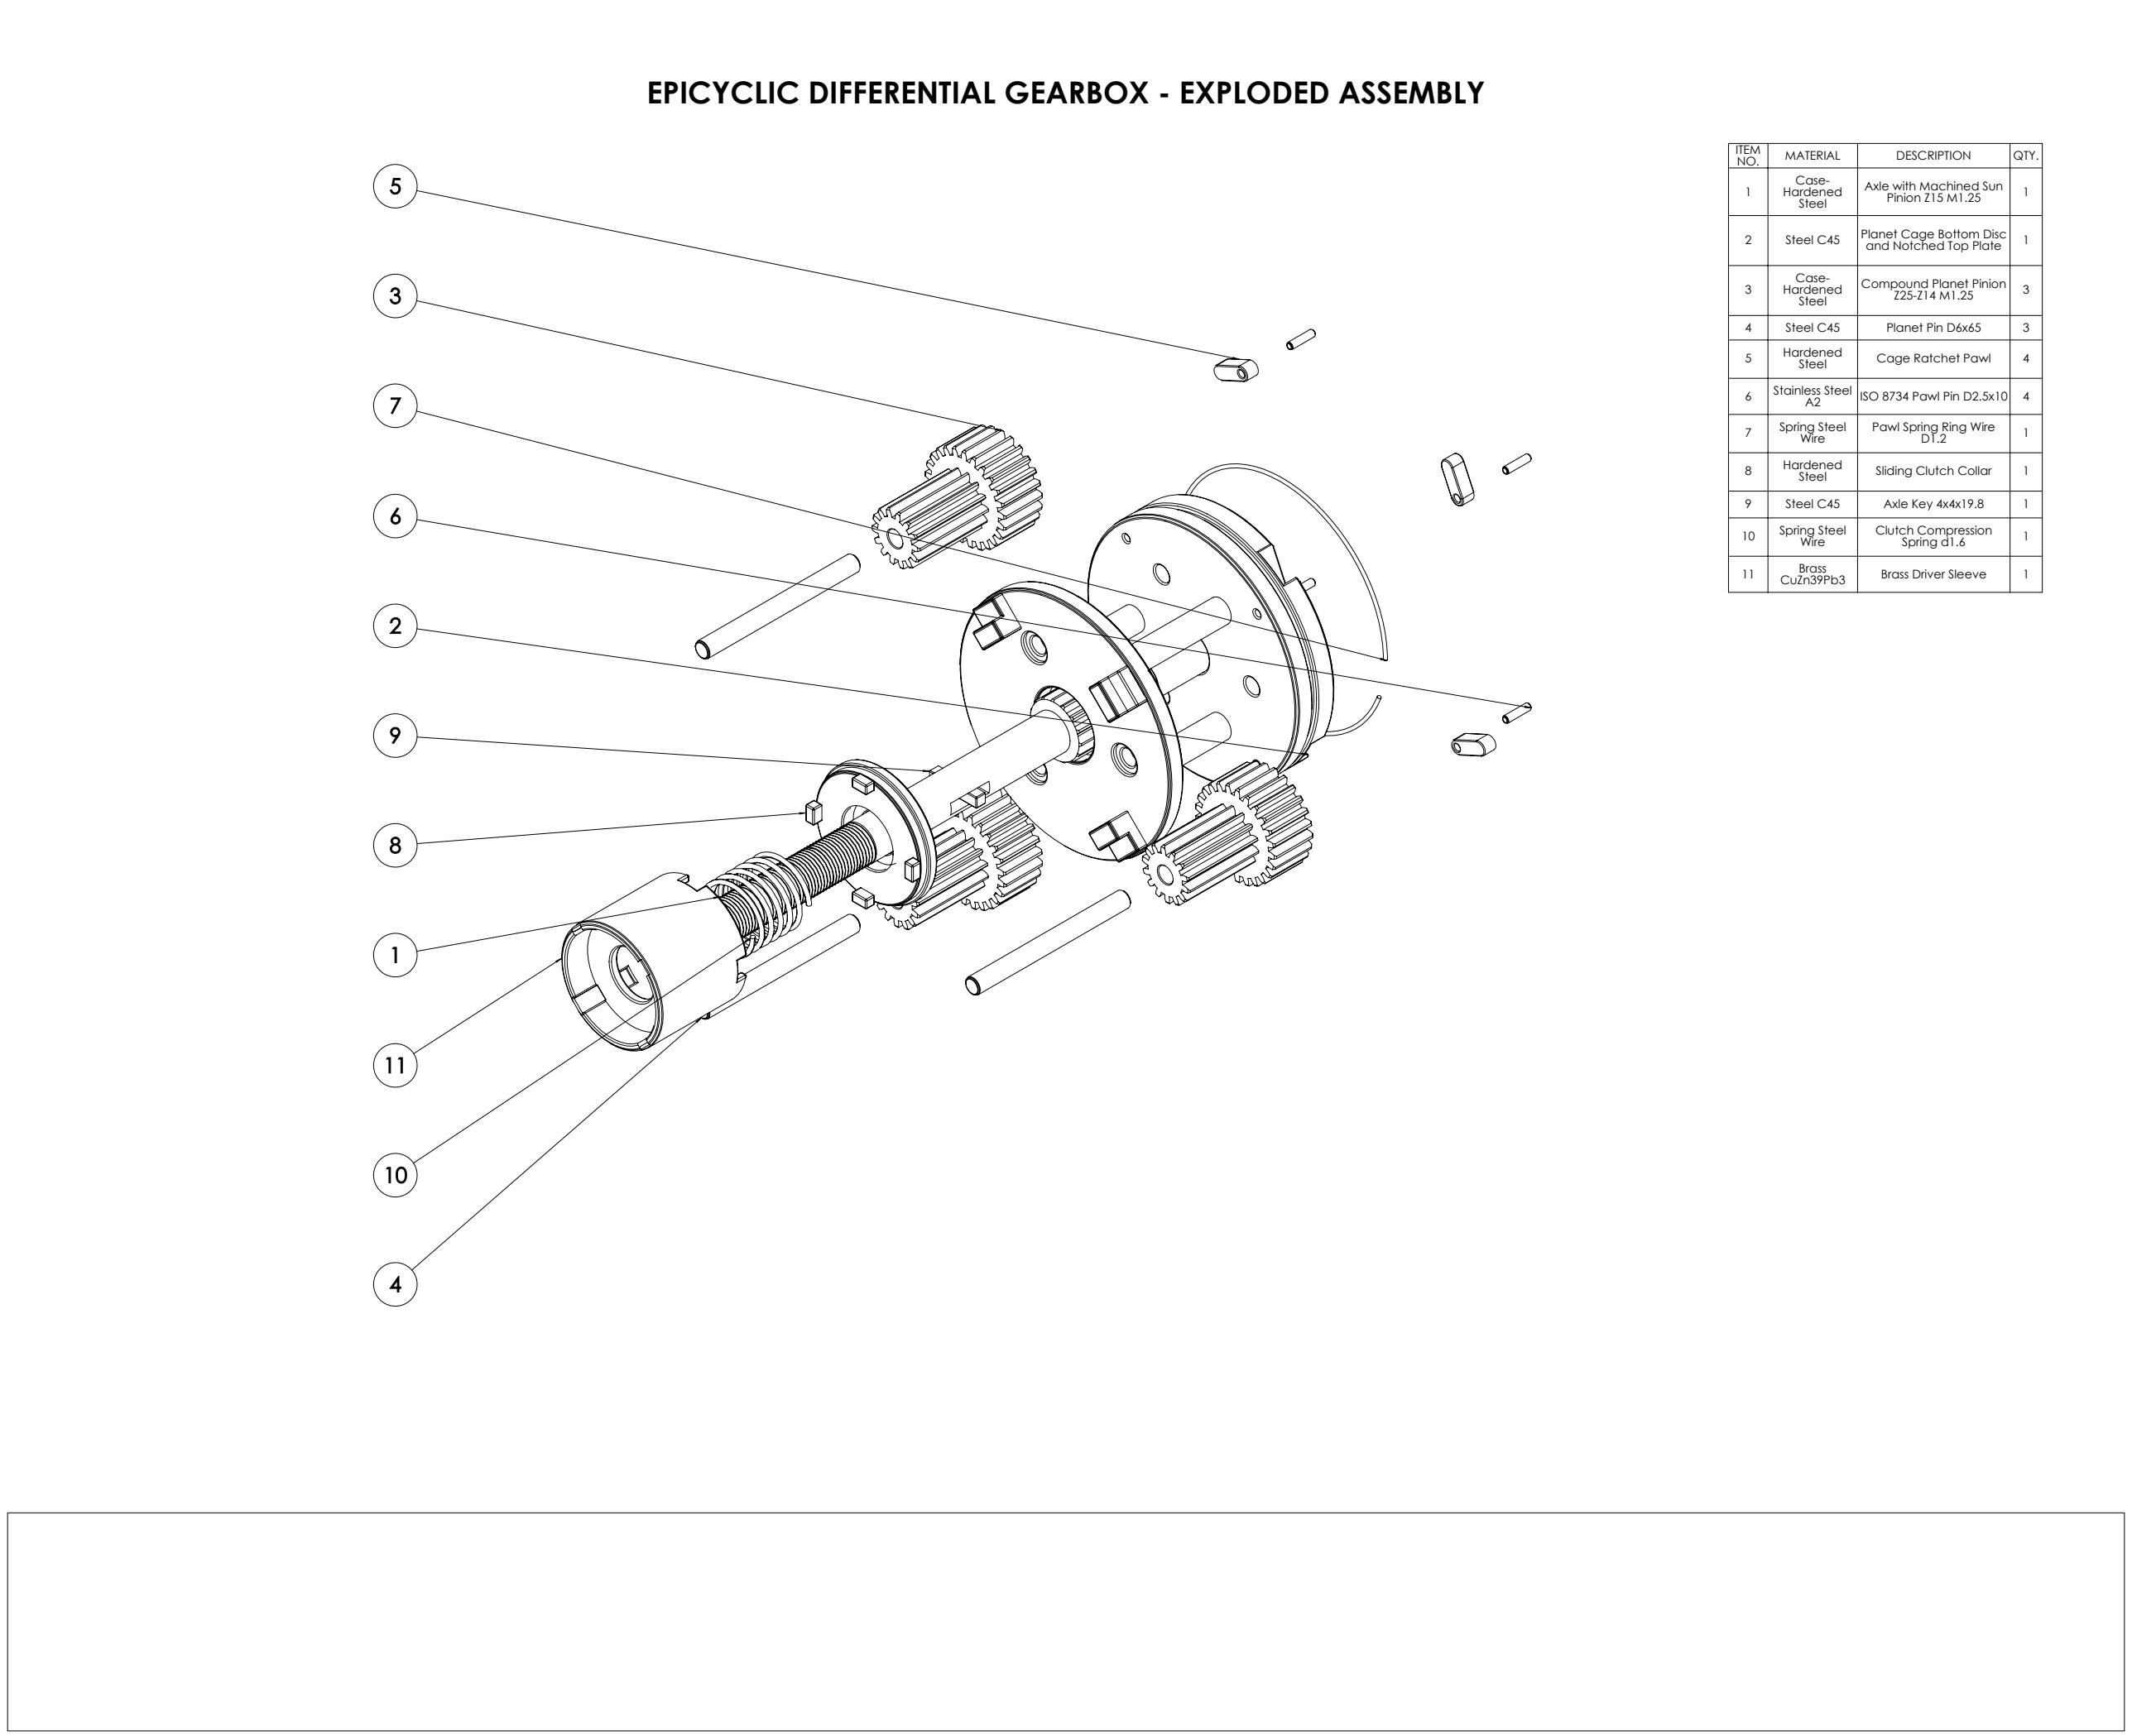
ISO-10303-21;
HEADER;
/* Generated by software containing ST-Developer
 * from STEP Tools, Inc. (www.steptools.com) 
 */

FILE_DESCRIPTION(
/* description */ (''),
/* implementation_level */ '2;1');

FILE_NAME(
/* name */ 'MAS-366',
/* time_stamp */ '2026-10-11T13:00:10-07:00',
/* author */ (''),
/* organization */ (''),
/* preprocessor_version */ 'ST-DEVELOPER v20.2',
/* originating_system */ 'Autodesk Translation Framework v15.15.0.0',
/* authorisation */ '');

FILE_SCHEMA (('AUTOMOTIVE_DESIGN { 1 0 10303 214 3 1 1 }'));
ENDSEC;

DATA;
#10=MECHANICAL_DESIGN_GEOMETRIC_PRESENTATION_REPRESENTATION('',(#358,#359,
#360,#361,#362,#363,#364,#365,#366,#367,#368),#65563);
#11=ITEM_DEFINED_TRANSFORMATION($,$,#20142,#22382);
#12=ITEM_DEFINED_TRANSFORMATION($,$,#20555,#22383);
#13=ITEM_DEFINED_TRANSFORMATION($,$,#21298,#22384);
#14=ITEM_DEFINED_TRANSFORMATION($,$,#21298,#22385);
#15=ITEM_DEFINED_TRANSFORMATION($,$,#21298,#22386);
#16=ITEM_DEFINED_TRANSFORMATION($,$,#21673,#22387);
#17=ITEM_DEFINED_TRANSFORMATION($,$,#21673,#22388);
#18=ITEM_DEFINED_TRANSFORMATION($,$,#21673,#22389);
#19=ITEM_DEFINED_TRANSFORMATION($,$,#21701,#22390);
#20=ITEM_DEFINED_TRANSFORMATION($,$,#21701,#22391);
#21=ITEM_DEFINED_TRANSFORMATION($,$,#21701,#22392);
#22=ITEM_DEFINED_TRANSFORMATION($,$,#21701,#22393);
#23=ITEM_DEFINED_TRANSFORMATION($,$,#21742,#22394);
#24=ITEM_DEFINED_TRANSFORMATION($,$,#21742,#22395);
#25=ITEM_DEFINED_TRANSFORMATION($,$,#21742,#22396);
#26=ITEM_DEFINED_TRANSFORMATION($,$,#21742,#22397);
#27=ITEM_DEFINED_TRANSFORMATION($,$,#21770,#22398);
#28=ITEM_DEFINED_TRANSFORMATION($,$,#21777,#22399);
#29=ITEM_DEFINED_TRANSFORMATION($,$,#22009,#22400);
#30=ITEM_DEFINED_TRANSFORMATION($,$,#22036,#22401);
#31=ITEM_DEFINED_TRANSFORMATION($,$,#22041,#22402);
#32=(
REPRESENTATION_RELATIONSHIP($,$,#65614,#65613)
REPRESENTATION_RELATIONSHIP_WITH_TRANSFORMATION(#11)
SHAPE_REPRESENTATION_RELATIONSHIP()
);
#33=(
REPRESENTATION_RELATIONSHIP($,$,#65615,#65613)
REPRESENTATION_RELATIONSHIP_WITH_TRANSFORMATION(#12)
SHAPE_REPRESENTATION_RELATIONSHIP()
);
#34=(
REPRESENTATION_RELATIONSHIP($,$,#65616,#65613)
REPRESENTATION_RELATIONSHIP_WITH_TRANSFORMATION(#13)
SHAPE_REPRESENTATION_RELATIONSHIP()
);
#35=(
REPRESENTATION_RELATIONSHIP($,$,#65616,#65613)
REPRESENTATION_RELATIONSHIP_WITH_TRANSFORMATION(#14)
SHAPE_REPRESENTATION_RELATIONSHIP()
);
#36=(
REPRESENTATION_RELATIONSHIP($,$,#65616,#65613)
REPRESENTATION_RELATIONSHIP_WITH_TRANSFORMATION(#15)
SHAPE_REPRESENTATION_RELATIONSHIP()
);
#37=(
REPRESENTATION_RELATIONSHIP($,$,#65617,#65613)
REPRESENTATION_RELATIONSHIP_WITH_TRANSFORMATION(#16)
SHAPE_REPRESENTATION_RELATIONSHIP()
);
#38=(
REPRESENTATION_RELATIONSHIP($,$,#65617,#65613)
REPRESENTATION_RELATIONSHIP_WITH_TRANSFORMATION(#17)
SHAPE_REPRESENTATION_RELATIONSHIP()
);
#39=(
REPRESENTATION_RELATIONSHIP($,$,#65617,#65613)
REPRESENTATION_RELATIONSHIP_WITH_TRANSFORMATION(#18)
SHAPE_REPRESENTATION_RELATIONSHIP()
);
#40=(
REPRESENTATION_RELATIONSHIP($,$,#65618,#65613)
REPRESENTATION_RELATIONSHIP_WITH_TRANSFORMATION(#19)
SHAPE_REPRESENTATION_RELATIONSHIP()
);
#41=(
REPRESENTATION_RELATIONSHIP($,$,#65618,#65613)
REPRESENTATION_RELATIONSHIP_WITH_TRANSFORMATION(#20)
SHAPE_REPRESENTATION_RELATIONSHIP()
);
#42=(
REPRESENTATION_RELATIONSHIP($,$,#65618,#65613)
REPRESENTATION_RELATIONSHIP_WITH_TRANSFORMATION(#21)
SHAPE_REPRESENTATION_RELATIONSHIP()
);
#43=(
REPRESENTATION_RELATIONSHIP($,$,#65618,#65613)
REPRESENTATION_RELATIONSHIP_WITH_TRANSFORMATION(#22)
SHAPE_REPRESENTATION_RELATIONSHIP()
);
#44=(
REPRESENTATION_RELATIONSHIP($,$,#65619,#65613)
REPRESENTATION_RELATIONSHIP_WITH_TRANSFORMATION(#23)
SHAPE_REPRESENTATION_RELATIONSHIP()
);
#45=(
REPRESENTATION_RELATIONSHIP($,$,#65619,#65613)
REPRESENTATION_RELATIONSHIP_WITH_TRANSFORMATION(#24)
SHAPE_REPRESENTATION_RELATIONSHIP()
);
#46=(
REPRESENTATION_RELATIONSHIP($,$,#65619,#65613)
REPRESENTATION_RELATIONSHIP_WITH_TRANSFORMATION(#25)
SHAPE_REPRESENTATION_RELATIONSHIP()
);
#47=(
REPRESENTATION_RELATIONSHIP($,$,#65619,#65613)
REPRESENTATION_RELATIONSHIP_WITH_TRANSFORMATION(#26)
SHAPE_REPRESENTATION_RELATIONSHIP()
);
#48=(
REPRESENTATION_RELATIONSHIP($,$,#65620,#65613)
REPRESENTATION_RELATIONSHIP_WITH_TRANSFORMATION(#27)
SHAPE_REPRESENTATION_RELATIONSHIP()
);
#49=(
REPRESENTATION_RELATIONSHIP($,$,#65621,#65613)
REPRESENTATION_RELATIONSHIP_WITH_TRANSFORMATION(#28)
SHAPE_REPRESENTATION_RELATIONSHIP()
);
#50=(
REPRESENTATION_RELATIONSHIP($,$,#65622,#65613)
REPRESENTATION_RELATIONSHIP_WITH_TRANSFORMATION(#29)
SHAPE_REPRESENTATION_RELATIONSHIP()
);
#51=(
REPRESENTATION_RELATIONSHIP($,$,#65623,#65613)
REPRESENTATION_RELATIONSHIP_WITH_TRANSFORMATION(#30)
SHAPE_REPRESENTATION_RELATIONSHIP()
);
#52=(
REPRESENTATION_RELATIONSHIP($,$,#65624,#65613)
REPRESENTATION_RELATIONSHIP_WITH_TRANSFORMATION(#31)
SHAPE_REPRESENTATION_RELATIONSHIP()
);
#53=CONTEXT_DEPENDENT_SHAPE_REPRESENTATION(#32,#65592);
#54=CONTEXT_DEPENDENT_SHAPE_REPRESENTATION(#33,#65593);
#55=CONTEXT_DEPENDENT_SHAPE_REPRESENTATION(#34,#65594);
#56=CONTEXT_DEPENDENT_SHAPE_REPRESENTATION(#35,#65595);
#57=CONTEXT_DEPENDENT_SHAPE_REPRESENTATION(#36,#65596);
#58=CONTEXT_DEPENDENT_SHAPE_REPRESENTATION(#37,#65597);
#59=CONTEXT_DEPENDENT_SHAPE_REPRESENTATION(#38,#65598);
#60=CONTEXT_DEPENDENT_SHAPE_REPRESENTATION(#39,#65599);
#61=CONTEXT_DEPENDENT_SHAPE_REPRESENTATION(#40,#65600);
#62=CONTEXT_DEPENDENT_SHAPE_REPRESENTATION(#41,#65601);
#63=CONTEXT_DEPENDENT_SHAPE_REPRESENTATION(#42,#65602);
#64=CONTEXT_DEPENDENT_SHAPE_REPRESENTATION(#43,#65603);
#65=CONTEXT_DEPENDENT_SHAPE_REPRESENTATION(#44,#65604);
#66=CONTEXT_DEPENDENT_SHAPE_REPRESENTATION(#45,#65605);
#67=CONTEXT_DEPENDENT_SHAPE_REPRESENTATION(#46,#65606);
#68=CONTEXT_DEPENDENT_SHAPE_REPRESENTATION(#47,#65607);
#69=CONTEXT_DEPENDENT_SHAPE_REPRESENTATION(#48,#65608);
#70=CONTEXT_DEPENDENT_SHAPE_REPRESENTATION(#49,#65609);
#71=CONTEXT_DEPENDENT_SHAPE_REPRESENTATION(#50,#65610);
#72=CONTEXT_DEPENDENT_SHAPE_REPRESENTATION(#51,#65611);
#73=CONTEXT_DEPENDENT_SHAPE_REPRESENTATION(#52,#65612);
#74=NEXT_ASSEMBLY_USAGE_OCCURRENCE(
'01_Axle_with_Machined_Sun_Pinion_Z15_M1.25:2',
'01_Axle_with_Machined_Sun_Pinion_Z15_M1.25:2',
'01_Axle_with_Machined_Sun_Pinion_Z15_M1.25:2',#65626,#65627,
'01_Axle_with_Machined_Sun_Pinion_Z15_M1.25:2');
#75=NEXT_ASSEMBLY_USAGE_OCCURRENCE(
'02_Planet_Cage_Bottom_Disc_and_Notched_Top_Plate:2',
'02_Planet_Cage_Bottom_Disc_and_Notched_Top_Plate:2',
'02_Planet_Cage_Bottom_Disc_and_Notched_Top_Plate:2',#65626,#65628,
'02_Planet_Cage_Bottom_Disc_and_Notched_Top_Plate:2');
#76=NEXT_ASSEMBLY_USAGE_OCCURRENCE(
'03_Compound_Planet_Pinion_Z25-Z14_M1.25:2',
'03_Compound_Planet_Pinion_Z25-Z14_M1.25:2',
'03_Compound_Planet_Pinion_Z25-Z14_M1.25:2',#65626,#65629,
'03_Compound_Planet_Pinion_Z25-Z14_M1.25:2');
#77=NEXT_ASSEMBLY_USAGE_OCCURRENCE(
'03_Compound_Planet_Pinion_Z25-Z14_M1.25:3',
'03_Compound_Planet_Pinion_Z25-Z14_M1.25:3',
'03_Compound_Planet_Pinion_Z25-Z14_M1.25:3',#65626,#65629,
'03_Compound_Planet_Pinion_Z25-Z14_M1.25:3');
#78=NEXT_ASSEMBLY_USAGE_OCCURRENCE(
'03_Compound_Planet_Pinion_Z25-Z14_M1.25:4',
'03_Compound_Planet_Pinion_Z25-Z14_M1.25:4',
'03_Compound_Planet_Pinion_Z25-Z14_M1.25:4',#65626,#65629,
'03_Compound_Planet_Pinion_Z25-Z14_M1.25:4');
#79=NEXT_ASSEMBLY_USAGE_OCCURRENCE('04_Planet_Pin_D6x65:2',
'04_Planet_Pin_D6x65:2','04_Planet_Pin_D6x65:2',#65626,#65630,
'04_Planet_Pin_D6x65:2');
#80=NEXT_ASSEMBLY_USAGE_OCCURRENCE('04_Planet_Pin_D6x65:3',
'04_Planet_Pin_D6x65:3','04_Planet_Pin_D6x65:3',#65626,#65630,
'04_Planet_Pin_D6x65:3');
#81=NEXT_ASSEMBLY_USAGE_OCCURRENCE('04_Planet_Pin_D6x65:4',
'04_Planet_Pin_D6x65:4','04_Planet_Pin_D6x65:4',#65626,#65630,
'04_Planet_Pin_D6x65:4');
#82=NEXT_ASSEMBLY_USAGE_OCCURRENCE('05_Cage_Ratchet_Pawl:2',
'05_Cage_Ratchet_Pawl:2','05_Cage_Ratchet_Pawl:2',#65626,#65631,
'05_Cage_Ratchet_Pawl:2');
#83=NEXT_ASSEMBLY_USAGE_OCCURRENCE('05_Cage_Ratchet_Pawl:3',
'05_Cage_Ratchet_Pawl:3','05_Cage_Ratchet_Pawl:3',#65626,#65631,
'05_Cage_Ratchet_Pawl:3');
#84=NEXT_ASSEMBLY_USAGE_OCCURRENCE('05_Cage_Ratchet_Pawl:4',
'05_Cage_Ratchet_Pawl:4','05_Cage_Ratchet_Pawl:4',#65626,#65631,
'05_Cage_Ratchet_Pawl:4');
#85=NEXT_ASSEMBLY_USAGE_OCCURRENCE('05_Cage_Ratchet_Pawl:5',
'05_Cage_Ratchet_Pawl:5','05_Cage_Ratchet_Pawl:5',#65626,#65631,
'05_Cage_Ratchet_Pawl:5');
#86=NEXT_ASSEMBLY_USAGE_OCCURRENCE('06_ISO_8734_Pawl_Pin_D2.5x10:2',
'06_ISO_8734_Pawl_Pin_D2.5x10:2','06_ISO_8734_Pawl_Pin_D2.5x10:2',#65626,
#65632,'06_ISO_8734_Pawl_Pin_D2.5x10:2');
#87=NEXT_ASSEMBLY_USAGE_OCCURRENCE('06_ISO_8734_Pawl_Pin_D2.5x10:3',
'06_ISO_8734_Pawl_Pin_D2.5x10:3','06_ISO_8734_Pawl_Pin_D2.5x10:3',#65626,
#65632,'06_ISO_8734_Pawl_Pin_D2.5x10:3');
#88=NEXT_ASSEMBLY_USAGE_OCCURRENCE('06_ISO_8734_Pawl_Pin_D2.5x10:4',
'06_ISO_8734_Pawl_Pin_D2.5x10:4','06_ISO_8734_Pawl_Pin_D2.5x10:4',#65626,
#65632,'06_ISO_8734_Pawl_Pin_D2.5x10:4');
#89=NEXT_ASSEMBLY_USAGE_OCCURRENCE('06_ISO_8734_Pawl_Pin_D2.5x10:5',
'06_ISO_8734_Pawl_Pin_D2.5x10:5','06_ISO_8734_Pawl_Pin_D2.5x10:5',#65626,
#65632,'06_ISO_8734_Pawl_Pin_D2.5x10:5');
#90=NEXT_ASSEMBLY_USAGE_OCCURRENCE('07_Pawl_Spring_Ring_Wire_D1.2:2',
'07_Pawl_Spring_Ring_Wire_D1.2:2','07_Pawl_Spring_Ring_Wire_D1.2:2',#65626,
#65633,'07_Pawl_Spring_Ring_Wire_D1.2:2');
#91=NEXT_ASSEMBLY_USAGE_OCCURRENCE('08_Sliding_Clutch_Collar:2',
'08_Sliding_Clutch_Collar:2','08_Sliding_Clutch_Collar:2',#65626,#65634,
'08_Sliding_Clutch_Collar:2');
#92=NEXT_ASSEMBLY_USAGE_OCCURRENCE('09_Axle_Key_4x4x19.8:2',
'09_Axle_Key_4x4x19.8:2','09_Axle_Key_4x4x19.8:2',#65626,#65635,
'09_Axle_Key_4x4x19.8:2');
#93=NEXT_ASSEMBLY_USAGE_OCCURRENCE(
'10_Clutch_Compression_Spring_d1.6:2',
'10_Clutch_Compression_Spring_d1.6:2',
'10_Clutch_Compression_Spring_d1.6:2',#65626,#65636,
'10_Clutch_Compression_Spring_d1.6:2');
#94=NEXT_ASSEMBLY_USAGE_OCCURRENCE('11_Brass_Driver_Sleeve:2',
'11_Brass_Driver_Sleeve:2','11_Brass_Driver_Sleeve:2',#65626,#65637,
'11_Brass_Driver_Sleeve:2');
#95=TOROIDAL_SURFACE('',#20843,43.5,0.5);
#96=TOROIDAL_SURFACE('',#20862,3.5,0.5);
#97=TOROIDAL_SURFACE('',#20886,42.9928932188135,0.5);
#98=TOROIDAL_SURFACE('',#20891,43.5,0.5);
#99=TOROIDAL_SURFACE('',#20897,3.5,0.5);
#100=TOROIDAL_SURFACE('',#20902,42.9928932188135,0.5);
#101=TOROIDAL_SURFACE('',#20905,42.9928932188135,0.5);
#102=TOROIDAL_SURFACE('',#20926,43.5,0.5);
#103=TOROIDAL_SURFACE('',#20929,43.5,0.5);
#104=TOROIDAL_SURFACE('',#20951,43.5,0.5);
#105=TOROIDAL_SURFACE('',#20956,43.5,0.5);
#106=TOROIDAL_SURFACE('',#20967,42.9928932188135,0.5);
#107=TOROIDAL_SURFACE('',#20971,3.5,0.5);
#108=TOROIDAL_SURFACE('',#20981,3.5,0.5);
#109=TOROIDAL_SURFACE('',#20985,1.75,0.5);
#110=TOROIDAL_SURFACE('',#21020,43.5,0.5);
#111=TOROIDAL_SURFACE('',#21025,1.75,0.5);
#112=TOROIDAL_SURFACE('',#21059,43.5,0.5);
#113=TOROIDAL_SURFACE('',#21069,43.5,0.5);
#114=TOROIDAL_SURFACE('',#21076,43.5,0.5);
#115=TOROIDAL_SURFACE('',#21081,43.5,0.5);
#116=TOROIDAL_SURFACE('',#21097,1.75,0.5);
#117=TOROIDAL_SURFACE('',#21103,1.75,0.5);
#118=TOROIDAL_SURFACE('',#21109,3.5,0.5);
#119=TOROIDAL_SURFACE('',#21128,3.5,0.5);
#120=TOROIDAL_SURFACE('',#21134,42.9928932188134,0.5);
#121=TOROIDAL_SURFACE('',#21136,1.75,0.5);
#122=TOROIDAL_SURFACE('',#21138,1.75,0.5);
#123=TOROIDAL_SURFACE('',#21140,3.5,0.5);
#124=TOROIDAL_SURFACE('',#21146,1.75,0.5);
#125=TOROIDAL_SURFACE('',#21148,1.75,0.5);
#126=TOROIDAL_SURFACE('',#21150,3.5,0.5);
#127=TOROIDAL_SURFACE('',#21158,3.5,0.5);
#128=TOROIDAL_SURFACE('',#21166,3.5,0.5);
#129=TOROIDAL_SURFACE('',#21183,43.5,0.5);
#130=TOROIDAL_SURFACE('',#21195,43.1928932188135,0.5);
#131=TOROIDAL_SURFACE('',#21206,3.5,0.5);
#132=TOROIDAL_SURFACE('',#21208,3.5,0.5);
#133=TOROIDAL_SURFACE('',#21210,3.5,0.5);
#134=TOROIDAL_SURFACE('',#21212,7.55,0.5);
#135=TOROIDAL_SURFACE('',#21219,7.75710678118654,0.5);
#136=TOROIDAL_SURFACE('',#21226,7.55,0.5);
#137=TOROIDAL_SURFACE('',#21228,12.5,0.5);
#138=TOROIDAL_SURFACE('',#21235,43.5,0.5);
#139=TOROIDAL_SURFACE('',#21243,43.1928932188135,0.5);
#140=TOROIDAL_SURFACE('',#21251,5.5,0.5);
#141=TOROIDAL_SURFACE('',#21261,5.5,0.5);
#142=TOROIDAL_SURFACE('',#21266,5.5,0.5);
#143=TOROIDAL_SURFACE('',#21271,12.5,0.5);
#144=TOROIDAL_SURFACE('',#21278,12.7071067811865,0.5);
#145=TOROIDAL_SURFACE('',#21674,2.47573593128807,0.3);
#146=TOROIDAL_SURFACE('',#21683,2.7,0.3);
#147=TOROIDAL_SURFACE('',#21690,2.7,0.3);
#148=TOROIDAL_SURFACE('',#21697,2.47573593128807,0.3);
#149=TOROIDAL_SURFACE('',#21705,2.2,0.3);
#150=TOROIDAL_SURFACE('',#21711,2.2,0.3);
#151=TOROIDAL_SURFACE('',#21722,2.2,0.3);
#152=TOROIDAL_SURFACE('',#21728,2.2,0.3);
#153=TOROIDAL_SURFACE('',#21733,1.575,0.3);
#154=TOROIDAL_SURFACE('',#21739,1.575,0.3);
#155=TOROIDAL_SURFACE('',#21743,0.867157287525381,0.2);
#156=TOROIDAL_SURFACE('',#21752,1.05,0.2);
#157=TOROIDAL_SURFACE('',#21759,1.05,0.2);
#158=TOROIDAL_SURFACE('',#21766,0.867157287525381,0.2);
#159=TOROIDAL_SURFACE('',#21771,43.2,0.599999999999996);
#160=TOROIDAL_SURFACE('',#21892,21.1343145750508,0.4);
#161=TOROIDAL_SURFACE('',#21909,22.6,0.4);
#162=TOROIDAL_SURFACE('',#21951,22.6,0.4);
#163=TOROIDAL_SURFACE('',#21958,21.4,0.4);
#164=TOROIDAL_SURFACE('',#21963,10.7968626966597,0.4);
#165=TOROIDAL_SURFACE('',#21966,22.2343145750508,0.4);
#166=TOROIDAL_SURFACE('',#21990,7.45,0.4);
#167=TOROIDAL_SURFACE('',#21997,7.45,0.4);
#168=TOROIDAL_SURFACE('',#22042,9.5,0.5);
#169=TOROIDAL_SURFACE('',#22064,9.5,0.5);
#170=TOROIDAL_SURFACE('',#22095,20.2928932188135,0.5);
#171=TOROIDAL_SURFACE('',#22125,20.5,0.5);
#172=TOROIDAL_SURFACE('',#22149,20.5,0.5);
#173=TOROIDAL_SURFACE('',#22154,20.2928932188135,0.5);
#174=TOROIDAL_SURFACE('',#22157,20.5,0.5);
#175=TOROIDAL_SURFACE('',#22166,20.5,0.5);
#176=TOROIDAL_SURFACE('',#22186,20.5,0.5);
#177=TOROIDAL_SURFACE('',#22207,20.5,0.5);
#178=TOROIDAL_SURFACE('',#22220,20.5,0.5);
#179=TOROIDAL_SURFACE('',#22225,19.,0.5);
#180=TOROIDAL_SURFACE('',#22227,19.,0.5);
#181=TOROIDAL_SURFACE('',#22231,19.,0.5);
#182=TOROIDAL_SURFACE('',#22248,19.,0.5);
#183=TOROIDAL_SURFACE('',#22252,19.,0.5);
#184=TOROIDAL_SURFACE('',#22256,19.,0.5);
#185=TOROIDAL_SURFACE('',#22263,19.,0.5);
#186=TOROIDAL_SURFACE('',#22264,19.,0.5);
#187=TOROIDAL_SURFACE('',#22265,19.,0.5);
#188=TOROIDAL_SURFACE('',#22275,20.2928932188135,0.5);
#189=TOROIDAL_SURFACE('',#22289,19.,0.5);
#190=TOROIDAL_SURFACE('',#22299,19.,0.5);
#191=TOROIDAL_SURFACE('',#22302,20.5,0.5);
#192=TOROIDAL_SURFACE('',#22320,19.,0.5);
#193=TOROIDAL_SURFACE('',#22331,19.9928932188135,0.5);
#194=TOROIDAL_SURFACE('',#22335,19.,0.5);
#195=TOROIDAL_SURFACE('',#22338,19.9928932188135,0.5);
#196=TOROIDAL_SURFACE('',#22342,19.,0.5);
#197=TOROIDAL_SURFACE('',#22348,19.,0.5);
#198=TOROIDAL_SURFACE('',#22361,19.9928932188135,0.5);
#199=TOROIDAL_SURFACE('',#22372,19.,0.5);
#200=ELLIPSE('',#20602,0.707106781186548,0.5);
#201=ELLIPSE('',#20603,0.707106781186549,0.5);
#202=ELLIPSE('',#20642,0.707106781186549,0.5);
#203=ELLIPSE('',#20643,0.707106781186543,0.5);
#204=ELLIPSE('',#20698,0.707106781186547,0.5);
#205=ELLIPSE('',#20715,0.707106781186547,0.5);
#206=ELLIPSE('',#20745,1.08766387358053,0.5);
#207=ELLIPSE('',#20747,0.563016250305246,0.5);
#208=ELLIPSE('',#20752,0.70710678118655,0.499999999999999);
#209=ELLIPSE('',#20753,0.707106781186547,0.5);
#210=ELLIPSE('',#20756,0.707106781186549,0.5);
#211=ELLIPSE('',#20759,0.707106781186548,0.5);
#212=ELLIPSE('',#20790,0.524647623275289,0.499999999999999);
#213=ELLIPSE('',#20791,1.08766387358054,0.499999999999999);
#214=ELLIPSE('',#20799,0.541196100146196,0.5);
#215=ELLIPSE('',#20808,0.707106781186548,0.5);
#216=ELLIPSE('',#20818,0.541196100146196,0.5);
#217=ELLIPSE('',#20819,0.707106781186546,0.5);
#218=ELLIPSE('',#20822,0.999999999999998,0.499999999999999);
#219=ELLIPSE('',#20832,0.707106781186548,0.5);
#220=ELLIPSE('',#20901,0.707106781186546,0.5);
#221=ELLIPSE('',#20996,0.707106781186545,0.5);
#222=ELLIPSE('',#21001,0.563016250305243,0.5);
#223=ELLIPSE('',#21002,0.563016250305246,0.5);
#224=ELLIPSE('',#21003,0.707106781186547,0.5);
#225=ELLIPSE('',#21004,0.707106781186543,0.5);
#226=ELLIPSE('',#21007,0.563016250305245,0.499999999999997);
#227=ELLIPSE('',#21010,0.563016250305245,0.499999999999999);
#228=ELLIPSE('',#21017,0.999999999999989,0.499999999999997);
#229=ELLIPSE('',#21019,0.707106781186552,0.5);
#230=ELLIPSE('',#21057,0.707106781186546,0.5);
#231=ELLIPSE('',#21087,0.541196100146194,0.5);
#232=ELLIPSE('',#21096,0.707106781186549,0.5);
#233=ELLIPSE('',#21780,0.565685424949238,0.4);
#234=ELLIPSE('',#21783,0.565685424949238,0.4);
#235=ELLIPSE('',#21819,0.565685424949238,0.4);
#236=ELLIPSE('',#21828,0.565685424949238,0.4);
#237=ELLIPSE('',#21872,0.565685424949238,0.4);
#238=ELLIPSE('',#21877,0.565685424949238,0.4);
#239=ELLIPSE('',#21929,0.565685424949238,0.4);
#240=ELLIPSE('',#21973,0.565685424949238,0.4);
#241=ELLIPSE('',#22319,0.707106781186544,0.5);
#242=ELLIPSE('',#22352,0.70710678118655,0.5);
#243=SPHERICAL_SURFACE('',#20559,0.5);
#244=SPHERICAL_SURFACE('',#20569,0.5);
#245=SPHERICAL_SURFACE('',#20571,0.5);
#246=SPHERICAL_SURFACE('',#20581,0.5);
#247=SPHERICAL_SURFACE('',#20595,0.5);
#248=SPHERICAL_SURFACE('',#20605,0.5);
#249=SPHERICAL_SURFACE('',#20612,0.5);
#250=SPHERICAL_SURFACE('',#20617,0.5);
#251=SPHERICAL_SURFACE('',#20631,0.5);
#252=SPHERICAL_SURFACE('',#20637,0.5);
#253=SPHERICAL_SURFACE('',#20646,0.5);
#254=SPHERICAL_SURFACE('',#20654,0.5);
#255=SPHERICAL_SURFACE('',#20665,0.5);
#256=SPHERICAL_SURFACE('',#20674,0.5);
#257=SPHERICAL_SURFACE('',#20679,0.5);
#258=SPHERICAL_SURFACE('',#20683,0.5);
#259=SPHERICAL_SURFACE('',#20702,0.5);
#260=SPHERICAL_SURFACE('',#20708,0.5);
#261=SPHERICAL_SURFACE('',#20722,0.5);
#262=SPHERICAL_SURFACE('',#20726,0.5);
#263=SPHERICAL_SURFACE('',#20732,0.5);
#264=SPHERICAL_SURFACE('',#20737,0.5);
#265=SPHERICAL_SURFACE('',#20748,0.5);
#266=SPHERICAL_SURFACE('',#20764,0.5);
#267=SPHERICAL_SURFACE('',#20768,0.5);
#268=SPHERICAL_SURFACE('',#20784,0.5);
#269=SPHERICAL_SURFACE('',#20787,0.5);
#270=SPHERICAL_SURFACE('',#20809,0.5);
#271=SPHERICAL_SURFACE('',#20824,0.5);
#272=SPHERICAL_SURFACE('',#20827,0.5);
#273=SPHERICAL_SURFACE('',#20836,0.5);
#274=SPHERICAL_SURFACE('',#20841,0.5);
#275=SPHERICAL_SURFACE('',#20868,0.5);
#276=SPHERICAL_SURFACE('',#20871,0.5);
#277=SPHERICAL_SURFACE('',#20914,0.5);
#278=SPHERICAL_SURFACE('',#20920,0.5);
#279=SPHERICAL_SURFACE('',#20934,0.5);
#280=SPHERICAL_SURFACE('',#20936,0.5);
#281=SPHERICAL_SURFACE('',#20946,0.5);
#282=SPHERICAL_SURFACE('',#20949,0.5);
#283=SPHERICAL_SURFACE('',#20961,0.500000000000003);
#284=SPHERICAL_SURFACE('',#20975,0.5);
#285=SPHERICAL_SURFACE('',#20991,0.5);
#286=SPHERICAL_SURFACE('',#21034,0.5);
#287=SPHERICAL_SURFACE('',#21038,0.5);
#288=SPHERICAL_SURFACE('',#21042,0.5);
#289=SPHERICAL_SURFACE('',#21053,0.5);
#290=SPHERICAL_SURFACE('',#21092,0.5);
#291=SPHERICAL_SURFACE('',#21178,0.5);
#292=SPHERICAL_SURFACE('',#21784,0.4);
#293=SPHERICAL_SURFACE('',#21791,0.4);
#294=SPHERICAL_SURFACE('',#21794,0.4);
#295=SPHERICAL_SURFACE('',#21799,0.4);
#296=SPHERICAL_SURFACE('',#21809,0.4);
#297=SPHERICAL_SURFACE('',#21823,0.4);
#298=SPHERICAL_SURFACE('',#21831,0.4);
#299=SPHERICAL_SURFACE('',#21833,0.4);
#300=SPHERICAL_SURFACE('',#21840,0.4);
#301=SPHERICAL_SURFACE('',#21846,0.4);
#302=SPHERICAL_SURFACE('',#21859,0.4);
#303=SPHERICAL_SURFACE('',#21862,0.4);
#304=SPHERICAL_SURFACE('',#21879,0.4);
#305=SPHERICAL_SURFACE('',#21881,0.4);
#306=SPHERICAL_SURFACE('',#21919,0.4);
#307=SPHERICAL_SURFACE('',#21925,0.4);
#308=SPHERICAL_SURFACE('',#21937,0.4);
#309=SPHERICAL_SURFACE('',#21940,0.4);
#310=SPHERICAL_SURFACE('',#21942,0.4);
#311=SPHERICAL_SURFACE('',#21974,0.4);
#312=SPHERICAL_SURFACE('',#21982,0.4);
#313=SPHERICAL_SURFACE('',#21985,0.4);
#314=SPHERICAL_SURFACE('',#22100,0.5);
#315=SPHERICAL_SURFACE('',#22106,0.5);
#316=SPHERICAL_SURFACE('',#22109,0.5);
#317=SPHERICAL_SURFACE('',#22121,0.5);
#318=SPHERICAL_SURFACE('',#22142,0.5);
#319=SPHERICAL_SURFACE('',#22145,0.5);
#320=SPHERICAL_SURFACE('',#22162,0.5);
#321=SPHERICAL_SURFACE('',#22170,0.5);
#322=SPHERICAL_SURFACE('',#22173,0.5);
#323=SPHERICAL_SURFACE('',#22176,0.5);
#324=SPHERICAL_SURFACE('',#22191,0.5);
#325=SPHERICAL_SURFACE('',#22193,0.5);
#326=SPHERICAL_SURFACE('',#22200,0.5);
#327=SPHERICAL_SURFACE('',#22209,0.5);
#328=SPHERICAL_SURFACE('',#22217,0.5);
#329=SPHERICAL_SURFACE('',#22233,0.5);
#330=SPHERICAL_SURFACE('',#22259,0.5);
#331=SPHERICAL_SURFACE('',#22271,0.5);
#332=SPHERICAL_SURFACE('',#22282,0.500000000000002);
#333=SPHERICAL_SURFACE('',#22285,0.5);
#334=SPHERICAL_SURFACE('',#22324,0.5);
#335=SPHERICAL_SURFACE('',#22354,0.5);
#336=SHAPE_REPRESENTATION_RELATIONSHIP('SRR','None',#65614,#347);
#337=SHAPE_REPRESENTATION_RELATIONSHIP('SRR','None',#65615,#348);
#338=SHAPE_REPRESENTATION_RELATIONSHIP('SRR','None',#65616,#349);
#339=SHAPE_REPRESENTATION_RELATIONSHIP('SRR','None',#65617,#350);
#340=SHAPE_REPRESENTATION_RELATIONSHIP('SRR','None',#65618,#351);
#341=SHAPE_REPRESENTATION_RELATIONSHIP('SRR','None',#65619,#352);
#342=SHAPE_REPRESENTATION_RELATIONSHIP('SRR','None',#65620,#353);
#343=SHAPE_REPRESENTATION_RELATIONSHIP('SRR','None',#65621,#354);
#344=SHAPE_REPRESENTATION_RELATIONSHIP('SRR','None',#65622,#355);
#345=SHAPE_REPRESENTATION_RELATIONSHIP('SRR','None',#65623,#356);
#346=SHAPE_REPRESENTATION_RELATIONSHIP('SRR','None',#65624,#357);
#347=ADVANCED_BREP_SHAPE_REPRESENTATION('',(#369),#65552);
#348=ADVANCED_BREP_SHAPE_REPRESENTATION('',(#370),#65553);
#349=ADVANCED_BREP_SHAPE_REPRESENTATION('',(#371),#65554);
#350=ADVANCED_BREP_SHAPE_REPRESENTATION('',(#372),#65555);
#351=ADVANCED_BREP_SHAPE_REPRESENTATION('',(#373),#65556);
#352=ADVANCED_BREP_SHAPE_REPRESENTATION('',(#374),#65557);
#353=ADVANCED_BREP_SHAPE_REPRESENTATION('',(#375),#65558);
#354=ADVANCED_BREP_SHAPE_REPRESENTATION('',(#376),#65559);
#355=ADVANCED_BREP_SHAPE_REPRESENTATION('',(#377),#65560);
#356=ADVANCED_BREP_SHAPE_REPRESENTATION('',(#378),#65561);
#357=ADVANCED_BREP_SHAPE_REPRESENTATION('',(#379),#65562);
#358=STYLED_ITEM('',(#65788),#369);
#359=STYLED_ITEM('',(#65802),#370);
#360=STYLED_ITEM('',(#65802),#371);
#361=STYLED_ITEM('',(#65788),#372);
#362=STYLED_ITEM('',(#65781),#373);
#363=STYLED_ITEM('',(#65788),#374);
#364=STYLED_ITEM('',(#65788),#375);
#365=STYLED_ITEM('',(#65802),#376);
#366=STYLED_ITEM('',(#65788),#377);
#367=STYLED_ITEM('',(#65788),#378);
#368=STYLED_ITEM('',(#65802),#379);
#369=MANIFOLD_SOLID_BREP('Body1',#20008);
#370=MANIFOLD_SOLID_BREP('Body1',#20009);
#371=MANIFOLD_SOLID_BREP('Body1',#20010);
#372=MANIFOLD_SOLID_BREP('Body1',#20011);
#373=MANIFOLD_SOLID_BREP('Body1',#20012);
#374=MANIFOLD_SOLID_BREP('Body1',#20013);
#375=MANIFOLD_SOLID_BREP('Body1',#20014);
#376=MANIFOLD_SOLID_BREP('Body1',#20015);
#377=MANIFOLD_SOLID_BREP('Body1',#20016);
#378=MANIFOLD_SOLID_BREP('Body1',#20017);
#379=MANIFOLD_SOLID_BREP('Body1',#20018);
#380=CONICAL_SURFACE('',#20340,10.375,0.785398163397451);
#381=CONICAL_SURFACE('',#20343,10.375,0.785398163397451);
#382=CONICAL_SURFACE('',#20348,10.375,0.785398163397451);
#383=CONICAL_SURFACE('',#20357,10.375,0.785398163397451);
#384=CONICAL_SURFACE('',#20362,10.375,0.785398163397451);
#385=CONICAL_SURFACE('',#20371,10.375,0.785398163397451);
#386=CONICAL_SURFACE('',#20376,10.375,0.785398163397451);
#387=CONICAL_SURFACE('',#20385,10.375,0.785398163397451);
#388=CONICAL_SURFACE('',#20390,10.375,0.785398163397451);
#389=CONICAL_SURFACE('',#20399,10.375,0.785398163397451);
#390=CONICAL_SURFACE('',#20404,10.375,0.785398163397451);
#391=CONICAL_SURFACE('',#20413,10.375,0.785398163397451);
#392=CONICAL_SURFACE('',#20418,10.375,0.785398163397451);
#393=CONICAL_SURFACE('',#20427,10.375,0.785398163397451);
#394=CONICAL_SURFACE('',#20432,10.375,0.785398163397451);
#395=CONICAL_SURFACE('',#20443,10.375,0.785398163397451);
#396=CONICAL_SURFACE('',#20448,10.375,0.785398163397451);
#397=CONICAL_SURFACE('',#20457,10.375,0.785398163397451);
#398=CONICAL_SURFACE('',#20462,10.375,0.785398163397451);
#399=CONICAL_SURFACE('',#20471,10.375,0.785398163397451);
#400=CONICAL_SURFACE('',#20476,10.375,0.785398163397451);
#401=CONICAL_SURFACE('',#20485,10.375,0.785398163397451);
#402=CONICAL_SURFACE('',#20490,10.375,0.785398163397451);
#403=CONICAL_SURFACE('',#20499,10.375,0.785398163397451);
#404=CONICAL_SURFACE('',#20504,10.375,0.785398163397451);
#405=CONICAL_SURFACE('',#20513,10.375,0.785398163397451);
#406=CONICAL_SURFACE('',#20518,10.375,0.785398163397451);
#407=CONICAL_SURFACE('',#20527,10.375,0.785398163397451);
#408=CONICAL_SURFACE('',#20532,10.375,0.785398163397451);
#409=CONICAL_SURFACE('',#20541,10.375,0.785398163397451);
#410=CONICAL_SURFACE('',#20547,6.5,0.78539816339745);
#411=CONICAL_SURFACE('',#20548,8.5625,1.41214106460849);
#412=CONICAL_SURFACE('',#20549,8.5625,1.4121410646085);
#413=CONICAL_SURFACE('',#20552,6.5,0.78539816339745);
#414=CONICAL_SURFACE('',#20889,43.6,0.785398163397448);
#415=CONICAL_SURFACE('',#20908,43.6,0.785398163397448);
#416=CONICAL_SURFACE('',#20924,43.6,0.785398163397448);
#417=CONICAL_SURFACE('',#20954,43.6,0.785398163397448);
#418=CONICAL_SURFACE('',#21073,43.6,0.785398163397454);
#419=CONICAL_SURFACE('',#21189,43.7,0.785398163397452);
#420=CONICAL_SURFACE('',#21223,7.3,0.785398163397442);
#421=CONICAL_SURFACE('',#21239,43.7,0.785398163397452);
#422=CONICAL_SURFACE('',#21275,12.25,0.785398163397448);
#423=CONICAL_SURFACE('',#21299,3.18,0.785398163397451);
#424=CONICAL_SURFACE('',#21335,3.18,0.785398163397444);
#425=CONICAL_SURFACE('',#21390,9.75,0.785398163397451);
#426=CONICAL_SURFACE('',#21474,9.75,0.785398163397451);
#427=CONICAL_SURFACE('',#21476,9.75,0.785398163397451);
#428=CONICAL_SURFACE('',#21482,9.75,0.785398163397451);
#429=CONICAL_SURFACE('',#21484,9.75,0.785398163397451);
#430=CONICAL_SURFACE('',#21490,9.75,0.785398163397451);
#431=CONICAL_SURFACE('',#21492,9.75,0.785398163397451);
#432=CONICAL_SURFACE('',#21498,9.75,0.785398163397451);
#433=CONICAL_SURFACE('',#21500,9.75,0.785398163397451);
#434=CONICAL_SURFACE('',#21506,9.75,0.785398163397451);
#435=CONICAL_SURFACE('',#21508,9.75,0.785398163397451);
#436=CONICAL_SURFACE('',#21514,9.75,0.785398163397451);
#437=CONICAL_SURFACE('',#21516,9.75,0.785398163397451);
#438=CONICAL_SURFACE('',#21521,16.625,0.785398163397451);
#439=CONICAL_SURFACE('',#21525,16.625,0.785398163397451);
#440=CONICAL_SURFACE('',#21527,16.625,0.785398163397451);
#441=CONICAL_SURFACE('',#21531,16.625,0.785398163397451);
#442=CONICAL_SURFACE('',#21533,16.625,0.785398163397451);
#443=CONICAL_SURFACE('',#21537,16.625,0.785398163397451);
#444=CONICAL_SURFACE('',#21539,16.625,0.785398163397451);
#445=CONICAL_SURFACE('',#21543,16.625,0.785398163397451);
#446=CONICAL_SURFACE('',#21545,16.625,0.785398163397451);
#447=CONICAL_SURFACE('',#21549,16.625,0.785398163397451);
#448=CONICAL_SURFACE('',#21551,16.625,0.785398163397451);
#449=CONICAL_SURFACE('',#21555,16.625,0.785398163397451);
#450=CONICAL_SURFACE('',#21557,16.625,0.785398163397451);
#451=CONICAL_SURFACE('',#21561,16.625,0.785398163397451);
#452=CONICAL_SURFACE('',#21563,16.625,0.785398163397451);
#453=CONICAL_SURFACE('',#21567,16.625,0.785398163397451);
#454=CONICAL_SURFACE('',#21569,16.625,0.785398163397451);
#455=CONICAL_SURFACE('',#21573,16.625,0.785398163397451);
#456=CONICAL_SURFACE('',#21575,16.625,0.785398163397451);
#457=CONICAL_SURFACE('',#21579,16.625,0.785398163397451);
#458=CONICAL_SURFACE('',#21581,16.625,0.785398163397451);
#459=CONICAL_SURFACE('',#21585,16.625,0.785398163397451);
#460=CONICAL_SURFACE('',#21587,16.625,0.785398163397451);
#461=CONICAL_SURFACE('',#21591,16.625,0.785398163397451);
#462=CONICAL_SURFACE('',#21593,16.625,0.785398163397451);
#463=CONICAL_SURFACE('',#21597,16.625,0.785398163397451);
#464=CONICAL_SURFACE('',#21599,16.625,0.785398163397451);
#465=CONICAL_SURFACE('',#21603,16.625,0.785398163397451);
#466=CONICAL_SURFACE('',#21605,16.625,0.785398163397451);
#467=CONICAL_SURFACE('',#21609,16.625,0.785398163397451);
#468=CONICAL_SURFACE('',#21611,16.625,0.785398163397451);
#469=CONICAL_SURFACE('',#21615,16.625,0.785398163397451);
#470=CONICAL_SURFACE('',#21617,16.625,0.785398163397451);
#471=CONICAL_SURFACE('',#21621,16.625,0.785398163397451);
#472=CONICAL_SURFACE('',#21623,16.625,0.785398163397451);
#473=CONICAL_SURFACE('',#21627,16.625,0.785398163397451);
#474=CONICAL_SURFACE('',#21629,16.625,0.785398163397451);
#475=CONICAL_SURFACE('',#21633,16.625,0.785398163397451);
#476=CONICAL_SURFACE('',#21635,16.625,0.785398163397451);
#477=CONICAL_SURFACE('',#21639,16.625,0.785398163397451);
#478=CONICAL_SURFACE('',#21641,16.625,0.785398163397451);
#479=CONICAL_SURFACE('',#21645,16.625,0.785398163397451);
#480=CONICAL_SURFACE('',#21647,16.625,0.785398163397451);
#481=CONICAL_SURFACE('',#21651,16.625,0.785398163397451);
#482=CONICAL_SURFACE('',#21653,16.625,0.785398163397451);
#483=CONICAL_SURFACE('',#21657,16.625,0.785398163397451);
#484=CONICAL_SURFACE('',#21659,16.625,0.785398163397451);
#485=CONICAL_SURFACE('',#21663,16.625,0.785398163397451);
#486=CONICAL_SURFACE('',#21665,16.625,0.785398163397451);
#487=CONICAL_SURFACE('',#21669,16.625,0.785398163397451);
#488=CONICAL_SURFACE('',#21672,9.75,0.785398163397451);
#489=CONICAL_SURFACE('',#21679,2.8,0.785398163397448);
#490=CONICAL_SURFACE('',#21694,2.8,0.785398163397436);
#491=CONICAL_SURFACE('',#21748,1.1,0.785398163397448);
#492=CONICAL_SURFACE('',#21763,1.1,0.785398163397448);
#493=CONICAL_SURFACE('',#21906,21.55,0.785398163397451);
#494=CONICAL_SURFACE('',#21955,22.7,0.785398163397452);
#495=CONICAL_SURFACE('',#22114,20.75,0.785398163397451);
#496=CONICAL_SURFACE('',#22152,20.75,0.785398163397451);
#497=CONICAL_SURFACE('',#22306,20.6,0.785398163397448);
#498=CONICAL_SURFACE('',#22380,20.75,0.785398163397451);
#499=CONICAL_SURFACE('',#22381,20.75,0.785398163397451);
#500=(
BOUNDED_SURFACE()
B_SPLINE_SURFACE(5,1,((#42423,#42424),(#42425,#42426),(#42427,#42428),(#42429,
#42430),(#42431,#42432),(#42433,#42434),(#42435,#42436),(#42437,#42438),
(#42439,#42440),(#42441,#42442),(#42443,#42444),(#42445,#42446),(#42447,
#42448),(#42449,#42450),(#42451,#42452),(#42453,#42454),(#42455,#42456),
(#42457,#42458),(#42459,#42460),(#42461,#42462),(#42463,#42464),(#42465,
#42466),(#42467,#42468),(#42469,#42470),(#42471,#42472),(#42473,#42474),
(#42475,#42476),(#42477,#42478),(#42479,#42480),(#42481,#42482),(#42483,
#42484),(#42485,#42486),(#42487,#42488),(#42489,#42490),(#42491,#42492),
(#42493,#42494),(#42495,#42496),(#42497,#42498),(#42499,#42500),(#42501,
#42502)),.UNSPECIFIED.,.F.,.F.,.F.)
B_SPLINE_SURFACE_WITH_KNOTS((6,1,1,1,1,1,1,1,1,1,1,1,1,1,1,1,1,1,1,1,1,
1,1,1,1,1,1,1,1,1,1,1,1,1,1,6),(2,2),(-1.,-0.971428571428572,-0.942857142857143,
-0.914285714285714,-0.885714285714286,-0.857142857142857,-0.828571428571429,
-0.8,-0.771428571428572,-0.742857142857143,-0.714285714285714,-0.685714285714286,
-0.657142857142857,-0.628571428571429,-0.6,-0.571428571428572,-0.542857142857143,
-0.514285714285714,-0.485714285714286,-0.457142857142857,-0.428571428571429,
-0.4,-0.371428571428571,-0.342857142857143,-0.314285714285714,-0.285714285714286,
-0.257142857142857,-0.228571428571429,-0.2,-0.171428571428571,-0.142857142857143,
-0.114285714285714,-0.0857142857142857,-0.0571428571428571,-0.0285714285714286,
0.),(0.,1.6),.UNSPECIFIED.)
GEOMETRIC_REPRESENTATION_ITEM()
RATIONAL_B_SPLINE_SURFACE(((1.,1.),(1.,1.),(1.,1.),(1.,1.),(1.,1.),(1.,
1.),(1.,1.),(1.,1.),(1.,1.),(1.,1.),(1.,1.),(1.,1.),(1.,1.),(1.,1.),(1.,
1.),(1.,1.),(1.,1.),(1.,1.),(1.,1.),(1.,1.),(1.,1.),(1.,1.),(1.,1.),(1.,
1.),(1.,1.),(1.,1.),(1.,1.),(1.,1.),(1.,1.),(1.,1.),(1.,1.),(1.,1.),(1.,
1.),(1.,1.),(1.,1.),(1.,1.),(1.,1.),(1.,1.),(1.,1.),(1.,1.)))
REPRESENTATION_ITEM('')
SURFACE()
);
#501=(
BOUNDED_SURFACE()
B_SPLINE_SURFACE(5,1,((#42551,#42552),(#42553,#42554),(#42555,#42556),(#42557,
#42558),(#42559,#42560),(#42561,#42562),(#42563,#42564),(#42565,#42566),
(#42567,#42568),(#42569,#42570),(#42571,#42572),(#42573,#42574),(#42575,
#42576),(#42577,#42578),(#42579,#42580),(#42581,#42582),(#42583,#42584),
(#42585,#42586),(#42587,#42588),(#42589,#42590),(#42591,#42592),(#42593,
#42594),(#42595,#42596),(#42597,#42598),(#42599,#42600),(#42601,#42602),
(#42603,#42604),(#42605,#42606),(#42607,#42608),(#42609,#42610),(#42611,
#42612),(#42613,#42614),(#42615,#42616),(#42617,#42618),(#42619,#42620),
(#42621,#42622),(#42623,#42624),(#42625,#42626),(#42627,#42628),(#42629,
#42630)),.UNSPECIFIED.,.F.,.F.,.F.)
B_SPLINE_SURFACE_WITH_KNOTS((6,1,1,1,1,1,1,1,1,1,1,1,1,1,1,1,1,1,1,1,1,
1,1,1,1,1,1,1,1,1,1,1,1,1,1,6),(2,2),(-1.,-0.971428571428572,-0.942857142857143,
-0.914285714285714,-0.885714285714286,-0.857142857142857,-0.828571428571429,
-0.8,-0.771428571428572,-0.742857142857143,-0.714285714285714,-0.685714285714286,
-0.657142857142857,-0.628571428571429,-0.6,-0.571428571428572,-0.542857142857143,
-0.514285714285714,-0.485714285714286,-0.457142857142857,-0.428571428571429,
-0.4,-0.371428571428571,-0.342857142857143,-0.314285714285714,-0.285714285714286,
-0.257142857142857,-0.228571428571429,-0.2,-0.171428571428571,-0.142857142857143,
-0.114285714285714,-0.0857142857142857,-0.0571428571428571,-0.0285714285714286,
0.),(0.,1.6),.UNSPECIFIED.)
GEOMETRIC_REPRESENTATION_ITEM()
RATIONAL_B_SPLINE_SURFACE(((1.,1.),(1.,1.),(1.,1.),(1.,1.),(1.,1.),(1.,
1.),(1.,1.),(1.,1.),(1.,1.),(1.,1.),(1.,1.),(1.,1.),(1.,1.),(1.,1.),(1.,
1.),(1.,1.),(1.,1.),(1.,1.),(1.,1.),(1.,1.),(1.,1.),(1.,1.),(1.,1.),(1.,
1.),(1.,1.),(1.,1.),(1.,1.),(1.,1.),(1.,1.),(1.,1.),(1.,1.),(1.,1.),(1.,
1.),(1.,1.),(1.,1.),(1.,1.),(1.,1.),(1.,1.),(1.,1.),(1.,1.)))
REPRESENTATION_ITEM('')
SURFACE()
);
#502=(
BOUNDED_SURFACE()
B_SPLINE_SURFACE(5,1,((#42775,#42776),(#42777,#42778),(#42779,#42780),(#42781,
#42782),(#42783,#42784),(#42785,#42786),(#42787,#42788),(#42789,#42790),
(#42791,#42792),(#42793,#42794),(#42795,#42796),(#42797,#42798),(#42799,
#42800),(#42801,#42802),(#42803,#42804),(#42805,#42806),(#42807,#42808),
(#42809,#42810),(#42811,#42812),(#42813,#42814),(#42815,#42816),(#42817,
#42818),(#42819,#42820),(#42821,#42822),(#42823,#42824),(#42825,#42826),
(#42827,#42828),(#42829,#42830),(#42831,#42832),(#42833,#42834),(#42835,
#42836),(#42837,#42838),(#42839,#42840),(#42841,#42842),(#42843,#42844),
(#42845,#42846),(#42847,#42848),(#42849,#42850),(#42851,#42852),(#42853,
#42854)),.UNSPECIFIED.,.F.,.F.,.F.)
B_SPLINE_SURFACE_WITH_KNOTS((6,1,1,1,1,1,1,1,1,1,1,1,1,1,1,1,1,1,1,1,1,
1,1,1,1,1,1,1,1,1,1,1,1,1,1,6),(2,2),(-1.,-0.971428571428572,-0.942857142857143,
-0.914285714285714,-0.885714285714286,-0.857142857142857,-0.828571428571429,
-0.8,-0.771428571428572,-0.742857142857143,-0.714285714285714,-0.685714285714286,
-0.657142857142857,-0.628571428571429,-0.6,-0.571428571428572,-0.542857142857143,
-0.514285714285714,-0.485714285714286,-0.457142857142857,-0.428571428571429,
-0.4,-0.371428571428571,-0.342857142857143,-0.314285714285714,-0.285714285714286,
-0.257142857142857,-0.228571428571429,-0.2,-0.171428571428571,-0.142857142857143,
-0.114285714285714,-0.0857142857142857,-0.0571428571428571,-0.0285714285714286,
0.),(0.,1.6),.UNSPECIFIED.)
GEOMETRIC_REPRESENTATION_ITEM()
RATIONAL_B_SPLINE_SURFACE(((1.,1.),(1.,1.),(1.,1.),(1.,1.),(1.,1.),(1.,
1.),(1.,1.),(1.,1.),(1.,1.),(1.,1.),(1.,1.),(1.,1.),(1.,1.),(1.,1.),(1.,
1.),(1.,1.),(1.,1.),(1.,1.),(1.,1.),(1.,1.),(1.,1.),(1.,1.),(1.,1.),(1.,
1.),(1.,1.),(1.,1.),(1.,1.),(1.,1.),(1.,1.),(1.,1.),(1.,1.),(1.,1.),(1.,
1.),(1.,1.),(1.,1.),(1.,1.),(1.,1.),(1.,1.),(1.,1.),(1.,1.)))
REPRESENTATION_ITEM('')
SURFACE()
);
#503=(
BOUNDED_SURFACE()
B_SPLINE_SURFACE(5,1,((#42903,#42904),(#42905,#42906),(#42907,#42908),(#42909,
#42910),(#42911,#42912),(#42913,#42914),(#42915,#42916),(#42917,#42918),
(#42919,#42920),(#42921,#42922),(#42923,#42924),(#42925,#42926),(#42927,
#42928),(#42929,#42930),(#42931,#42932),(#42933,#42934),(#42935,#42936),
(#42937,#42938),(#42939,#42940),(#42941,#42942),(#42943,#42944),(#42945,
#42946),(#42947,#42948),(#42949,#42950),(#42951,#42952),(#42953,#42954),
(#42955,#42956),(#42957,#42958),(#42959,#42960),(#42961,#42962),(#42963,
#42964),(#42965,#42966),(#42967,#42968),(#42969,#42970),(#42971,#42972),
(#42973,#42974),(#42975,#42976),(#42977,#42978),(#42979,#42980),(#42981,
#42982)),.UNSPECIFIED.,.F.,.F.,.F.)
B_SPLINE_SURFACE_WITH_KNOTS((6,1,1,1,1,1,1,1,1,1,1,1,1,1,1,1,1,1,1,1,1,
1,1,1,1,1,1,1,1,1,1,1,1,1,1,6),(2,2),(-1.,-0.971428571428572,-0.942857142857143,
-0.914285714285714,-0.885714285714286,-0.857142857142857,-0.828571428571429,
-0.8,-0.771428571428572,-0.742857142857143,-0.714285714285714,-0.685714285714286,
-0.657142857142857,-0.628571428571429,-0.6,-0.571428571428572,-0.542857142857143,
-0.514285714285714,-0.485714285714286,-0.457142857142857,-0.428571428571429,
-0.4,-0.371428571428571,-0.342857142857143,-0.314285714285714,-0.285714285714286,
-0.257142857142857,-0.228571428571429,-0.2,-0.171428571428571,-0.142857142857143,
-0.114285714285714,-0.0857142857142857,-0.0571428571428571,-0.0285714285714286,
0.),(0.,1.6),.UNSPECIFIED.)
GEOMETRIC_REPRESENTATION_ITEM()
RATIONAL_B_SPLINE_SURFACE(((1.,1.),(1.,1.),(1.,1.),(1.,1.),(1.,1.),(1.,
1.),(1.,1.),(1.,1.),(1.,1.),(1.,1.),(1.,1.),(1.,1.),(1.,1.),(1.,1.),(1.,
1.),(1.,1.),(1.,1.),(1.,1.),(1.,1.),(1.,1.),(1.,1.),(1.,1.),(1.,1.),(1.,
1.),(1.,1.),(1.,1.),(1.,1.),(1.,1.),(1.,1.),(1.,1.),(1.,1.),(1.,1.),(1.,
1.),(1.,1.),(1.,1.),(1.,1.),(1.,1.),(1.,1.),(1.,1.),(1.,1.)))
REPRESENTATION_ITEM('')
SURFACE()
);
#504=(
BOUNDED_SURFACE()
B_SPLINE_SURFACE(5,1,((#43097,#43098),(#43099,#43100),(#43101,#43102),(#43103,
#43104),(#43105,#43106),(#43107,#43108),(#43109,#43110),(#43111,#43112),
(#43113,#43114),(#43115,#43116),(#43117,#43118),(#43119,#43120),(#43121,
#43122),(#43123,#43124),(#43125,#43126),(#43127,#43128),(#43129,#43130),
(#43131,#43132),(#43133,#43134),(#43135,#43136),(#43137,#43138),(#43139,
#43140),(#43141,#43142),(#43143,#43144),(#43145,#43146),(#43147,#43148),
(#43149,#43150),(#43151,#43152),(#43153,#43154),(#43155,#43156),(#43157,
#43158),(#43159,#43160),(#43161,#43162),(#43163,#43164),(#43165,#43166),
(#43167,#43168),(#43169,#43170),(#43171,#43172),(#43173,#43174),(#43175,
#43176)),.UNSPECIFIED.,.F.,.F.,.F.)
B_SPLINE_SURFACE_WITH_KNOTS((6,1,1,1,1,1,1,1,1,1,1,1,1,1,1,1,1,1,1,1,1,
1,1,1,1,1,1,1,1,1,1,1,1,1,1,6),(2,2),(-1.,-0.971428571428572,-0.942857142857143,
-0.914285714285714,-0.885714285714286,-0.857142857142857,-0.828571428571429,
-0.8,-0.771428571428572,-0.742857142857143,-0.714285714285714,-0.685714285714286,
-0.657142857142857,-0.628571428571429,-0.6,-0.571428571428572,-0.542857142857143,
-0.514285714285714,-0.485714285714286,-0.457142857142857,-0.428571428571429,
-0.4,-0.371428571428571,-0.342857142857143,-0.314285714285714,-0.285714285714286,
-0.257142857142857,-0.228571428571429,-0.2,-0.171428571428571,-0.142857142857143,
-0.114285714285714,-0.0857142857142857,-0.0571428571428571,-0.0285714285714286,
0.),(0.,1.6),.UNSPECIFIED.)
GEOMETRIC_REPRESENTATION_ITEM()
RATIONAL_B_SPLINE_SURFACE(((1.,1.),(1.,1.),(1.,1.),(1.,1.),(1.,1.),(1.,
1.),(1.,1.),(1.,1.),(1.,1.),(1.,1.),(1.,1.),(1.,1.),(1.,1.),(1.,1.),(1.,
1.),(1.,1.),(1.,1.),(1.,1.),(1.,1.),(1.,1.),(1.,1.),(1.,1.),(1.,1.),(1.,
1.),(1.,1.),(1.,1.),(1.,1.),(1.,1.),(1.,1.),(1.,1.),(1.,1.),(1.,1.),(1.,
1.),(1.,1.),(1.,1.),(1.,1.),(1.,1.),(1.,1.),(1.,1.),(1.,1.)))
REPRESENTATION_ITEM('')
SURFACE()
);
#505=(
BOUNDED_SURFACE()
B_SPLINE_SURFACE(5,1,((#43225,#43226),(#43227,#43228),(#43229,#43230),(#43231,
#43232),(#43233,#43234),(#43235,#43236),(#43237,#43238),(#43239,#43240),
(#43241,#43242),(#43243,#43244),(#43245,#43246),(#43247,#43248),(#43249,
#43250),(#43251,#43252),(#43253,#43254),(#43255,#43256),(#43257,#43258),
(#43259,#43260),(#43261,#43262),(#43263,#43264),(#43265,#43266),(#43267,
#43268),(#43269,#43270),(#43271,#43272),(#43273,#43274),(#43275,#43276),
(#43277,#43278),(#43279,#43280),(#43281,#43282),(#43283,#43284),(#43285,
#43286),(#43287,#43288),(#43289,#43290),(#43291,#43292),(#43293,#43294),
(#43295,#43296),(#43297,#43298),(#43299,#43300),(#43301,#43302),(#43303,
#43304)),.UNSPECIFIED.,.F.,.F.,.F.)
B_SPLINE_SURFACE_WITH_KNOTS((6,1,1,1,1,1,1,1,1,1,1,1,1,1,1,1,1,1,1,1,1,
1,1,1,1,1,1,1,1,1,1,1,1,1,1,6),(2,2),(-1.,-0.971428571428572,-0.942857142857143,
-0.914285714285714,-0.885714285714286,-0.857142857142857,-0.828571428571429,
-0.8,-0.771428571428572,-0.742857142857143,-0.714285714285714,-0.685714285714286,
-0.657142857142857,-0.628571428571429,-0.6,-0.571428571428572,-0.542857142857143,
-0.514285714285714,-0.485714285714286,-0.457142857142857,-0.428571428571429,
-0.4,-0.371428571428571,-0.342857142857143,-0.314285714285714,-0.285714285714286,
-0.257142857142857,-0.228571428571429,-0.2,-0.171428571428571,-0.142857142857143,
-0.114285714285714,-0.0857142857142857,-0.0571428571428571,-0.0285714285714286,
0.),(0.,1.6),.UNSPECIFIED.)
GEOMETRIC_REPRESENTATION_ITEM()
RATIONAL_B_SPLINE_SURFACE(((1.,1.),(1.,1.),(1.,1.),(1.,1.),(1.,1.),(1.,
1.),(1.,1.),(1.,1.),(1.,1.),(1.,1.),(1.,1.),(1.,1.),(1.,1.),(1.,1.),(1.,
1.),(1.,1.),(1.,1.),(1.,1.),(1.,1.),(1.,1.),(1.,1.),(1.,1.),(1.,1.),(1.,
1.),(1.,1.),(1.,1.),(1.,1.),(1.,1.),(1.,1.),(1.,1.),(1.,1.),(1.,1.),(1.,
1.),(1.,1.),(1.,1.),(1.,1.),(1.,1.),(1.,1.),(1.,1.),(1.,1.)))
REPRESENTATION_ITEM('')
SURFACE()
);
#506=(
BOUNDED_SURFACE()
B_SPLINE_SURFACE(5,1,((#43419,#43420),(#43421,#43422),(#43423,#43424),(#43425,
#43426),(#43427,#43428),(#43429,#43430),(#43431,#43432),(#43433,#43434),
(#43435,#43436),(#43437,#43438),(#43439,#43440),(#43441,#43442),(#43443,
#43444),(#43445,#43446),(#43447,#43448),(#43449,#43450),(#43451,#43452),
(#43453,#43454),(#43455,#43456),(#43457,#43458),(#43459,#43460),(#43461,
#43462),(#43463,#43464),(#43465,#43466),(#43467,#43468),(#43469,#43470),
(#43471,#43472),(#43473,#43474),(#43475,#43476),(#43477,#43478),(#43479,
#43480),(#43481,#43482),(#43483,#43484),(#43485,#43486),(#43487,#43488),
(#43489,#43490),(#43491,#43492),(#43493,#43494),(#43495,#43496),(#43497,
#43498)),.UNSPECIFIED.,.F.,.F.,.F.)
B_SPLINE_SURFACE_WITH_KNOTS((6,1,1,1,1,1,1,1,1,1,1,1,1,1,1,1,1,1,1,1,1,
1,1,1,1,1,1,1,1,1,1,1,1,1,1,6),(2,2),(-1.,-0.971428571428572,-0.942857142857143,
-0.914285714285714,-0.885714285714286,-0.857142857142857,-0.828571428571429,
-0.8,-0.771428571428572,-0.742857142857143,-0.714285714285714,-0.685714285714286,
-0.657142857142857,-0.628571428571429,-0.6,-0.571428571428572,-0.542857142857143,
-0.514285714285714,-0.485714285714286,-0.457142857142857,-0.428571428571429,
-0.4,-0.371428571428571,-0.342857142857143,-0.314285714285714,-0.285714285714286,
-0.257142857142857,-0.228571428571429,-0.2,-0.171428571428571,-0.142857142857143,
-0.114285714285714,-0.0857142857142857,-0.0571428571428571,-0.0285714285714286,
0.),(0.,1.6),.UNSPECIFIED.)
GEOMETRIC_REPRESENTATION_ITEM()
RATIONAL_B_SPLINE_SURFACE(((1.,1.),(1.,1.),(1.,1.),(1.,1.),(1.,1.),(1.,
1.),(1.,1.),(1.,1.),(1.,1.),(1.,1.),(1.,1.),(1.,1.),(1.,1.),(1.,1.),(1.,
1.),(1.,1.),(1.,1.),(1.,1.),(1.,1.),(1.,1.),(1.,1.),(1.,1.),(1.,1.),(1.,
1.),(1.,1.),(1.,1.),(1.,1.),(1.,1.),(1.,1.),(1.,1.),(1.,1.),(1.,1.),(1.,
1.),(1.,1.),(1.,1.),(1.,1.),(1.,1.),(1.,1.),(1.,1.),(1.,1.)))
REPRESENTATION_ITEM('')
SURFACE()
);
#507=(
BOUNDED_SURFACE()
B_SPLINE_SURFACE(5,1,((#43547,#43548),(#43549,#43550),(#43551,#43552),(#43553,
#43554),(#43555,#43556),(#43557,#43558),(#43559,#43560),(#43561,#43562),
(#43563,#43564),(#43565,#43566),(#43567,#43568),(#43569,#43570),(#43571,
#43572),(#43573,#43574),(#43575,#43576),(#43577,#43578),(#43579,#43580),
(#43581,#43582),(#43583,#43584),(#43585,#43586),(#43587,#43588),(#43589,
#43590),(#43591,#43592),(#43593,#43594),(#43595,#43596),(#43597,#43598),
(#43599,#43600),(#43601,#43602),(#43603,#43604),(#43605,#43606),(#43607,
#43608),(#43609,#43610),(#43611,#43612),(#43613,#43614),(#43615,#43616),
(#43617,#43618),(#43619,#43620),(#43621,#43622),(#43623,#43624),(#43625,
#43626)),.UNSPECIFIED.,.F.,.F.,.F.)
B_SPLINE_SURFACE_WITH_KNOTS((6,1,1,1,1,1,1,1,1,1,1,1,1,1,1,1,1,1,1,1,1,
1,1,1,1,1,1,1,1,1,1,1,1,1,1,6),(2,2),(-1.,-0.971428571428572,-0.942857142857143,
-0.914285714285714,-0.885714285714286,-0.857142857142857,-0.828571428571429,
-0.8,-0.771428571428572,-0.742857142857143,-0.714285714285714,-0.685714285714286,
-0.657142857142857,-0.628571428571429,-0.6,-0.571428571428572,-0.542857142857143,
-0.514285714285714,-0.485714285714286,-0.457142857142857,-0.428571428571429,
-0.4,-0.371428571428571,-0.342857142857143,-0.314285714285714,-0.285714285714286,
-0.257142857142857,-0.228571428571429,-0.2,-0.171428571428571,-0.142857142857143,
-0.114285714285714,-0.0857142857142857,-0.0571428571428571,-0.0285714285714286,
0.),(0.,1.6),.UNSPECIFIED.)
GEOMETRIC_REPRESENTATION_ITEM()
RATIONAL_B_SPLINE_SURFACE(((1.,1.),(1.,1.),(1.,1.),(1.,1.),(1.,1.),(1.,
1.),(1.,1.),(1.,1.),(1.,1.),(1.,1.),(1.,1.),(1.,1.),(1.,1.),(1.,1.),(1.,
1.),(1.,1.),(1.,1.),(1.,1.),(1.,1.),(1.,1.),(1.,1.),(1.,1.),(1.,1.),(1.,
1.),(1.,1.),(1.,1.),(1.,1.),(1.,1.),(1.,1.),(1.,1.),(1.,1.),(1.,1.),(1.,
1.),(1.,1.),(1.,1.),(1.,1.),(1.,1.),(1.,1.),(1.,1.),(1.,1.)))
REPRESENTATION_ITEM('')
SURFACE()
);
#508=(
BOUNDED_SURFACE()
B_SPLINE_SURFACE(5,1,((#43741,#43742),(#43743,#43744),(#43745,#43746),(#43747,
#43748),(#43749,#43750),(#43751,#43752),(#43753,#43754),(#43755,#43756),
(#43757,#43758),(#43759,#43760),(#43761,#43762),(#43763,#43764),(#43765,
#43766),(#43767,#43768),(#43769,#43770),(#43771,#43772),(#43773,#43774),
(#43775,#43776),(#43777,#43778),(#43779,#43780),(#43781,#43782),(#43783,
#43784),(#43785,#43786),(#43787,#43788),(#43789,#43790),(#43791,#43792),
(#43793,#43794),(#43795,#43796),(#43797,#43798),(#43799,#43800),(#43801,
#43802),(#43803,#43804),(#43805,#43806),(#43807,#43808),(#43809,#43810),
(#43811,#43812),(#43813,#43814),(#43815,#43816),(#43817,#43818),(#43819,
#43820)),.UNSPECIFIED.,.F.,.F.,.F.)
B_SPLINE_SURFACE_WITH_KNOTS((6,1,1,1,1,1,1,1,1,1,1,1,1,1,1,1,1,1,1,1,1,
1,1,1,1,1,1,1,1,1,1,1,1,1,1,6),(2,2),(-1.,-0.971428571428572,-0.942857142857143,
-0.914285714285714,-0.885714285714286,-0.857142857142857,-0.828571428571429,
-0.8,-0.771428571428572,-0.742857142857143,-0.714285714285714,-0.685714285714286,
-0.657142857142857,-0.628571428571429,-0.6,-0.571428571428572,-0.542857142857143,
-0.514285714285714,-0.485714285714286,-0.457142857142857,-0.428571428571429,
-0.4,-0.371428571428571,-0.342857142857143,-0.314285714285714,-0.285714285714286,
-0.257142857142857,-0.228571428571429,-0.2,-0.171428571428571,-0.142857142857143,
-0.114285714285714,-0.0857142857142857,-0.0571428571428571,-0.0285714285714286,
0.),(0.,1.6),.UNSPECIFIED.)
GEOMETRIC_REPRESENTATION_ITEM()
RATIONAL_B_SPLINE_SURFACE(((1.,1.),(1.,1.),(1.,1.),(1.,1.),(1.,1.),(1.,
1.),(1.,1.),(1.,1.),(1.,1.),(1.,1.),(1.,1.),(1.,1.),(1.,1.),(1.,1.),(1.,
1.),(1.,1.),(1.,1.),(1.,1.),(1.,1.),(1.,1.),(1.,1.),(1.,1.),(1.,1.),(1.,
1.),(1.,1.),(1.,1.),(1.,1.),(1.,1.),(1.,1.),(1.,1.),(1.,1.),(1.,1.),(1.,
1.),(1.,1.),(1.,1.),(1.,1.),(1.,1.),(1.,1.),(1.,1.),(1.,1.)))
REPRESENTATION_ITEM('')
SURFACE()
);
#509=(
BOUNDED_SURFACE()
B_SPLINE_SURFACE(5,1,((#43882,#43883),(#43884,#43885),(#43886,#43887),(#43888,
#43889),(#43890,#43891),(#43892,#43893),(#43894,#43895),(#43896,#43897),
(#43898,#43899),(#43900,#43901),(#43902,#43903),(#43904,#43905),(#43906,
#43907),(#43908,#43909),(#43910,#43911),(#43912,#43913),(#43914,#43915),
(#43916,#43917),(#43918,#43919),(#43920,#43921),(#43922,#43923),(#43924,
#43925),(#43926,#43927),(#43928,#43929),(#43930,#43931),(#43932,#43933),
(#43934,#43935),(#43936,#43937),(#43938,#43939),(#43940,#43941),(#43942,
#43943),(#43944,#43945),(#43946,#43947),(#43948,#43949),(#43950,#43951),
(#43952,#43953),(#43954,#43955),(#43956,#43957),(#43958,#43959),(#43960,
#43961)),.UNSPECIFIED.,.F.,.F.,.F.)
B_SPLINE_SURFACE_WITH_KNOTS((6,1,1,1,1,1,1,1,1,1,1,1,1,1,1,1,1,1,1,1,1,
1,1,1,1,1,1,1,1,1,1,1,1,1,1,6),(2,2),(-1.,-0.971428571428572,-0.942857142857143,
-0.914285714285714,-0.885714285714286,-0.857142857142857,-0.828571428571429,
-0.8,-0.771428571428572,-0.742857142857143,-0.714285714285714,-0.685714285714286,
-0.657142857142857,-0.628571428571429,-0.6,-0.571428571428572,-0.542857142857143,
-0.514285714285714,-0.485714285714286,-0.457142857142857,-0.428571428571429,
-0.4,-0.371428571428571,-0.342857142857143,-0.314285714285714,-0.285714285714286,
-0.257142857142857,-0.228571428571429,-0.2,-0.171428571428571,-0.142857142857143,
-0.114285714285714,-0.0857142857142857,-0.0571428571428571,-0.0285714285714286,
0.),(0.,1.6),.UNSPECIFIED.)
GEOMETRIC_REPRESENTATION_ITEM()
RATIONAL_B_SPLINE_SURFACE(((1.,1.),(1.,1.),(1.,1.),(1.,1.),(1.,1.),(1.,
1.),(1.,1.),(1.,1.),(1.,1.),(1.,1.),(1.,1.),(1.,1.),(1.,1.),(1.,1.),(1.,
1.),(1.,1.),(1.,1.),(1.,1.),(1.,1.),(1.,1.),(1.,1.),(1.,1.),(1.,1.),(1.,
1.),(1.,1.),(1.,1.),(1.,1.),(1.,1.),(1.,1.),(1.,1.),(1.,1.),(1.,1.),(1.,
1.),(1.,1.),(1.,1.),(1.,1.),(1.,1.),(1.,1.),(1.,1.),(1.,1.)))
REPRESENTATION_ITEM('')
SURFACE()
);
#510=(
BOUNDED_SURFACE()
B_SPLINE_SURFACE(5,1,((#44076,#44077),(#44078,#44079),(#44080,#44081),(#44082,
#44083),(#44084,#44085),(#44086,#44087),(#44088,#44089),(#44090,#44091),
(#44092,#44093),(#44094,#44095),(#44096,#44097),(#44098,#44099),(#44100,
#44101),(#44102,#44103),(#44104,#44105),(#44106,#44107),(#44108,#44109),
(#44110,#44111),(#44112,#44113),(#44114,#44115),(#44116,#44117),(#44118,
#44119),(#44120,#44121),(#44122,#44123),(#44124,#44125),(#44126,#44127),
(#44128,#44129),(#44130,#44131),(#44132,#44133),(#44134,#44135),(#44136,
#44137),(#44138,#44139),(#44140,#44141),(#44142,#44143),(#44144,#44145),
(#44146,#44147),(#44148,#44149),(#44150,#44151),(#44152,#44153),(#44154,
#44155)),.UNSPECIFIED.,.F.,.F.,.F.)
B_SPLINE_SURFACE_WITH_KNOTS((6,1,1,1,1,1,1,1,1,1,1,1,1,1,1,1,1,1,1,1,1,
1,1,1,1,1,1,1,1,1,1,1,1,1,1,6),(2,2),(-1.,-0.971428571428572,-0.942857142857143,
-0.914285714285714,-0.885714285714286,-0.857142857142857,-0.828571428571429,
-0.8,-0.771428571428572,-0.742857142857143,-0.714285714285714,-0.685714285714286,
-0.657142857142857,-0.628571428571429,-0.6,-0.571428571428572,-0.542857142857143,
-0.514285714285714,-0.485714285714286,-0.457142857142857,-0.428571428571429,
-0.4,-0.371428571428571,-0.342857142857143,-0.314285714285714,-0.285714285714286,
-0.257142857142857,-0.228571428571429,-0.2,-0.171428571428571,-0.142857142857143,
-0.114285714285714,-0.0857142857142857,-0.0571428571428571,-0.0285714285714286,
0.),(0.,1.6),.UNSPECIFIED.)
GEOMETRIC_REPRESENTATION_ITEM()
RATIONAL_B_SPLINE_SURFACE(((1.,1.),(1.,1.),(1.,1.),(1.,1.),(1.,1.),(1.,
1.),(1.,1.),(1.,1.),(1.,1.),(1.,1.),(1.,1.),(1.,1.),(1.,1.),(1.,1.),(1.,
1.),(1.,1.),(1.,1.),(1.,1.),(1.,1.),(1.,1.),(1.,1.),(1.,1.),(1.,1.),(1.,
1.),(1.,1.),(1.,1.),(1.,1.),(1.,1.),(1.,1.),(1.,1.),(1.,1.),(1.,1.),(1.,
1.),(1.,1.),(1.,1.),(1.,1.),(1.,1.),(1.,1.),(1.,1.),(1.,1.)))
REPRESENTATION_ITEM('')
SURFACE()
);
#511=(
BOUNDED_SURFACE()
B_SPLINE_SURFACE(5,1,((#44204,#44205),(#44206,#44207),(#44208,#44209),(#44210,
#44211),(#44212,#44213),(#44214,#44215),(#44216,#44217),(#44218,#44219),
(#44220,#44221),(#44222,#44223),(#44224,#44225),(#44226,#44227),(#44228,
#44229),(#44230,#44231),(#44232,#44233),(#44234,#44235),(#44236,#44237),
(#44238,#44239),(#44240,#44241),(#44242,#44243),(#44244,#44245),(#44246,
#44247),(#44248,#44249),(#44250,#44251),(#44252,#44253),(#44254,#44255),
(#44256,#44257),(#44258,#44259),(#44260,#44261),(#44262,#44263),(#44264,
#44265),(#44266,#44267),(#44268,#44269),(#44270,#44271),(#44272,#44273),
(#44274,#44275),(#44276,#44277),(#44278,#44279),(#44280,#44281),(#44282,
#44283)),.UNSPECIFIED.,.F.,.F.,.F.)
B_SPLINE_SURFACE_WITH_KNOTS((6,1,1,1,1,1,1,1,1,1,1,1,1,1,1,1,1,1,1,1,1,
1,1,1,1,1,1,1,1,1,1,1,1,1,1,6),(2,2),(-1.,-0.971428571428572,-0.942857142857143,
-0.914285714285714,-0.885714285714286,-0.857142857142857,-0.828571428571429,
-0.8,-0.771428571428572,-0.742857142857143,-0.714285714285714,-0.685714285714286,
-0.657142857142857,-0.628571428571429,-0.6,-0.571428571428572,-0.542857142857143,
-0.514285714285714,-0.485714285714286,-0.457142857142857,-0.428571428571429,
-0.4,-0.371428571428571,-0.342857142857143,-0.314285714285714,-0.285714285714286,
-0.257142857142857,-0.228571428571429,-0.2,-0.171428571428571,-0.142857142857143,
-0.114285714285714,-0.0857142857142857,-0.0571428571428571,-0.0285714285714286,
0.),(0.,1.6),.UNSPECIFIED.)
GEOMETRIC_REPRESENTATION_ITEM()
RATIONAL_B_SPLINE_SURFACE(((1.,1.),(1.,1.),(1.,1.),(1.,1.),(1.,1.),(1.,
1.),(1.,1.),(1.,1.),(1.,1.),(1.,1.),(1.,1.),(1.,1.),(1.,1.),(1.,1.),(1.,
1.),(1.,1.),(1.,1.),(1.,1.),(1.,1.),(1.,1.),(1.,1.),(1.,1.),(1.,1.),(1.,
1.),(1.,1.),(1.,1.),(1.,1.),(1.,1.),(1.,1.),(1.,1.),(1.,1.),(1.,1.),(1.,
1.),(1.,1.),(1.,1.),(1.,1.),(1.,1.),(1.,1.),(1.,1.),(1.,1.)))
REPRESENTATION_ITEM('')
SURFACE()
);
#512=(
BOUNDED_SURFACE()
B_SPLINE_SURFACE(5,1,((#44398,#44399),(#44400,#44401),(#44402,#44403),(#44404,
#44405),(#44406,#44407),(#44408,#44409),(#44410,#44411),(#44412,#44413),
(#44414,#44415),(#44416,#44417),(#44418,#44419),(#44420,#44421),(#44422,
#44423),(#44424,#44425),(#44426,#44427),(#44428,#44429),(#44430,#44431),
(#44432,#44433),(#44434,#44435),(#44436,#44437),(#44438,#44439),(#44440,
#44441),(#44442,#44443),(#44444,#44445),(#44446,#44447),(#44448,#44449),
(#44450,#44451),(#44452,#44453),(#44454,#44455),(#44456,#44457),(#44458,
#44459),(#44460,#44461),(#44462,#44463),(#44464,#44465),(#44466,#44467),
(#44468,#44469),(#44470,#44471),(#44472,#44473),(#44474,#44475),(#44476,
#44477)),.UNSPECIFIED.,.F.,.F.,.F.)
B_SPLINE_SURFACE_WITH_KNOTS((6,1,1,1,1,1,1,1,1,1,1,1,1,1,1,1,1,1,1,1,1,
1,1,1,1,1,1,1,1,1,1,1,1,1,1,6),(2,2),(-1.,-0.971428571428572,-0.942857142857143,
-0.914285714285714,-0.885714285714286,-0.857142857142857,-0.828571428571429,
-0.8,-0.771428571428572,-0.742857142857143,-0.714285714285714,-0.685714285714286,
-0.657142857142857,-0.628571428571429,-0.6,-0.571428571428572,-0.542857142857143,
-0.514285714285714,-0.485714285714286,-0.457142857142857,-0.428571428571429,
-0.4,-0.371428571428571,-0.342857142857143,-0.314285714285714,-0.285714285714286,
-0.257142857142857,-0.228571428571429,-0.2,-0.171428571428571,-0.142857142857143,
-0.114285714285714,-0.0857142857142857,-0.0571428571428571,-0.0285714285714286,
0.),(0.,1.6),.UNSPECIFIED.)
GEOMETRIC_REPRESENTATION_ITEM()
RATIONAL_B_SPLINE_SURFACE(((1.,1.),(1.,1.),(1.,1.),(1.,1.),(1.,1.),(1.,
1.),(1.,1.),(1.,1.),(1.,1.),(1.,1.),(1.,1.),(1.,1.),(1.,1.),(1.,1.),(1.,
1.),(1.,1.),(1.,1.),(1.,1.),(1.,1.),(1.,1.),(1.,1.),(1.,1.),(1.,1.),(1.,
1.),(1.,1.),(1.,1.),(1.,1.),(1.,1.),(1.,1.),(1.,1.),(1.,1.),(1.,1.),(1.,
1.),(1.,1.),(1.,1.),(1.,1.),(1.,1.),(1.,1.),(1.,1.),(1.,1.)))
REPRESENTATION_ITEM('')
SURFACE()
);
#513=(
BOUNDED_SURFACE()
B_SPLINE_SURFACE(5,1,((#44526,#44527),(#44528,#44529),(#44530,#44531),(#44532,
#44533),(#44534,#44535),(#44536,#44537),(#44538,#44539),(#44540,#44541),
(#44542,#44543),(#44544,#44545),(#44546,#44547),(#44548,#44549),(#44550,
#44551),(#44552,#44553),(#44554,#44555),(#44556,#44557),(#44558,#44559),
(#44560,#44561),(#44562,#44563),(#44564,#44565),(#44566,#44567),(#44568,
#44569),(#44570,#44571),(#44572,#44573),(#44574,#44575),(#44576,#44577),
(#44578,#44579),(#44580,#44581),(#44582,#44583),(#44584,#44585),(#44586,
#44587),(#44588,#44589),(#44590,#44591),(#44592,#44593),(#44594,#44595),
(#44596,#44597),(#44598,#44599),(#44600,#44601),(#44602,#44603),(#44604,
#44605)),.UNSPECIFIED.,.F.,.F.,.F.)
B_SPLINE_SURFACE_WITH_KNOTS((6,1,1,1,1,1,1,1,1,1,1,1,1,1,1,1,1,1,1,1,1,
1,1,1,1,1,1,1,1,1,1,1,1,1,1,6),(2,2),(-1.,-0.971428571428572,-0.942857142857143,
-0.914285714285714,-0.885714285714286,-0.857142857142857,-0.828571428571429,
-0.8,-0.771428571428572,-0.742857142857143,-0.714285714285714,-0.685714285714286,
-0.657142857142857,-0.628571428571429,-0.6,-0.571428571428572,-0.542857142857143,
-0.514285714285714,-0.485714285714286,-0.457142857142857,-0.428571428571429,
-0.4,-0.371428571428571,-0.342857142857143,-0.314285714285714,-0.285714285714286,
-0.257142857142857,-0.228571428571429,-0.2,-0.171428571428571,-0.142857142857143,
-0.114285714285714,-0.0857142857142857,-0.0571428571428571,-0.0285714285714286,
0.),(0.,1.6),.UNSPECIFIED.)
GEOMETRIC_REPRESENTATION_ITEM()
RATIONAL_B_SPLINE_SURFACE(((1.,1.),(1.,1.),(1.,1.),(1.,1.),(1.,1.),(1.,
1.),(1.,1.),(1.,1.),(1.,1.),(1.,1.),(1.,1.),(1.,1.),(1.,1.),(1.,1.),(1.,
1.),(1.,1.),(1.,1.),(1.,1.),(1.,1.),(1.,1.),(1.,1.),(1.,1.),(1.,1.),(1.,
1.),(1.,1.),(1.,1.),(1.,1.),(1.,1.),(1.,1.),(1.,1.),(1.,1.),(1.,1.),(1.,
1.),(1.,1.),(1.,1.),(1.,1.),(1.,1.),(1.,1.),(1.,1.),(1.,1.)))
REPRESENTATION_ITEM('')
SURFACE()
);
#514=(
BOUNDED_SURFACE()
B_SPLINE_SURFACE(5,1,((#44722,#44723),(#44724,#44725),(#44726,#44727),(#44728,
#44729),(#44730,#44731),(#44732,#44733),(#44734,#44735),(#44736,#44737),
(#44738,#44739),(#44740,#44741),(#44742,#44743),(#44744,#44745),(#44746,
#44747),(#44748,#44749),(#44750,#44751),(#44752,#44753),(#44754,#44755),
(#44756,#44757),(#44758,#44759),(#44760,#44761),(#44762,#44763),(#44764,
#44765),(#44766,#44767),(#44768,#44769),(#44770,#44771),(#44772,#44773),
(#44774,#44775),(#44776,#44777),(#44778,#44779),(#44780,#44781),(#44782,
#44783),(#44784,#44785),(#44786,#44787),(#44788,#44789),(#44790,#44791),
(#44792,#44793),(#44794,#44795),(#44796,#44797),(#44798,#44799),(#44800,
#44801)),.UNSPECIFIED.,.F.,.F.,.F.)
B_SPLINE_SURFACE_WITH_KNOTS((6,1,1,1,1,1,1,1,1,1,1,1,1,1,1,1,1,1,1,1,1,
1,1,1,1,1,1,1,1,1,1,1,1,1,1,6),(2,2),(-1.,-0.971428571428572,-0.942857142857143,
-0.914285714285714,-0.885714285714286,-0.857142857142857,-0.828571428571429,
-0.8,-0.771428571428572,-0.742857142857143,-0.714285714285714,-0.685714285714286,
-0.657142857142857,-0.628571428571429,-0.6,-0.571428571428572,-0.542857142857143,
-0.514285714285714,-0.485714285714286,-0.457142857142857,-0.428571428571429,
-0.4,-0.371428571428571,-0.342857142857143,-0.314285714285714,-0.285714285714286,
-0.257142857142857,-0.228571428571429,-0.2,-0.171428571428571,-0.142857142857143,
-0.114285714285714,-0.0857142857142857,-0.0571428571428571,-0.0285714285714286,
0.),(0.,1.6),.UNSPECIFIED.)
GEOMETRIC_REPRESENTATION_ITEM()
RATIONAL_B_SPLINE_SURFACE(((1.,1.),(1.,1.),(1.,1.),(1.,1.),(1.,1.),(1.,
1.),(1.,1.),(1.,1.),(1.,1.),(1.,1.),(1.,1.),(1.,1.),(1.,1.),(1.,1.),(1.,
1.),(1.,1.),(1.,1.),(1.,1.),(1.,1.),(1.,1.),(1.,1.),(1.,1.),(1.,1.),(1.,
1.),(1.,1.),(1.,1.),(1.,1.),(1.,1.),(1.,1.),(1.,1.),(1.,1.),(1.,1.),(1.,
1.),(1.,1.),(1.,1.),(1.,1.),(1.,1.),(1.,1.),(1.,1.),(1.,1.)))
REPRESENTATION_ITEM('')
SURFACE()
);
#515=(
BOUNDED_SURFACE()
B_SPLINE_SURFACE(5,1,((#44852,#44853),(#44854,#44855),(#44856,#44857),(#44858,
#44859),(#44860,#44861),(#44862,#44863),(#44864,#44865),(#44866,#44867),
(#44868,#44869),(#44870,#44871),(#44872,#44873),(#44874,#44875),(#44876,
#44877),(#44878,#44879),(#44880,#44881),(#44882,#44883),(#44884,#44885),
(#44886,#44887),(#44888,#44889),(#44890,#44891),(#44892,#44893),(#44894,
#44895),(#44896,#44897),(#44898,#44899),(#44900,#44901),(#44902,#44903),
(#44904,#44905),(#44906,#44907),(#44908,#44909),(#44910,#44911),(#44912,
#44913),(#44914,#44915),(#44916,#44917),(#44918,#44919),(#44920,#44921),
(#44922,#44923),(#44924,#44925),(#44926,#44927),(#44928,#44929),(#44930,
#44931)),.UNSPECIFIED.,.F.,.F.,.F.)
B_SPLINE_SURFACE_WITH_KNOTS((6,1,1,1,1,1,1,1,1,1,1,1,1,1,1,1,1,1,1,1,1,
1,1,1,1,1,1,1,1,1,1,1,1,1,1,6),(2,2),(-1.,-0.971428571428572,-0.942857142857143,
-0.914285714285714,-0.885714285714286,-0.857142857142857,-0.828571428571429,
-0.8,-0.771428571428572,-0.742857142857143,-0.714285714285714,-0.685714285714286,
-0.657142857142857,-0.628571428571429,-0.6,-0.571428571428572,-0.542857142857143,
-0.514285714285714,-0.485714285714286,-0.457142857142857,-0.428571428571429,
-0.4,-0.371428571428571,-0.342857142857143,-0.314285714285714,-0.285714285714286,
-0.257142857142857,-0.228571428571429,-0.2,-0.171428571428571,-0.142857142857143,
-0.114285714285714,-0.0857142857142857,-0.0571428571428571,-0.0285714285714286,
0.),(0.,1.6),.UNSPECIFIED.)
GEOMETRIC_REPRESENTATION_ITEM()
RATIONAL_B_SPLINE_SURFACE(((1.,1.),(1.,1.),(1.,1.),(1.,1.),(1.,1.),(1.,
1.),(1.,1.),(1.,1.),(1.,1.),(1.,1.),(1.,1.),(1.,1.),(1.,1.),(1.,1.),(1.,
1.),(1.,1.),(1.,1.),(1.,1.),(1.,1.),(1.,1.),(1.,1.),(1.,1.),(1.,1.),(1.,
1.),(1.,1.),(1.,1.),(1.,1.),(1.,1.),(1.,1.),(1.,1.),(1.,1.),(1.,1.),(1.,
1.),(1.,1.),(1.,1.),(1.,1.),(1.,1.),(1.,1.),(1.,1.),(1.,1.)))
REPRESENTATION_ITEM('')
SURFACE()
);
#516=(
BOUNDED_SURFACE()
B_SPLINE_SURFACE(5,1,((#45048,#45049),(#45050,#45051),(#45052,#45053),(#45054,
#45055),(#45056,#45057),(#45058,#45059),(#45060,#45061),(#45062,#45063),
(#45064,#45065),(#45066,#45067),(#45068,#45069),(#45070,#45071),(#45072,
#45073),(#45074,#45075),(#45076,#45077),(#45078,#45079),(#45080,#45081),
(#45082,#45083),(#45084,#45085),(#45086,#45087),(#45088,#45089),(#45090,
#45091),(#45092,#45093),(#45094,#45095),(#45096,#45097),(#45098,#45099),
(#45100,#45101),(#45102,#45103),(#45104,#45105),(#45106,#45107),(#45108,
#45109),(#45110,#45111),(#45112,#45113),(#45114,#45115),(#45116,#45117),
(#45118,#45119),(#45120,#45121),(#45122,#45123),(#45124,#45125),(#45126,
#45127)),.UNSPECIFIED.,.F.,.F.,.F.)
B_SPLINE_SURFACE_WITH_KNOTS((6,1,1,1,1,1,1,1,1,1,1,1,1,1,1,1,1,1,1,1,1,
1,1,1,1,1,1,1,1,1,1,1,1,1,1,6),(2,2),(-1.,-0.971428571428572,-0.942857142857143,
-0.914285714285714,-0.885714285714286,-0.857142857142857,-0.828571428571429,
-0.8,-0.771428571428572,-0.742857142857143,-0.714285714285714,-0.685714285714286,
-0.657142857142857,-0.628571428571429,-0.6,-0.571428571428572,-0.542857142857143,
-0.514285714285714,-0.485714285714286,-0.457142857142857,-0.428571428571429,
-0.4,-0.371428571428571,-0.342857142857143,-0.314285714285714,-0.285714285714286,
-0.257142857142857,-0.228571428571429,-0.2,-0.171428571428571,-0.142857142857143,
-0.114285714285714,-0.0857142857142857,-0.0571428571428571,-0.0285714285714286,
0.),(0.,1.6),.UNSPECIFIED.)
GEOMETRIC_REPRESENTATION_ITEM()
RATIONAL_B_SPLINE_SURFACE(((1.,1.),(1.,1.),(1.,1.),(1.,1.),(1.,1.),(1.,
1.),(1.,1.),(1.,1.),(1.,1.),(1.,1.),(1.,1.),(1.,1.),(1.,1.),(1.,1.),(1.,
1.),(1.,1.),(1.,1.),(1.,1.),(1.,1.),(1.,1.),(1.,1.),(1.,1.),(1.,1.),(1.,
1.),(1.,1.),(1.,1.),(1.,1.),(1.,1.),(1.,1.),(1.,1.),(1.,1.),(1.,1.),(1.,
1.),(1.,1.),(1.,1.),(1.,1.),(1.,1.),(1.,1.),(1.,1.),(1.,1.)))
REPRESENTATION_ITEM('')
SURFACE()
);
#517=(
BOUNDED_SURFACE()
B_SPLINE_SURFACE(5,1,((#45176,#45177),(#45178,#45179),(#45180,#45181),(#45182,
#45183),(#45184,#45185),(#45186,#45187),(#45188,#45189),(#45190,#45191),
(#45192,#45193),(#45194,#45195),(#45196,#45197),(#45198,#45199),(#45200,
#45201),(#45202,#45203),(#45204,#45205),(#45206,#45207),(#45208,#45209),
(#45210,#45211),(#45212,#45213),(#45214,#45215),(#45216,#45217),(#45218,
#45219),(#45220,#45221),(#45222,#45223),(#45224,#45225),(#45226,#45227),
(#45228,#45229),(#45230,#45231),(#45232,#45233),(#45234,#45235),(#45236,
#45237),(#45238,#45239),(#45240,#45241),(#45242,#45243),(#45244,#45245),
(#45246,#45247),(#45248,#45249),(#45250,#45251),(#45252,#45253),(#45254,
#45255)),.UNSPECIFIED.,.F.,.F.,.F.)
B_SPLINE_SURFACE_WITH_KNOTS((6,1,1,1,1,1,1,1,1,1,1,1,1,1,1,1,1,1,1,1,1,
1,1,1,1,1,1,1,1,1,1,1,1,1,1,6),(2,2),(-1.,-0.971428571428572,-0.942857142857143,
-0.914285714285714,-0.885714285714286,-0.857142857142857,-0.828571428571429,
-0.8,-0.771428571428572,-0.742857142857143,-0.714285714285714,-0.685714285714286,
-0.657142857142857,-0.628571428571429,-0.6,-0.571428571428572,-0.542857142857143,
-0.514285714285714,-0.485714285714286,-0.457142857142857,-0.428571428571429,
-0.4,-0.371428571428571,-0.342857142857143,-0.314285714285714,-0.285714285714286,
-0.257142857142857,-0.228571428571429,-0.2,-0.171428571428571,-0.142857142857143,
-0.114285714285714,-0.0857142857142857,-0.0571428571428571,-0.0285714285714286,
0.),(0.,1.6),.UNSPECIFIED.)
GEOMETRIC_REPRESENTATION_ITEM()
RATIONAL_B_SPLINE_SURFACE(((1.,1.),(1.,1.),(1.,1.),(1.,1.),(1.,1.),(1.,
1.),(1.,1.),(1.,1.),(1.,1.),(1.,1.),(1.,1.),(1.,1.),(1.,1.),(1.,1.),(1.,
1.),(1.,1.),(1.,1.),(1.,1.),(1.,1.),(1.,1.),(1.,1.),(1.,1.),(1.,1.),(1.,
1.),(1.,1.),(1.,1.),(1.,1.),(1.,1.),(1.,1.),(1.,1.),(1.,1.),(1.,1.),(1.,
1.),(1.,1.),(1.,1.),(1.,1.),(1.,1.),(1.,1.),(1.,1.),(1.,1.)))
REPRESENTATION_ITEM('')
SURFACE()
);
#518=(
BOUNDED_SURFACE()
B_SPLINE_SURFACE(5,1,((#45370,#45371),(#45372,#45373),(#45374,#45375),(#45376,
#45377),(#45378,#45379),(#45380,#45381),(#45382,#45383),(#45384,#45385),
(#45386,#45387),(#45388,#45389),(#45390,#45391),(#45392,#45393),(#45394,
#45395),(#45396,#45397),(#45398,#45399),(#45400,#45401),(#45402,#45403),
(#45404,#45405),(#45406,#45407),(#45408,#45409),(#45410,#45411),(#45412,
#45413),(#45414,#45415),(#45416,#45417),(#45418,#45419),(#45420,#45421),
(#45422,#45423),(#45424,#45425),(#45426,#45427),(#45428,#45429),(#45430,
#45431),(#45432,#45433),(#45434,#45435),(#45436,#45437),(#45438,#45439),
(#45440,#45441),(#45442,#45443),(#45444,#45445),(#45446,#45447),(#45448,
#45449)),.UNSPECIFIED.,.F.,.F.,.F.)
B_SPLINE_SURFACE_WITH_KNOTS((6,1,1,1,1,1,1,1,1,1,1,1,1,1,1,1,1,1,1,1,1,
1,1,1,1,1,1,1,1,1,1,1,1,1,1,6),(2,2),(-1.,-0.971428571428572,-0.942857142857143,
-0.914285714285714,-0.885714285714286,-0.857142857142857,-0.828571428571429,
-0.8,-0.771428571428572,-0.742857142857143,-0.714285714285714,-0.685714285714286,
-0.657142857142857,-0.628571428571429,-0.6,-0.571428571428572,-0.542857142857143,
-0.514285714285714,-0.485714285714286,-0.457142857142857,-0.428571428571429,
-0.4,-0.371428571428571,-0.342857142857143,-0.314285714285714,-0.285714285714286,
-0.257142857142857,-0.228571428571429,-0.2,-0.171428571428571,-0.142857142857143,
-0.114285714285714,-0.0857142857142857,-0.0571428571428571,-0.0285714285714286,
0.),(0.,1.6),.UNSPECIFIED.)
GEOMETRIC_REPRESENTATION_ITEM()
RATIONAL_B_SPLINE_SURFACE(((1.,1.),(1.,1.),(1.,1.),(1.,1.),(1.,1.),(1.,
1.),(1.,1.),(1.,1.),(1.,1.),(1.,1.),(1.,1.),(1.,1.),(1.,1.),(1.,1.),(1.,
1.),(1.,1.),(1.,1.),(1.,1.),(1.,1.),(1.,1.),(1.,1.),(1.,1.),(1.,1.),(1.,
1.),(1.,1.),(1.,1.),(1.,1.),(1.,1.),(1.,1.),(1.,1.),(1.,1.),(1.,1.),(1.,
1.),(1.,1.),(1.,1.),(1.,1.),(1.,1.),(1.,1.),(1.,1.),(1.,1.)))
REPRESENTATION_ITEM('')
SURFACE()
);
#519=(
BOUNDED_SURFACE()
B_SPLINE_SURFACE(5,1,((#45498,#45499),(#45500,#45501),(#45502,#45503),(#45504,
#45505),(#45506,#45507),(#45508,#45509),(#45510,#45511),(#45512,#45513),
(#45514,#45515),(#45516,#45517),(#45518,#45519),(#45520,#45521),(#45522,
#45523),(#45524,#45525),(#45526,#45527),(#45528,#45529),(#45530,#45531),
(#45532,#45533),(#45534,#45535),(#45536,#45537),(#45538,#45539),(#45540,
#45541),(#45542,#45543),(#45544,#45545),(#45546,#45547),(#45548,#45549),
(#45550,#45551),(#45552,#45553),(#45554,#45555),(#45556,#45557),(#45558,
#45559),(#45560,#45561),(#45562,#45563),(#45564,#45565),(#45566,#45567),
(#45568,#45569),(#45570,#45571),(#45572,#45573),(#45574,#45575),(#45576,
#45577)),.UNSPECIFIED.,.F.,.F.,.F.)
B_SPLINE_SURFACE_WITH_KNOTS((6,1,1,1,1,1,1,1,1,1,1,1,1,1,1,1,1,1,1,1,1,
1,1,1,1,1,1,1,1,1,1,1,1,1,1,6),(2,2),(-1.,-0.971428571428572,-0.942857142857143,
-0.914285714285714,-0.885714285714286,-0.857142857142857,-0.828571428571429,
-0.8,-0.771428571428572,-0.742857142857143,-0.714285714285714,-0.685714285714286,
-0.657142857142857,-0.628571428571429,-0.6,-0.571428571428572,-0.542857142857143,
-0.514285714285714,-0.485714285714286,-0.457142857142857,-0.428571428571429,
-0.4,-0.371428571428571,-0.342857142857143,-0.314285714285714,-0.285714285714286,
-0.257142857142857,-0.228571428571429,-0.2,-0.171428571428571,-0.142857142857143,
-0.114285714285714,-0.0857142857142857,-0.0571428571428571,-0.0285714285714286,
0.),(0.,1.6),.UNSPECIFIED.)
GEOMETRIC_REPRESENTATION_ITEM()
RATIONAL_B_SPLINE_SURFACE(((1.,1.),(1.,1.),(1.,1.),(1.,1.),(1.,1.),(1.,
1.),(1.,1.),(1.,1.),(1.,1.),(1.,1.),(1.,1.),(1.,1.),(1.,1.),(1.,1.),(1.,
1.),(1.,1.),(1.,1.),(1.,1.),(1.,1.),(1.,1.),(1.,1.),(1.,1.),(1.,1.),(1.,
1.),(1.,1.),(1.,1.),(1.,1.),(1.,1.),(1.,1.),(1.,1.),(1.,1.),(1.,1.),(1.,
1.),(1.,1.),(1.,1.),(1.,1.),(1.,1.),(1.,1.),(1.,1.),(1.,1.)))
REPRESENTATION_ITEM('')
SURFACE()
);
#520=(
BOUNDED_SURFACE()
B_SPLINE_SURFACE(5,1,((#45692,#45693),(#45694,#45695),(#45696,#45697),(#45698,
#45699),(#45700,#45701),(#45702,#45703),(#45704,#45705),(#45706,#45707),
(#45708,#45709),(#45710,#45711),(#45712,#45713),(#45714,#45715),(#45716,
#45717),(#45718,#45719),(#45720,#45721),(#45722,#45723),(#45724,#45725),
(#45726,#45727),(#45728,#45729),(#45730,#45731),(#45732,#45733),(#45734,
#45735),(#45736,#45737),(#45738,#45739),(#45740,#45741),(#45742,#45743),
(#45744,#45745),(#45746,#45747),(#45748,#45749),(#45750,#45751),(#45752,
#45753),(#45754,#45755),(#45756,#45757),(#45758,#45759),(#45760,#45761),
(#45762,#45763),(#45764,#45765),(#45766,#45767),(#45768,#45769),(#45770,
#45771)),.UNSPECIFIED.,.F.,.F.,.F.)
B_SPLINE_SURFACE_WITH_KNOTS((6,1,1,1,1,1,1,1,1,1,1,1,1,1,1,1,1,1,1,1,1,
1,1,1,1,1,1,1,1,1,1,1,1,1,1,6),(2,2),(-1.,-0.971428571428572,-0.942857142857143,
-0.914285714285714,-0.885714285714286,-0.857142857142857,-0.828571428571429,
-0.8,-0.771428571428572,-0.742857142857143,-0.714285714285714,-0.685714285714286,
-0.657142857142857,-0.628571428571429,-0.6,-0.571428571428572,-0.542857142857143,
-0.514285714285714,-0.485714285714286,-0.457142857142857,-0.428571428571429,
-0.4,-0.371428571428571,-0.342857142857143,-0.314285714285714,-0.285714285714286,
-0.257142857142857,-0.228571428571429,-0.2,-0.171428571428571,-0.142857142857143,
-0.114285714285714,-0.0857142857142857,-0.0571428571428571,-0.0285714285714286,
0.),(0.,1.6),.UNSPECIFIED.)
GEOMETRIC_REPRESENTATION_ITEM()
RATIONAL_B_SPLINE_SURFACE(((1.,1.),(1.,1.),(1.,1.),(1.,1.),(1.,1.),(1.,
1.),(1.,1.),(1.,1.),(1.,1.),(1.,1.),(1.,1.),(1.,1.),(1.,1.),(1.,1.),(1.,
1.),(1.,1.),(1.,1.),(1.,1.),(1.,1.),(1.,1.),(1.,1.),(1.,1.),(1.,1.),(1.,
1.),(1.,1.),(1.,1.),(1.,1.),(1.,1.),(1.,1.),(1.,1.),(1.,1.),(1.,1.),(1.,
1.),(1.,1.),(1.,1.),(1.,1.),(1.,1.),(1.,1.),(1.,1.),(1.,1.)))
REPRESENTATION_ITEM('')
SURFACE()
);
#521=(
BOUNDED_SURFACE()
B_SPLINE_SURFACE(5,1,((#45820,#45821),(#45822,#45823),(#45824,#45825),(#45826,
#45827),(#45828,#45829),(#45830,#45831),(#45832,#45833),(#45834,#45835),
(#45836,#45837),(#45838,#45839),(#45840,#45841),(#45842,#45843),(#45844,
#45845),(#45846,#45847),(#45848,#45849),(#45850,#45851),(#45852,#45853),
(#45854,#45855),(#45856,#45857),(#45858,#45859),(#45860,#45861),(#45862,
#45863),(#45864,#45865),(#45866,#45867),(#45868,#45869),(#45870,#45871),
(#45872,#45873),(#45874,#45875),(#45876,#45877),(#45878,#45879),(#45880,
#45881),(#45882,#45883),(#45884,#45885),(#45886,#45887),(#45888,#45889),
(#45890,#45891),(#45892,#45893),(#45894,#45895),(#45896,#45897),(#45898,
#45899)),.UNSPECIFIED.,.F.,.F.,.F.)
B_SPLINE_SURFACE_WITH_KNOTS((6,1,1,1,1,1,1,1,1,1,1,1,1,1,1,1,1,1,1,1,1,
1,1,1,1,1,1,1,1,1,1,1,1,1,1,6),(2,2),(-1.,-0.971428571428572,-0.942857142857143,
-0.914285714285714,-0.885714285714286,-0.857142857142857,-0.828571428571429,
-0.8,-0.771428571428572,-0.742857142857143,-0.714285714285714,-0.685714285714286,
-0.657142857142857,-0.628571428571429,-0.6,-0.571428571428572,-0.542857142857143,
-0.514285714285714,-0.485714285714286,-0.457142857142857,-0.428571428571429,
-0.4,-0.371428571428571,-0.342857142857143,-0.314285714285714,-0.285714285714286,
-0.257142857142857,-0.228571428571429,-0.2,-0.171428571428571,-0.142857142857143,
-0.114285714285714,-0.0857142857142857,-0.0571428571428571,-0.0285714285714286,
0.),(0.,1.6),.UNSPECIFIED.)
GEOMETRIC_REPRESENTATION_ITEM()
RATIONAL_B_SPLINE_SURFACE(((1.,1.),(1.,1.),(1.,1.),(1.,1.),(1.,1.),(1.,
1.),(1.,1.),(1.,1.),(1.,1.),(1.,1.),(1.,1.),(1.,1.),(1.,1.),(1.,1.),(1.,
1.),(1.,1.),(1.,1.),(1.,1.),(1.,1.),(1.,1.),(1.,1.),(1.,1.),(1.,1.),(1.,
1.),(1.,1.),(1.,1.),(1.,1.),(1.,1.),(1.,1.),(1.,1.),(1.,1.),(1.,1.),(1.,
1.),(1.,1.),(1.,1.),(1.,1.),(1.,1.),(1.,1.),(1.,1.),(1.,1.)))
REPRESENTATION_ITEM('')
SURFACE()
);
#522=(
BOUNDED_SURFACE()
B_SPLINE_SURFACE(5,1,((#46020,#46021),(#46022,#46023),(#46024,#46025),(#46026,
#46027),(#46028,#46029),(#46030,#46031),(#46032,#46033),(#46034,#46035),
(#46036,#46037),(#46038,#46039),(#46040,#46041),(#46042,#46043),(#46044,
#46045),(#46046,#46047),(#46048,#46049),(#46050,#46051),(#46052,#46053),
(#46054,#46055),(#46056,#46057),(#46058,#46059),(#46060,#46061),(#46062,
#46063),(#46064,#46065),(#46066,#46067),(#46068,#46069),(#46070,#46071),
(#46072,#46073),(#46074,#46075),(#46076,#46077),(#46078,#46079),(#46080,
#46081),(#46082,#46083),(#46084,#46085),(#46086,#46087),(#46088,#46089),
(#46090,#46091),(#46092,#46093),(#46094,#46095),(#46096,#46097),(#46098,
#46099)),.UNSPECIFIED.,.F.,.F.,.F.)
B_SPLINE_SURFACE_WITH_KNOTS((6,1,1,1,1,1,1,1,1,1,1,1,1,1,1,1,1,1,1,1,1,
1,1,1,1,1,1,1,1,1,1,1,1,1,1,6),(2,2),(-1.,-0.971428571428572,-0.942857142857143,
-0.914285714285714,-0.885714285714286,-0.857142857142857,-0.828571428571429,
-0.8,-0.771428571428572,-0.742857142857143,-0.714285714285714,-0.685714285714286,
-0.657142857142857,-0.628571428571429,-0.6,-0.571428571428572,-0.542857142857143,
-0.514285714285714,-0.485714285714286,-0.457142857142857,-0.428571428571429,
-0.4,-0.371428571428571,-0.342857142857143,-0.314285714285714,-0.285714285714286,
-0.257142857142857,-0.228571428571429,-0.2,-0.171428571428571,-0.142857142857143,
-0.114285714285714,-0.0857142857142857,-0.0571428571428571,-0.0285714285714286,
0.),(0.,1.6),.UNSPECIFIED.)
GEOMETRIC_REPRESENTATION_ITEM()
RATIONAL_B_SPLINE_SURFACE(((1.,1.),(1.,1.),(1.,1.),(1.,1.),(1.,1.),(1.,
1.),(1.,1.),(1.,1.),(1.,1.),(1.,1.),(1.,1.),(1.,1.),(1.,1.),(1.,1.),(1.,
1.),(1.,1.),(1.,1.),(1.,1.),(1.,1.),(1.,1.),(1.,1.),(1.,1.),(1.,1.),(1.,
1.),(1.,1.),(1.,1.),(1.,1.),(1.,1.),(1.,1.),(1.,1.),(1.,1.),(1.,1.),(1.,
1.),(1.,1.),(1.,1.),(1.,1.),(1.,1.),(1.,1.),(1.,1.),(1.,1.)))
REPRESENTATION_ITEM('')
SURFACE()
);
#523=(
BOUNDED_SURFACE()
B_SPLINE_SURFACE(5,1,((#46148,#46149),(#46150,#46151),(#46152,#46153),(#46154,
#46155),(#46156,#46157),(#46158,#46159),(#46160,#46161),(#46162,#46163),
(#46164,#46165),(#46166,#46167),(#46168,#46169),(#46170,#46171),(#46172,
#46173),(#46174,#46175),(#46176,#46177),(#46178,#46179),(#46180,#46181),
(#46182,#46183),(#46184,#46185),(#46186,#46187),(#46188,#46189),(#46190,
#46191),(#46192,#46193),(#46194,#46195),(#46196,#46197),(#46198,#46199),
(#46200,#46201),(#46202,#46203),(#46204,#46205),(#46206,#46207),(#46208,
#46209),(#46210,#46211),(#46212,#46213),(#46214,#46215),(#46216,#46217),
(#46218,#46219),(#46220,#46221),(#46222,#46223),(#46224,#46225),(#46226,
#46227)),.UNSPECIFIED.,.F.,.F.,.F.)
B_SPLINE_SURFACE_WITH_KNOTS((6,1,1,1,1,1,1,1,1,1,1,1,1,1,1,1,1,1,1,1,1,
1,1,1,1,1,1,1,1,1,1,1,1,1,1,6),(2,2),(-1.,-0.971428571428572,-0.942857142857143,
-0.914285714285714,-0.885714285714286,-0.857142857142857,-0.828571428571429,
-0.8,-0.771428571428572,-0.742857142857143,-0.714285714285714,-0.685714285714286,
-0.657142857142857,-0.628571428571429,-0.6,-0.571428571428572,-0.542857142857143,
-0.514285714285714,-0.485714285714286,-0.457142857142857,-0.428571428571429,
-0.4,-0.371428571428571,-0.342857142857143,-0.314285714285714,-0.285714285714286,
-0.257142857142857,-0.228571428571429,-0.2,-0.171428571428571,-0.142857142857143,
-0.114285714285714,-0.0857142857142857,-0.0571428571428571,-0.0285714285714286,
0.),(0.,1.6),.UNSPECIFIED.)
GEOMETRIC_REPRESENTATION_ITEM()
RATIONAL_B_SPLINE_SURFACE(((1.,1.),(1.,1.),(1.,1.),(1.,1.),(1.,1.),(1.,
1.),(1.,1.),(1.,1.),(1.,1.),(1.,1.),(1.,1.),(1.,1.),(1.,1.),(1.,1.),(1.,
1.),(1.,1.),(1.,1.),(1.,1.),(1.,1.),(1.,1.),(1.,1.),(1.,1.),(1.,1.),(1.,
1.),(1.,1.),(1.,1.),(1.,1.),(1.,1.),(1.,1.),(1.,1.),(1.,1.),(1.,1.),(1.,
1.),(1.,1.),(1.,1.),(1.,1.),(1.,1.),(1.,1.),(1.,1.),(1.,1.)))
REPRESENTATION_ITEM('')
SURFACE()
);
#524=(
BOUNDED_SURFACE()
B_SPLINE_SURFACE(5,1,((#46342,#46343),(#46344,#46345),(#46346,#46347),(#46348,
#46349),(#46350,#46351),(#46352,#46353),(#46354,#46355),(#46356,#46357),
(#46358,#46359),(#46360,#46361),(#46362,#46363),(#46364,#46365),(#46366,
#46367),(#46368,#46369),(#46370,#46371),(#46372,#46373),(#46374,#46375),
(#46376,#46377),(#46378,#46379),(#46380,#46381),(#46382,#46383),(#46384,
#46385),(#46386,#46387),(#46388,#46389),(#46390,#46391),(#46392,#46393),
(#46394,#46395),(#46396,#46397),(#46398,#46399),(#46400,#46401),(#46402,
#46403),(#46404,#46405),(#46406,#46407),(#46408,#46409),(#46410,#46411),
(#46412,#46413),(#46414,#46415),(#46416,#46417),(#46418,#46419),(#46420,
#46421)),.UNSPECIFIED.,.F.,.F.,.F.)
B_SPLINE_SURFACE_WITH_KNOTS((6,1,1,1,1,1,1,1,1,1,1,1,1,1,1,1,1,1,1,1,1,
1,1,1,1,1,1,1,1,1,1,1,1,1,1,6),(2,2),(-1.,-0.971428571428572,-0.942857142857143,
-0.914285714285714,-0.885714285714286,-0.857142857142857,-0.828571428571429,
-0.8,-0.771428571428572,-0.742857142857143,-0.714285714285714,-0.685714285714286,
-0.657142857142857,-0.628571428571429,-0.6,-0.571428571428572,-0.542857142857143,
-0.514285714285714,-0.485714285714286,-0.457142857142857,-0.428571428571429,
-0.4,-0.371428571428571,-0.342857142857143,-0.314285714285714,-0.285714285714286,
-0.257142857142857,-0.228571428571429,-0.2,-0.171428571428571,-0.142857142857143,
-0.114285714285714,-0.0857142857142857,-0.0571428571428571,-0.0285714285714286,
0.),(0.,1.6),.UNSPECIFIED.)
GEOMETRIC_REPRESENTATION_ITEM()
RATIONAL_B_SPLINE_SURFACE(((1.,1.),(1.,1.),(1.,1.),(1.,1.),(1.,1.),(1.,
1.),(1.,1.),(1.,1.),(1.,1.),(1.,1.),(1.,1.),(1.,1.),(1.,1.),(1.,1.),(1.,
1.),(1.,1.),(1.,1.),(1.,1.),(1.,1.),(1.,1.),(1.,1.),(1.,1.),(1.,1.),(1.,
1.),(1.,1.),(1.,1.),(1.,1.),(1.,1.),(1.,1.),(1.,1.),(1.,1.),(1.,1.),(1.,
1.),(1.,1.),(1.,1.),(1.,1.),(1.,1.),(1.,1.),(1.,1.),(1.,1.)))
REPRESENTATION_ITEM('')
SURFACE()
);
#525=(
BOUNDED_SURFACE()
B_SPLINE_SURFACE(5,1,((#46470,#46471),(#46472,#46473),(#46474,#46475),(#46476,
#46477),(#46478,#46479),(#46480,#46481),(#46482,#46483),(#46484,#46485),
(#46486,#46487),(#46488,#46489),(#46490,#46491),(#46492,#46493),(#46494,
#46495),(#46496,#46497),(#46498,#46499),(#46500,#46501),(#46502,#46503),
(#46504,#46505),(#46506,#46507),(#46508,#46509),(#46510,#46511),(#46512,
#46513),(#46514,#46515),(#46516,#46517),(#46518,#46519),(#46520,#46521),
(#46522,#46523),(#46524,#46525),(#46526,#46527),(#46528,#46529),(#46530,
#46531),(#46532,#46533),(#46534,#46535),(#46536,#46537),(#46538,#46539),
(#46540,#46541),(#46542,#46543),(#46544,#46545),(#46546,#46547),(#46548,
#46549)),.UNSPECIFIED.,.F.,.F.,.F.)
B_SPLINE_SURFACE_WITH_KNOTS((6,1,1,1,1,1,1,1,1,1,1,1,1,1,1,1,1,1,1,1,1,
1,1,1,1,1,1,1,1,1,1,1,1,1,1,6),(2,2),(-1.,-0.971428571428572,-0.942857142857143,
-0.914285714285714,-0.885714285714286,-0.857142857142857,-0.828571428571429,
-0.8,-0.771428571428572,-0.742857142857143,-0.714285714285714,-0.685714285714286,
-0.657142857142857,-0.628571428571429,-0.6,-0.571428571428572,-0.542857142857143,
-0.514285714285714,-0.485714285714286,-0.457142857142857,-0.428571428571429,
-0.4,-0.371428571428571,-0.342857142857143,-0.314285714285714,-0.285714285714286,
-0.257142857142857,-0.228571428571429,-0.2,-0.171428571428571,-0.142857142857143,
-0.114285714285714,-0.0857142857142857,-0.0571428571428571,-0.0285714285714286,
0.),(0.,1.6),.UNSPECIFIED.)
GEOMETRIC_REPRESENTATION_ITEM()
RATIONAL_B_SPLINE_SURFACE(((1.,1.),(1.,1.),(1.,1.),(1.,1.),(1.,1.),(1.,
1.),(1.,1.),(1.,1.),(1.,1.),(1.,1.),(1.,1.),(1.,1.),(1.,1.),(1.,1.),(1.,
1.),(1.,1.),(1.,1.),(1.,1.),(1.,1.),(1.,1.),(1.,1.),(1.,1.),(1.,1.),(1.,
1.),(1.,1.),(1.,1.),(1.,1.),(1.,1.),(1.,1.),(1.,1.),(1.,1.),(1.,1.),(1.,
1.),(1.,1.),(1.,1.),(1.,1.),(1.,1.),(1.,1.),(1.,1.),(1.,1.)))
REPRESENTATION_ITEM('')
SURFACE()
);
#526=(
BOUNDED_SURFACE()
B_SPLINE_SURFACE(5,1,((#46664,#46665),(#46666,#46667),(#46668,#46669),(#46670,
#46671),(#46672,#46673),(#46674,#46675),(#46676,#46677),(#46678,#46679),
(#46680,#46681),(#46682,#46683),(#46684,#46685),(#46686,#46687),(#46688,
#46689),(#46690,#46691),(#46692,#46693),(#46694,#46695),(#46696,#46697),
(#46698,#46699),(#46700,#46701),(#46702,#46703),(#46704,#46705),(#46706,
#46707),(#46708,#46709),(#46710,#46711),(#46712,#46713),(#46714,#46715),
(#46716,#46717),(#46718,#46719),(#46720,#46721),(#46722,#46723),(#46724,
#46725),(#46726,#46727),(#46728,#46729),(#46730,#46731),(#46732,#46733),
(#46734,#46735),(#46736,#46737),(#46738,#46739),(#46740,#46741),(#46742,
#46743)),.UNSPECIFIED.,.F.,.F.,.F.)
B_SPLINE_SURFACE_WITH_KNOTS((6,1,1,1,1,1,1,1,1,1,1,1,1,1,1,1,1,1,1,1,1,
1,1,1,1,1,1,1,1,1,1,1,1,1,1,6),(2,2),(-1.,-0.971428571428572,-0.942857142857143,
-0.914285714285714,-0.885714285714286,-0.857142857142857,-0.828571428571429,
-0.8,-0.771428571428572,-0.742857142857143,-0.714285714285714,-0.685714285714286,
-0.657142857142857,-0.628571428571429,-0.6,-0.571428571428572,-0.542857142857143,
-0.514285714285714,-0.485714285714286,-0.457142857142857,-0.428571428571429,
-0.4,-0.371428571428571,-0.342857142857143,-0.314285714285714,-0.285714285714286,
-0.257142857142857,-0.228571428571429,-0.2,-0.171428571428571,-0.142857142857143,
-0.114285714285714,-0.0857142857142857,-0.0571428571428571,-0.0285714285714286,
0.),(0.,1.6),.UNSPECIFIED.)
GEOMETRIC_REPRESENTATION_ITEM()
RATIONAL_B_SPLINE_SURFACE(((1.,1.),(1.,1.),(1.,1.),(1.,1.),(1.,1.),(1.,
1.),(1.,1.),(1.,1.),(1.,1.),(1.,1.),(1.,1.),(1.,1.),(1.,1.),(1.,1.),(1.,
1.),(1.,1.),(1.,1.),(1.,1.),(1.,1.),(1.,1.),(1.,1.),(1.,1.),(1.,1.),(1.,
1.),(1.,1.),(1.,1.),(1.,1.),(1.,1.),(1.,1.),(1.,1.),(1.,1.),(1.,1.),(1.,
1.),(1.,1.),(1.,1.),(1.,1.),(1.,1.),(1.,1.),(1.,1.),(1.,1.)))
REPRESENTATION_ITEM('')
SURFACE()
);
#527=(
BOUNDED_SURFACE()
B_SPLINE_SURFACE(5,1,((#46792,#46793),(#46794,#46795),(#46796,#46797),(#46798,
#46799),(#46800,#46801),(#46802,#46803),(#46804,#46805),(#46806,#46807),
(#46808,#46809),(#46810,#46811),(#46812,#46813),(#46814,#46815),(#46816,
#46817),(#46818,#46819),(#46820,#46821),(#46822,#46823),(#46824,#46825),
(#46826,#46827),(#46828,#46829),(#46830,#46831),(#46832,#46833),(#46834,
#46835),(#46836,#46837),(#46838,#46839),(#46840,#46841),(#46842,#46843),
(#46844,#46845),(#46846,#46847),(#46848,#46849),(#46850,#46851),(#46852,
#46853),(#46854,#46855),(#46856,#46857),(#46858,#46859),(#46860,#46861),
(#46862,#46863),(#46864,#46865),(#46866,#46867),(#46868,#46869),(#46870,
#46871)),.UNSPECIFIED.,.F.,.F.,.F.)
B_SPLINE_SURFACE_WITH_KNOTS((6,1,1,1,1,1,1,1,1,1,1,1,1,1,1,1,1,1,1,1,1,
1,1,1,1,1,1,1,1,1,1,1,1,1,1,6),(2,2),(-1.,-0.971428571428572,-0.942857142857143,
-0.914285714285714,-0.885714285714286,-0.857142857142857,-0.828571428571429,
-0.8,-0.771428571428572,-0.742857142857143,-0.714285714285714,-0.685714285714286,
-0.657142857142857,-0.628571428571429,-0.6,-0.571428571428572,-0.542857142857143,
-0.514285714285714,-0.485714285714286,-0.457142857142857,-0.428571428571429,
-0.4,-0.371428571428571,-0.342857142857143,-0.314285714285714,-0.285714285714286,
-0.257142857142857,-0.228571428571429,-0.2,-0.171428571428571,-0.142857142857143,
-0.114285714285714,-0.0857142857142857,-0.0571428571428571,-0.0285714285714286,
0.),(0.,1.6),.UNSPECIFIED.)
GEOMETRIC_REPRESENTATION_ITEM()
RATIONAL_B_SPLINE_SURFACE(((1.,1.),(1.,1.),(1.,1.),(1.,1.),(1.,1.),(1.,
1.),(1.,1.),(1.,1.),(1.,1.),(1.,1.),(1.,1.),(1.,1.),(1.,1.),(1.,1.),(1.,
1.),(1.,1.),(1.,1.),(1.,1.),(1.,1.),(1.,1.),(1.,1.),(1.,1.),(1.,1.),(1.,
1.),(1.,1.),(1.,1.),(1.,1.),(1.,1.),(1.,1.),(1.,1.),(1.,1.),(1.,1.),(1.,
1.),(1.,1.),(1.,1.),(1.,1.),(1.,1.),(1.,1.),(1.,1.),(1.,1.)))
REPRESENTATION_ITEM('')
SURFACE()
);
#528=(
BOUNDED_SURFACE()
B_SPLINE_SURFACE(5,1,((#46926,#46927),(#46928,#46929),(#46930,#46931),(#46932,
#46933),(#46934,#46935),(#46936,#46937),(#46938,#46939),(#46940,#46941),
(#46942,#46943),(#46944,#46945),(#46946,#46947),(#46948,#46949),(#46950,
#46951),(#46952,#46953),(#46954,#46955),(#46956,#46957),(#46958,#46959),
(#46960,#46961),(#46962,#46963),(#46964,#46965),(#46966,#46967),(#46968,
#46969),(#46970,#46971),(#46972,#46973),(#46974,#46975),(#46976,#46977),
(#46978,#46979),(#46980,#46981),(#46982,#46983),(#46984,#46985),(#46986,
#46987),(#46988,#46989),(#46990,#46991),(#46992,#46993),(#46994,#46995),
(#46996,#46997),(#46998,#46999),(#47000,#47001),(#47002,#47003),(#47004,
#47005)),.UNSPECIFIED.,.F.,.F.,.F.)
B_SPLINE_SURFACE_WITH_KNOTS((6,1,1,1,1,1,1,1,1,1,1,1,1,1,1,1,1,1,1,1,1,
1,1,1,1,1,1,1,1,1,1,1,1,1,1,6),(2,2),(-1.,-0.971428571428572,-0.942857142857143,
-0.914285714285714,-0.885714285714286,-0.857142857142857,-0.828571428571429,
-0.8,-0.771428571428572,-0.742857142857143,-0.714285714285714,-0.685714285714286,
-0.657142857142857,-0.628571428571429,-0.6,-0.571428571428572,-0.542857142857143,
-0.514285714285714,-0.485714285714286,-0.457142857142857,-0.428571428571429,
-0.4,-0.371428571428571,-0.342857142857143,-0.314285714285714,-0.285714285714286,
-0.257142857142857,-0.228571428571429,-0.2,-0.171428571428571,-0.142857142857143,
-0.114285714285714,-0.0857142857142857,-0.0571428571428571,-0.0285714285714286,
0.),(0.,1.6),.UNSPECIFIED.)
GEOMETRIC_REPRESENTATION_ITEM()
RATIONAL_B_SPLINE_SURFACE(((1.,1.),(1.,1.),(1.,1.),(1.,1.),(1.,1.),(1.,
1.),(1.,1.),(1.,1.),(1.,1.),(1.,1.),(1.,1.),(1.,1.),(1.,1.),(1.,1.),(1.,
1.),(1.,1.),(1.,1.),(1.,1.),(1.,1.),(1.,1.),(1.,1.),(1.,1.),(1.,1.),(1.,
1.),(1.,1.),(1.,1.),(1.,1.),(1.,1.),(1.,1.),(1.,1.),(1.,1.),(1.,1.),(1.,
1.),(1.,1.),(1.,1.),(1.,1.),(1.,1.),(1.,1.),(1.,1.),(1.,1.)))
REPRESENTATION_ITEM('')
SURFACE()
);
#529=(
BOUNDED_SURFACE()
B_SPLINE_SURFACE(5,1,((#47100,#47101),(#47102,#47103),(#47104,#47105),(#47106,
#47107),(#47108,#47109),(#47110,#47111),(#47112,#47113),(#47114,#47115),
(#47116,#47117),(#47118,#47119),(#47120,#47121),(#47122,#47123),(#47124,
#47125),(#47126,#47127),(#47128,#47129),(#47130,#47131),(#47132,#47133),
(#47134,#47135),(#47136,#47137),(#47138,#47139),(#47140,#47141),(#47142,
#47143),(#47144,#47145),(#47146,#47147),(#47148,#47149),(#47150,#47151),
(#47152,#47153),(#47154,#47155),(#47156,#47157),(#47158,#47159),(#47160,
#47161),(#47162,#47163),(#47164,#47165),(#47166,#47167),(#47168,#47169),
(#47170,#47171),(#47172,#47173),(#47174,#47175),(#47176,#47177),(#47178,
#47179)),.UNSPECIFIED.,.F.,.F.,.F.)
B_SPLINE_SURFACE_WITH_KNOTS((6,1,1,1,1,1,1,1,1,1,1,1,1,1,1,1,1,1,1,1,1,
1,1,1,1,1,1,1,1,1,1,1,1,1,1,6),(2,2),(-1.,-0.971428571428572,-0.942857142857143,
-0.914285714285714,-0.885714285714286,-0.857142857142857,-0.828571428571429,
-0.8,-0.771428571428572,-0.742857142857143,-0.714285714285714,-0.685714285714286,
-0.657142857142857,-0.628571428571429,-0.6,-0.571428571428572,-0.542857142857143,
-0.514285714285714,-0.485714285714286,-0.457142857142857,-0.428571428571429,
-0.4,-0.371428571428571,-0.342857142857143,-0.314285714285714,-0.285714285714286,
-0.257142857142857,-0.228571428571429,-0.2,-0.171428571428571,-0.142857142857143,
-0.114285714285714,-0.0857142857142857,-0.0571428571428571,-0.0285714285714286,
0.),(0.,1.6),.UNSPECIFIED.)
GEOMETRIC_REPRESENTATION_ITEM()
RATIONAL_B_SPLINE_SURFACE(((1.,1.),(1.,1.),(1.,1.),(1.,1.),(1.,1.),(1.,
1.),(1.,1.),(1.,1.),(1.,1.),(1.,1.),(1.,1.),(1.,1.),(1.,1.),(1.,1.),(1.,
1.),(1.,1.),(1.,1.),(1.,1.),(1.,1.),(1.,1.),(1.,1.),(1.,1.),(1.,1.),(1.,
1.),(1.,1.),(1.,1.),(1.,1.),(1.,1.),(1.,1.),(1.,1.),(1.,1.),(1.,1.),(1.,
1.),(1.,1.),(1.,1.),(1.,1.),(1.,1.),(1.,1.),(1.,1.),(1.,1.)))
REPRESENTATION_ITEM('')
SURFACE()
);
#530=(
BOUNDED_SURFACE()
B_SPLINE_SURFACE(5,1,((#51613,#51614),(#51615,#51616),(#51617,#51618),(#51619,
#51620),(#51621,#51622),(#51623,#51624),(#51625,#51626),(#51627,#51628),
(#51629,#51630),(#51631,#51632),(#51633,#51634),(#51635,#51636),(#51637,
#51638),(#51639,#51640),(#51641,#51642),(#51643,#51644),(#51645,#51646),
(#51647,#51648),(#51649,#51650),(#51651,#51652),(#51653,#51654),(#51655,
#51656),(#51657,#51658),(#51659,#51660),(#51661,#51662),(#51663,#51664),
(#51665,#51666),(#51667,#51668),(#51669,#51670),(#51671,#51672),(#51673,
#51674),(#51675,#51676),(#51677,#51678),(#51679,#51680),(#51681,#51682),
(#51683,#51684),(#51685,#51686),(#51687,#51688),(#51689,#51690),(#51691,
#51692)),.UNSPECIFIED.,.F.,.F.,.F.)
B_SPLINE_SURFACE_WITH_KNOTS((6,1,1,1,1,1,1,1,1,1,1,1,1,1,1,1,1,1,1,1,1,
1,1,1,1,1,1,1,1,1,1,1,1,1,1,6),(2,2),(-1.,-0.971428571428572,-0.942857142857143,
-0.914285714285714,-0.885714285714286,-0.857142857142857,-0.828571428571429,
-0.8,-0.771428571428572,-0.742857142857143,-0.714285714285714,-0.685714285714286,
-0.657142857142857,-0.628571428571429,-0.6,-0.571428571428572,-0.542857142857143,
-0.514285714285714,-0.485714285714286,-0.457142857142857,-0.428571428571429,
-0.4,-0.371428571428571,-0.342857142857143,-0.314285714285714,-0.285714285714286,
-0.257142857142857,-0.228571428571429,-0.2,-0.171428571428571,-0.142857142857143,
-0.114285714285714,-0.0857142857142857,-0.0571428571428571,-0.0285714285714286,
0.),(0.,2.9),.UNSPECIFIED.)
GEOMETRIC_REPRESENTATION_ITEM()
RATIONAL_B_SPLINE_SURFACE(((1.,1.),(1.,1.),(1.,1.),(1.,1.),(1.,1.),(1.,
1.),(1.,1.),(1.,1.),(1.,1.),(1.,1.),(1.,1.),(1.,1.),(1.,1.),(1.,1.),(1.,
1.),(1.,1.),(1.,1.),(1.,1.),(1.,1.),(1.,1.),(1.,1.),(1.,1.),(1.,1.),(1.,
1.),(1.,1.),(1.,1.),(1.,1.),(1.,1.),(1.,1.),(1.,1.),(1.,1.),(1.,1.),(1.,
1.),(1.,1.),(1.,1.),(1.,1.),(1.,1.),(1.,1.),(1.,1.),(1.,1.)))
REPRESENTATION_ITEM('')
SURFACE()
);
#531=(
BOUNDED_SURFACE()
B_SPLINE_SURFACE(5,1,((#51748,#51749),(#51750,#51751),(#51752,#51753),(#51754,
#51755),(#51756,#51757),(#51758,#51759),(#51760,#51761),(#51762,#51763),
(#51764,#51765),(#51766,#51767),(#51768,#51769),(#51770,#51771),(#51772,
#51773),(#51774,#51775),(#51776,#51777),(#51778,#51779),(#51780,#51781),
(#51782,#51783),(#51784,#51785),(#51786,#51787),(#51788,#51789),(#51790,
#51791),(#51792,#51793),(#51794,#51795),(#51796,#51797),(#51798,#51799),
(#51800,#51801),(#51802,#51803),(#51804,#51805),(#51806,#51807),(#51808,
#51809),(#51810,#51811),(#51812,#51813),(#51814,#51815),(#51816,#51817),
(#51818,#51819),(#51820,#51821),(#51822,#51823),(#51824,#51825),(#51826,
#51827)),.UNSPECIFIED.,.F.,.F.,.F.)
B_SPLINE_SURFACE_WITH_KNOTS((6,1,1,1,1,1,1,1,1,1,1,1,1,1,1,1,1,1,1,1,1,
1,1,1,1,1,1,1,1,1,1,1,1,1,1,6),(2,2),(-1.,-0.971428571428572,-0.942857142857143,
-0.914285714285714,-0.885714285714286,-0.857142857142857,-0.828571428571429,
-0.8,-0.771428571428572,-0.742857142857143,-0.714285714285714,-0.685714285714286,
-0.657142857142857,-0.628571428571429,-0.6,-0.571428571428572,-0.542857142857143,
-0.514285714285714,-0.485714285714286,-0.457142857142857,-0.428571428571429,
-0.4,-0.371428571428571,-0.342857142857143,-0.314285714285714,-0.285714285714286,
-0.257142857142857,-0.228571428571429,-0.2,-0.171428571428571,-0.142857142857143,
-0.114285714285714,-0.0857142857142857,-0.0571428571428571,-0.0285714285714286,
0.),(0.,2.9),.UNSPECIFIED.)
GEOMETRIC_REPRESENTATION_ITEM()
RATIONAL_B_SPLINE_SURFACE(((1.,1.),(1.,1.),(1.,1.),(1.,1.),(1.,1.),(1.,
1.),(1.,1.),(1.,1.),(1.,1.),(1.,1.),(1.,1.),(1.,1.),(1.,1.),(1.,1.),(1.,
1.),(1.,1.),(1.,1.),(1.,1.),(1.,1.),(1.,1.),(1.,1.),(1.,1.),(1.,1.),(1.,
1.),(1.,1.),(1.,1.),(1.,1.),(1.,1.),(1.,1.),(1.,1.),(1.,1.),(1.,1.),(1.,
1.),(1.,1.),(1.,1.),(1.,1.),(1.,1.),(1.,1.),(1.,1.),(1.,1.)))
REPRESENTATION_ITEM('')
SURFACE()
);
#532=(
BOUNDED_SURFACE()
B_SPLINE_SURFACE(5,1,((#51889,#51890),(#51891,#51892),(#51893,#51894),(#51895,
#51896),(#51897,#51898),(#51899,#51900),(#51901,#51902),(#51903,#51904),
(#51905,#51906),(#51907,#51908),(#51909,#51910),(#51911,#51912),(#51913,
#51914),(#51915,#51916),(#51917,#51918),(#51919,#51920),(#51921,#51922),
(#51923,#51924),(#51925,#51926),(#51927,#51928),(#51929,#51930),(#51931,
#51932),(#51933,#51934),(#51935,#51936),(#51937,#51938),(#51939,#51940),
(#51941,#51942),(#51943,#51944),(#51945,#51946),(#51947,#51948),(#51949,
#51950),(#51951,#51952),(#51953,#51954),(#51955,#51956),(#51957,#51958),
(#51959,#51960),(#51961,#51962),(#51963,#51964),(#51965,#51966),(#51967,
#51968)),.UNSPECIFIED.,.F.,.F.,.F.)
B_SPLINE_SURFACE_WITH_KNOTS((6,1,1,1,1,1,1,1,1,1,1,1,1,1,1,1,1,1,1,1,1,
1,1,1,1,1,1,1,1,1,1,1,1,1,1,6),(2,2),(-1.,-0.971428571428572,-0.942857142857143,
-0.914285714285714,-0.885714285714286,-0.857142857142857,-0.828571428571429,
-0.8,-0.771428571428572,-0.742857142857143,-0.714285714285714,-0.685714285714286,
-0.657142857142857,-0.628571428571429,-0.6,-0.571428571428572,-0.542857142857143,
-0.514285714285714,-0.485714285714286,-0.457142857142857,-0.428571428571429,
-0.4,-0.371428571428571,-0.342857142857143,-0.314285714285714,-0.285714285714286,
-0.257142857142857,-0.228571428571429,-0.2,-0.171428571428571,-0.142857142857143,
-0.114285714285714,-0.0857142857142857,-0.0571428571428571,-0.0285714285714286,
0.),(0.,2.9),.UNSPECIFIED.)
GEOMETRIC_REPRESENTATION_ITEM()
RATIONAL_B_SPLINE_SURFACE(((1.,1.),(1.,1.),(1.,1.),(1.,1.),(1.,1.),(1.,
1.),(1.,1.),(1.,1.),(1.,1.),(1.,1.),(1.,1.),(1.,1.),(1.,1.),(1.,1.),(1.,
1.),(1.,1.),(1.,1.),(1.,1.),(1.,1.),(1.,1.),(1.,1.),(1.,1.),(1.,1.),(1.,
1.),(1.,1.),(1.,1.),(1.,1.),(1.,1.),(1.,1.),(1.,1.),(1.,1.),(1.,1.),(1.,
1.),(1.,1.),(1.,1.),(1.,1.),(1.,1.),(1.,1.),(1.,1.),(1.,1.)))
REPRESENTATION_ITEM('')
SURFACE()
);
#533=(
BOUNDED_SURFACE()
B_SPLINE_SURFACE(5,1,((#52018,#52019),(#52020,#52021),(#52022,#52023),(#52024,
#52025),(#52026,#52027),(#52028,#52029),(#52030,#52031),(#52032,#52033),
(#52034,#52035),(#52036,#52037),(#52038,#52039),(#52040,#52041),(#52042,
#52043),(#52044,#52045),(#52046,#52047),(#52048,#52049),(#52050,#52051),
(#52052,#52053),(#52054,#52055),(#52056,#52057),(#52058,#52059),(#52060,
#52061),(#52062,#52063),(#52064,#52065),(#52066,#52067),(#52068,#52069),
(#52070,#52071),(#52072,#52073),(#52074,#52075),(#52076,#52077),(#52078,
#52079),(#52080,#52081),(#52082,#52083),(#52084,#52085),(#52086,#52087),
(#52088,#52089),(#52090,#52091),(#52092,#52093),(#52094,#52095),(#52096,
#52097)),.UNSPECIFIED.,.F.,.F.,.F.)
B_SPLINE_SURFACE_WITH_KNOTS((6,1,1,1,1,1,1,1,1,1,1,1,1,1,1,1,1,1,1,1,1,
1,1,1,1,1,1,1,1,1,1,1,1,1,1,6),(2,2),(-1.,-0.971428571428572,-0.942857142857143,
-0.914285714285714,-0.885714285714286,-0.857142857142857,-0.828571428571429,
-0.8,-0.771428571428572,-0.742857142857143,-0.714285714285714,-0.685714285714286,
-0.657142857142857,-0.628571428571429,-0.6,-0.571428571428572,-0.542857142857143,
-0.514285714285714,-0.485714285714286,-0.457142857142857,-0.428571428571429,
-0.4,-0.371428571428571,-0.342857142857143,-0.314285714285714,-0.285714285714286,
-0.257142857142857,-0.228571428571429,-0.2,-0.171428571428571,-0.142857142857143,
-0.114285714285714,-0.0857142857142857,-0.0571428571428571,-0.0285714285714286,
0.),(0.,2.9),.UNSPECIFIED.)
GEOMETRIC_REPRESENTATION_ITEM()
RATIONAL_B_SPLINE_SURFACE(((1.,1.),(1.,1.),(1.,1.),(1.,1.),(1.,1.),(1.,
1.),(1.,1.),(1.,1.),(1.,1.),(1.,1.),(1.,1.),(1.,1.),(1.,1.),(1.,1.),(1.,
1.),(1.,1.),(1.,1.),(1.,1.),(1.,1.),(1.,1.),(1.,1.),(1.,1.),(1.,1.),(1.,
1.),(1.,1.),(1.,1.),(1.,1.),(1.,1.),(1.,1.),(1.,1.),(1.,1.),(1.,1.),(1.,
1.),(1.,1.),(1.,1.),(1.,1.),(1.,1.),(1.,1.),(1.,1.),(1.,1.)))
REPRESENTATION_ITEM('')
SURFACE()
);
#534=(
BOUNDED_SURFACE()
B_SPLINE_SURFACE(5,1,((#54512,#54513),(#54514,#54515),(#54516,#54517),(#54518,
#54519),(#54520,#54521),(#54522,#54523),(#54524,#54525),(#54526,#54527),
(#54528,#54529),(#54530,#54531),(#54532,#54533),(#54534,#54535),(#54536,
#54537),(#54538,#54539),(#54540,#54541),(#54542,#54543),(#54544,#54545),
(#54546,#54547),(#54548,#54549),(#54550,#54551),(#54552,#54553),(#54554,
#54555),(#54556,#54557),(#54558,#54559),(#54560,#54561),(#54562,#54563),
(#54564,#54565),(#54566,#54567),(#54568,#54569),(#54570,#54571),(#54572,
#54573),(#54574,#54575),(#54576,#54577),(#54578,#54579),(#54580,#54581),
(#54582,#54583),(#54584,#54585),(#54586,#54587),(#54588,#54589),(#54590,
#54591)),.UNSPECIFIED.,.F.,.F.,.F.)
B_SPLINE_SURFACE_WITH_KNOTS((6,1,1,1,1,1,1,1,1,1,1,1,1,1,1,1,1,1,1,1,1,
1,1,1,1,1,1,1,1,1,1,1,1,1,1,6),(2,2),(-1.,-0.971428571428572,-0.942857142857143,
-0.914285714285714,-0.885714285714286,-0.857142857142857,-0.828571428571429,
-0.8,-0.771428571428572,-0.742857142857143,-0.714285714285714,-0.685714285714286,
-0.657142857142857,-0.628571428571429,-0.6,-0.571428571428572,-0.542857142857143,
-0.514285714285714,-0.485714285714286,-0.457142857142857,-0.428571428571429,
-0.4,-0.371428571428571,-0.342857142857143,-0.314285714285714,-0.285714285714286,
-0.257142857142857,-0.228571428571429,-0.2,-0.171428571428571,-0.142857142857143,
-0.114285714285714,-0.0857142857142857,-0.0571428571428571,-0.0285714285714286,
0.),(0.,2.9),.UNSPECIFIED.)
GEOMETRIC_REPRESENTATION_ITEM()
RATIONAL_B_SPLINE_SURFACE(((1.,1.),(1.,1.),(1.,1.),(1.,1.),(1.,1.),(1.,
1.),(1.,1.),(1.,1.),(1.,1.),(1.,1.),(1.,1.),(1.,1.),(1.,1.),(1.,1.),(1.,
1.),(1.,1.),(1.,1.),(1.,1.),(1.,1.),(1.,1.),(1.,1.),(1.,1.),(1.,1.),(1.,
1.),(1.,1.),(1.,1.),(1.,1.),(1.,1.),(1.,1.),(1.,1.),(1.,1.),(1.,1.),(1.,
1.),(1.,1.),(1.,1.),(1.,1.),(1.,1.),(1.,1.),(1.,1.),(1.,1.)))
REPRESENTATION_ITEM('')
SURFACE()
);
#535=(
BOUNDED_SURFACE()
B_SPLINE_SURFACE(5,1,((#54595,#54596),(#54597,#54598),(#54599,#54600),(#54601,
#54602),(#54603,#54604),(#54605,#54606),(#54607,#54608),(#54609,#54610),
(#54611,#54612),(#54613,#54614),(#54615,#54616),(#54617,#54618),(#54619,
#54620),(#54621,#54622),(#54623,#54624),(#54625,#54626),(#54627,#54628),
(#54629,#54630),(#54631,#54632),(#54633,#54634),(#54635,#54636),(#54637,
#54638),(#54639,#54640),(#54641,#54642),(#54643,#54644),(#54645,#54646),
(#54647,#54648),(#54649,#54650),(#54651,#54652),(#54653,#54654),(#54655,
#54656),(#54657,#54658),(#54659,#54660),(#54661,#54662),(#54663,#54664),
(#54665,#54666),(#54667,#54668),(#54669,#54670),(#54671,#54672),(#54673,
#54674)),.UNSPECIFIED.,.F.,.F.,.F.)
B_SPLINE_SURFACE_WITH_KNOTS((6,1,1,1,1,1,1,1,1,1,1,1,1,1,1,1,1,1,1,1,1,
1,1,1,1,1,1,1,1,1,1,1,1,1,1,6),(2,2),(-1.,-0.971428571428572,-0.942857142857143,
-0.914285714285714,-0.885714285714286,-0.857142857142857,-0.828571428571429,
-0.8,-0.771428571428572,-0.742857142857143,-0.714285714285714,-0.685714285714286,
-0.657142857142857,-0.628571428571429,-0.6,-0.571428571428572,-0.542857142857143,
-0.514285714285714,-0.485714285714286,-0.457142857142857,-0.428571428571429,
-0.4,-0.371428571428571,-0.342857142857143,-0.314285714285714,-0.285714285714286,
-0.257142857142857,-0.228571428571429,-0.2,-0.171428571428571,-0.142857142857143,
-0.114285714285714,-0.0857142857142857,-0.0571428571428571,-0.0285714285714286,
0.),(0.,2.9),.UNSPECIFIED.)
GEOMETRIC_REPRESENTATION_ITEM()
RATIONAL_B_SPLINE_SURFACE(((1.,1.),(1.,1.),(1.,1.),(1.,1.),(1.,1.),(1.,
1.),(1.,1.),(1.,1.),(1.,1.),(1.,1.),(1.,1.),(1.,1.),(1.,1.),(1.,1.),(1.,
1.),(1.,1.),(1.,1.),(1.,1.),(1.,1.),(1.,1.),(1.,1.),(1.,1.),(1.,1.),(1.,
1.),(1.,1.),(1.,1.),(1.,1.),(1.,1.),(1.,1.),(1.,1.),(1.,1.),(1.,1.),(1.,
1.),(1.,1.),(1.,1.),(1.,1.),(1.,1.),(1.,1.),(1.,1.),(1.,1.)))
REPRESENTATION_ITEM('')
SURFACE()
);
#536=(
BOUNDED_SURFACE()
B_SPLINE_SURFACE(5,1,((#54691,#54692),(#54693,#54694),(#54695,#54696),(#54697,
#54698),(#54699,#54700),(#54701,#54702),(#54703,#54704),(#54705,#54706),
(#54707,#54708),(#54709,#54710),(#54711,#54712),(#54713,#54714),(#54715,
#54716),(#54717,#54718),(#54719,#54720),(#54721,#54722),(#54723,#54724),
(#54725,#54726),(#54727,#54728),(#54729,#54730),(#54731,#54732),(#54733,
#54734),(#54735,#54736),(#54737,#54738),(#54739,#54740),(#54741,#54742),
(#54743,#54744),(#54745,#54746),(#54747,#54748),(#54749,#54750),(#54751,
#54752),(#54753,#54754),(#54755,#54756),(#54757,#54758),(#54759,#54760),
(#54761,#54762),(#54763,#54764),(#54765,#54766),(#54767,#54768),(#54769,
#54770)),.UNSPECIFIED.,.F.,.F.,.F.)
B_SPLINE_SURFACE_WITH_KNOTS((6,1,1,1,1,1,1,1,1,1,1,1,1,1,1,1,1,1,1,1,1,
1,1,1,1,1,1,1,1,1,1,1,1,1,1,6),(2,2),(-1.,-0.971428571428572,-0.942857142857143,
-0.914285714285714,-0.885714285714286,-0.857142857142857,-0.828571428571429,
-0.8,-0.771428571428572,-0.742857142857143,-0.714285714285714,-0.685714285714286,
-0.657142857142857,-0.628571428571429,-0.6,-0.571428571428572,-0.542857142857143,
-0.514285714285714,-0.485714285714286,-0.457142857142857,-0.428571428571429,
-0.4,-0.371428571428571,-0.342857142857143,-0.314285714285714,-0.285714285714286,
-0.257142857142857,-0.228571428571429,-0.2,-0.171428571428571,-0.142857142857143,
-0.114285714285714,-0.0857142857142857,-0.0571428571428571,-0.0285714285714286,
0.),(0.,2.9),.UNSPECIFIED.)
GEOMETRIC_REPRESENTATION_ITEM()
RATIONAL_B_SPLINE_SURFACE(((1.,1.),(1.,1.),(1.,1.),(1.,1.),(1.,1.),(1.,
1.),(1.,1.),(1.,1.),(1.,1.),(1.,1.),(1.,1.),(1.,1.),(1.,1.),(1.,1.),(1.,
1.),(1.,1.),(1.,1.),(1.,1.),(1.,1.),(1.,1.),(1.,1.),(1.,1.),(1.,1.),(1.,
1.),(1.,1.),(1.,1.),(1.,1.),(1.,1.),(1.,1.),(1.,1.),(1.,1.),(1.,1.),(1.,
1.),(1.,1.),(1.,1.),(1.,1.),(1.,1.),(1.,1.),(1.,1.),(1.,1.)))
REPRESENTATION_ITEM('')
SURFACE()
);
#537=(
BOUNDED_SURFACE()
B_SPLINE_SURFACE(5,1,((#54787,#54788),(#54789,#54790),(#54791,#54792),(#54793,
#54794),(#54795,#54796),(#54797,#54798),(#54799,#54800),(#54801,#54802),
(#54803,#54804),(#54805,#54806),(#54807,#54808),(#54809,#54810),(#54811,
#54812),(#54813,#54814),(#54815,#54816),(#54817,#54818),(#54819,#54820),
(#54821,#54822),(#54823,#54824),(#54825,#54826),(#54827,#54828),(#54829,
#54830),(#54831,#54832),(#54833,#54834),(#54835,#54836),(#54837,#54838),
(#54839,#54840),(#54841,#54842),(#54843,#54844),(#54845,#54846),(#54847,
#54848),(#54849,#54850),(#54851,#54852),(#54853,#54854),(#54855,#54856),
(#54857,#54858),(#54859,#54860),(#54861,#54862),(#54863,#54864),(#54865,
#54866)),.UNSPECIFIED.,.F.,.F.,.F.)
B_SPLINE_SURFACE_WITH_KNOTS((6,1,1,1,1,1,1,1,1,1,1,1,1,1,1,1,1,1,1,1,1,
1,1,1,1,1,1,1,1,1,1,1,1,1,1,6),(2,2),(-1.,-0.971428571428572,-0.942857142857143,
-0.914285714285714,-0.885714285714286,-0.857142857142857,-0.828571428571429,
-0.8,-0.771428571428572,-0.742857142857143,-0.714285714285714,-0.685714285714286,
-0.657142857142857,-0.628571428571429,-0.6,-0.571428571428572,-0.542857142857143,
-0.514285714285714,-0.485714285714286,-0.457142857142857,-0.428571428571429,
-0.4,-0.371428571428571,-0.342857142857143,-0.314285714285714,-0.285714285714286,
-0.257142857142857,-0.228571428571429,-0.2,-0.171428571428571,-0.142857142857143,
-0.114285714285714,-0.0857142857142857,-0.0571428571428571,-0.0285714285714286,
0.),(0.,2.9),.UNSPECIFIED.)
GEOMETRIC_REPRESENTATION_ITEM()
RATIONAL_B_SPLINE_SURFACE(((1.,1.),(1.,1.),(1.,1.),(1.,1.),(1.,1.),(1.,
1.),(1.,1.),(1.,1.),(1.,1.),(1.,1.),(1.,1.),(1.,1.),(1.,1.),(1.,1.),(1.,
1.),(1.,1.),(1.,1.),(1.,1.),(1.,1.),(1.,1.),(1.,1.),(1.,1.),(1.,1.),(1.,
1.),(1.,1.),(1.,1.),(1.,1.),(1.,1.),(1.,1.),(1.,1.),(1.,1.),(1.,1.),(1.,
1.),(1.,1.),(1.,1.),(1.,1.),(1.,1.),(1.,1.),(1.,1.),(1.,1.)))
REPRESENTATION_ITEM('')
SURFACE()
);
#538=(
BOUNDED_SURFACE()
B_SPLINE_SURFACE(5,1,((#54898,#54899),(#54900,#54901),(#54902,#54903),(#54904,
#54905),(#54906,#54907),(#54908,#54909),(#54910,#54911),(#54912,#54913),
(#54914,#54915),(#54916,#54917),(#54918,#54919),(#54920,#54921),(#54922,
#54923),(#54924,#54925),(#54926,#54927),(#54928,#54929),(#54930,#54931),
(#54932,#54933),(#54934,#54935),(#54936,#54937),(#54938,#54939),(#54940,
#54941),(#54942,#54943),(#54944,#54945),(#54946,#54947),(#54948,#54949),
(#54950,#54951),(#54952,#54953),(#54954,#54955),(#54956,#54957),(#54958,
#54959),(#54960,#54961),(#54962,#54963),(#54964,#54965),(#54966,#54967),
(#54968,#54969),(#54970,#54971),(#54972,#54973),(#54974,#54975),(#54976,
#54977)),.UNSPECIFIED.,.F.,.F.,.F.)
B_SPLINE_SURFACE_WITH_KNOTS((6,1,1,1,1,1,1,1,1,1,1,1,1,1,1,1,1,1,1,1,1,
1,1,1,1,1,1,1,1,1,1,1,1,1,1,6),(2,2),(-1.,-0.971428571428572,-0.942857142857143,
-0.914285714285714,-0.885714285714286,-0.857142857142857,-0.828571428571429,
-0.8,-0.771428571428572,-0.742857142857143,-0.714285714285714,-0.685714285714286,
-0.657142857142857,-0.628571428571429,-0.6,-0.571428571428572,-0.542857142857143,
-0.514285714285714,-0.485714285714286,-0.457142857142857,-0.428571428571429,
-0.4,-0.371428571428571,-0.342857142857143,-0.314285714285714,-0.285714285714286,
-0.257142857142857,-0.228571428571429,-0.2,-0.171428571428571,-0.142857142857143,
-0.114285714285714,-0.0857142857142857,-0.0571428571428571,-0.0285714285714286,
0.),(0.,2.9),.UNSPECIFIED.)
GEOMETRIC_REPRESENTATION_ITEM()
RATIONAL_B_SPLINE_SURFACE(((1.,1.),(1.,1.),(1.,1.),(1.,1.),(1.,1.),(1.,
1.),(1.,1.),(1.,1.),(1.,1.),(1.,1.),(1.,1.),(1.,1.),(1.,1.),(1.,1.),(1.,
1.),(1.,1.),(1.,1.),(1.,1.),(1.,1.),(1.,1.),(1.,1.),(1.,1.),(1.,1.),(1.,
1.),(1.,1.),(1.,1.),(1.,1.),(1.,1.),(1.,1.),(1.,1.),(1.,1.),(1.,1.),(1.,
1.),(1.,1.),(1.,1.),(1.,1.),(1.,1.),(1.,1.),(1.,1.),(1.,1.)))
REPRESENTATION_ITEM('')
SURFACE()
);
#539=(
BOUNDED_SURFACE()
B_SPLINE_SURFACE(5,1,((#54981,#54982),(#54983,#54984),(#54985,#54986),(#54987,
#54988),(#54989,#54990),(#54991,#54992),(#54993,#54994),(#54995,#54996),
(#54997,#54998),(#54999,#55000),(#55001,#55002),(#55003,#55004),(#55005,
#55006),(#55007,#55008),(#55009,#55010),(#55011,#55012),(#55013,#55014),
(#55015,#55016),(#55017,#55018),(#55019,#55020),(#55021,#55022),(#55023,
#55024),(#55025,#55026),(#55027,#55028),(#55029,#55030),(#55031,#55032),
(#55033,#55034),(#55035,#55036),(#55037,#55038),(#55039,#55040),(#55041,
#55042),(#55043,#55044),(#55045,#55046),(#55047,#55048),(#55049,#55050),
(#55051,#55052),(#55053,#55054),(#55055,#55056),(#55057,#55058),(#55059,
#55060)),.UNSPECIFIED.,.F.,.F.,.F.)
B_SPLINE_SURFACE_WITH_KNOTS((6,1,1,1,1,1,1,1,1,1,1,1,1,1,1,1,1,1,1,1,1,
1,1,1,1,1,1,1,1,1,1,1,1,1,1,6),(2,2),(-1.,-0.971428571428572,-0.942857142857143,
-0.914285714285714,-0.885714285714286,-0.857142857142857,-0.828571428571429,
-0.8,-0.771428571428572,-0.742857142857143,-0.714285714285714,-0.685714285714286,
-0.657142857142857,-0.628571428571429,-0.6,-0.571428571428572,-0.542857142857143,
-0.514285714285714,-0.485714285714286,-0.457142857142857,-0.428571428571429,
-0.4,-0.371428571428571,-0.342857142857143,-0.314285714285714,-0.285714285714286,
-0.257142857142857,-0.228571428571429,-0.2,-0.171428571428571,-0.142857142857143,
-0.114285714285714,-0.0857142857142857,-0.0571428571428571,-0.0285714285714286,
0.),(0.,2.9),.UNSPECIFIED.)
GEOMETRIC_REPRESENTATION_ITEM()
RATIONAL_B_SPLINE_SURFACE(((1.,1.),(1.,1.),(1.,1.),(1.,1.),(1.,1.),(1.,
1.),(1.,1.),(1.,1.),(1.,1.),(1.,1.),(1.,1.),(1.,1.),(1.,1.),(1.,1.),(1.,
1.),(1.,1.),(1.,1.),(1.,1.),(1.,1.),(1.,1.),(1.,1.),(1.,1.),(1.,1.),(1.,
1.),(1.,1.),(1.,1.),(1.,1.),(1.,1.),(1.,1.),(1.,1.),(1.,1.),(1.,1.),(1.,
1.),(1.,1.),(1.,1.),(1.,1.),(1.,1.),(1.,1.),(1.,1.),(1.,1.)))
REPRESENTATION_ITEM('')
SURFACE()
);
#540=(
BOUNDED_SURFACE()
B_SPLINE_SURFACE(5,1,((#55077,#55078),(#55079,#55080),(#55081,#55082),(#55083,
#55084),(#55085,#55086),(#55087,#55088),(#55089,#55090),(#55091,#55092),
(#55093,#55094),(#55095,#55096),(#55097,#55098),(#55099,#55100),(#55101,
#55102),(#55103,#55104),(#55105,#55106),(#55107,#55108),(#55109,#55110),
(#55111,#55112),(#55113,#55114),(#55115,#55116),(#55117,#55118),(#55119,
#55120),(#55121,#55122),(#55123,#55124),(#55125,#55126),(#55127,#55128),
(#55129,#55130),(#55131,#55132),(#55133,#55134),(#55135,#55136),(#55137,
#55138),(#55139,#55140),(#55141,#55142),(#55143,#55144),(#55145,#55146),
(#55147,#55148),(#55149,#55150),(#55151,#55152),(#55153,#55154),(#55155,
#55156)),.UNSPECIFIED.,.F.,.F.,.F.)
B_SPLINE_SURFACE_WITH_KNOTS((6,1,1,1,1,1,1,1,1,1,1,1,1,1,1,1,1,1,1,1,1,
1,1,1,1,1,1,1,1,1,1,1,1,1,1,6),(2,2),(-1.,-0.971428571428572,-0.942857142857143,
-0.914285714285714,-0.885714285714286,-0.857142857142857,-0.828571428571429,
-0.8,-0.771428571428572,-0.742857142857143,-0.714285714285714,-0.685714285714286,
-0.657142857142857,-0.628571428571429,-0.6,-0.571428571428572,-0.542857142857143,
-0.514285714285714,-0.485714285714286,-0.457142857142857,-0.428571428571429,
-0.4,-0.371428571428571,-0.342857142857143,-0.314285714285714,-0.285714285714286,
-0.257142857142857,-0.228571428571429,-0.2,-0.171428571428571,-0.142857142857143,
-0.114285714285714,-0.0857142857142857,-0.0571428571428571,-0.0285714285714286,
0.),(0.,2.9),.UNSPECIFIED.)
GEOMETRIC_REPRESENTATION_ITEM()
RATIONAL_B_SPLINE_SURFACE(((1.,1.),(1.,1.),(1.,1.),(1.,1.),(1.,1.),(1.,
1.),(1.,1.),(1.,1.),(1.,1.),(1.,1.),(1.,1.),(1.,1.),(1.,1.),(1.,1.),(1.,
1.),(1.,1.),(1.,1.),(1.,1.),(1.,1.),(1.,1.),(1.,1.),(1.,1.),(1.,1.),(1.,
1.),(1.,1.),(1.,1.),(1.,1.),(1.,1.),(1.,1.),(1.,1.),(1.,1.),(1.,1.),(1.,
1.),(1.,1.),(1.,1.),(1.,1.),(1.,1.),(1.,1.),(1.,1.),(1.,1.)))
REPRESENTATION_ITEM('')
SURFACE()
);
#541=(
BOUNDED_SURFACE()
B_SPLINE_SURFACE(5,1,((#55173,#55174),(#55175,#55176),(#55177,#55178),(#55179,
#55180),(#55181,#55182),(#55183,#55184),(#55185,#55186),(#55187,#55188),
(#55189,#55190),(#55191,#55192),(#55193,#55194),(#55195,#55196),(#55197,
#55198),(#55199,#55200),(#55201,#55202),(#55203,#55204),(#55205,#55206),
(#55207,#55208),(#55209,#55210),(#55211,#55212),(#55213,#55214),(#55215,
#55216),(#55217,#55218),(#55219,#55220),(#55221,#55222),(#55223,#55224),
(#55225,#55226),(#55227,#55228),(#55229,#55230),(#55231,#55232),(#55233,
#55234),(#55235,#55236),(#55237,#55238),(#55239,#55240),(#55241,#55242),
(#55243,#55244),(#55245,#55246),(#55247,#55248),(#55249,#55250),(#55251,
#55252)),.UNSPECIFIED.,.F.,.F.,.F.)
B_SPLINE_SURFACE_WITH_KNOTS((6,1,1,1,1,1,1,1,1,1,1,1,1,1,1,1,1,1,1,1,1,
1,1,1,1,1,1,1,1,1,1,1,1,1,1,6),(2,2),(-1.,-0.971428571428572,-0.942857142857143,
-0.914285714285714,-0.885714285714286,-0.857142857142857,-0.828571428571429,
-0.8,-0.771428571428572,-0.742857142857143,-0.714285714285714,-0.685714285714286,
-0.657142857142857,-0.628571428571429,-0.6,-0.571428571428572,-0.542857142857143,
-0.514285714285714,-0.485714285714286,-0.457142857142857,-0.428571428571429,
-0.4,-0.371428571428571,-0.342857142857143,-0.314285714285714,-0.285714285714286,
-0.257142857142857,-0.228571428571429,-0.2,-0.171428571428571,-0.142857142857143,
-0.114285714285714,-0.0857142857142857,-0.0571428571428571,-0.0285714285714286,
0.),(0.,2.9),.UNSPECIFIED.)
GEOMETRIC_REPRESENTATION_ITEM()
RATIONAL_B_SPLINE_SURFACE(((1.,1.),(1.,1.),(1.,1.),(1.,1.),(1.,1.),(1.,
1.),(1.,1.),(1.,1.),(1.,1.),(1.,1.),(1.,1.),(1.,1.),(1.,1.),(1.,1.),(1.,
1.),(1.,1.),(1.,1.),(1.,1.),(1.,1.),(1.,1.),(1.,1.),(1.,1.),(1.,1.),(1.,
1.),(1.,1.),(1.,1.),(1.,1.),(1.,1.),(1.,1.),(1.,1.),(1.,1.),(1.,1.),(1.,
1.),(1.,1.),(1.,1.),(1.,1.),(1.,1.),(1.,1.),(1.,1.),(1.,1.)))
REPRESENTATION_ITEM('')
SURFACE()
);
#542=(
BOUNDED_SURFACE()
B_SPLINE_SURFACE(5,1,((#55278,#55279),(#55280,#55281),(#55282,#55283),(#55284,
#55285),(#55286,#55287),(#55288,#55289),(#55290,#55291),(#55292,#55293),
(#55294,#55295),(#55296,#55297),(#55298,#55299),(#55300,#55301),(#55302,
#55303),(#55304,#55305),(#55306,#55307),(#55308,#55309),(#55310,#55311),
(#55312,#55313),(#55314,#55315),(#55316,#55317),(#55318,#55319),(#55320,
#55321),(#55322,#55323),(#55324,#55325),(#55326,#55327),(#55328,#55329),
(#55330,#55331),(#55332,#55333),(#55334,#55335),(#55336,#55337),(#55338,
#55339),(#55340,#55341),(#55342,#55343),(#55344,#55345),(#55346,#55347),
(#55348,#55349),(#55350,#55351),(#55352,#55353),(#55354,#55355),(#55356,
#55357)),.UNSPECIFIED.,.F.,.F.,.F.)
B_SPLINE_SURFACE_WITH_KNOTS((6,1,1,1,1,1,1,1,1,1,1,1,1,1,1,1,1,1,1,1,1,
1,1,1,1,1,1,1,1,1,1,1,1,1,1,6),(2,2),(-1.,-0.971428571428572,-0.942857142857143,
-0.914285714285714,-0.885714285714286,-0.857142857142857,-0.828571428571429,
-0.8,-0.771428571428572,-0.742857142857143,-0.714285714285714,-0.685714285714286,
-0.657142857142857,-0.628571428571429,-0.6,-0.571428571428572,-0.542857142857143,
-0.514285714285714,-0.485714285714286,-0.457142857142857,-0.428571428571429,
-0.4,-0.371428571428571,-0.342857142857143,-0.314285714285714,-0.285714285714286,
-0.257142857142857,-0.228571428571429,-0.2,-0.171428571428571,-0.142857142857143,
-0.114285714285714,-0.0857142857142857,-0.0571428571428571,-0.0285714285714286,
0.),(0.,2.9),.UNSPECIFIED.)
GEOMETRIC_REPRESENTATION_ITEM()
RATIONAL_B_SPLINE_SURFACE(((1.,1.),(1.,1.),(1.,1.),(1.,1.),(1.,1.),(1.,
1.),(1.,1.),(1.,1.),(1.,1.),(1.,1.),(1.,1.),(1.,1.),(1.,1.),(1.,1.),(1.,
1.),(1.,1.),(1.,1.),(1.,1.),(1.,1.),(1.,1.),(1.,1.),(1.,1.),(1.,1.),(1.,
1.),(1.,1.),(1.,1.),(1.,1.),(1.,1.),(1.,1.),(1.,1.),(1.,1.),(1.,1.),(1.,
1.),(1.,1.),(1.,1.),(1.,1.),(1.,1.),(1.,1.),(1.,1.),(1.,1.)))
REPRESENTATION_ITEM('')
SURFACE()
);
#543=(
BOUNDED_SURFACE()
B_SPLINE_SURFACE(5,1,((#55361,#55362),(#55363,#55364),(#55365,#55366),(#55367,
#55368),(#55369,#55370),(#55371,#55372),(#55373,#55374),(#55375,#55376),
(#55377,#55378),(#55379,#55380),(#55381,#55382),(#55383,#55384),(#55385,
#55386),(#55387,#55388),(#55389,#55390),(#55391,#55392),(#55393,#55394),
(#55395,#55396),(#55397,#55398),(#55399,#55400),(#55401,#55402),(#55403,
#55404),(#55405,#55406),(#55407,#55408),(#55409,#55410),(#55411,#55412),
(#55413,#55414),(#55415,#55416),(#55417,#55418),(#55419,#55420),(#55421,
#55422),(#55423,#55424),(#55425,#55426),(#55427,#55428),(#55429,#55430),
(#55431,#55432),(#55433,#55434),(#55435,#55436),(#55437,#55438),(#55439,
#55440)),.UNSPECIFIED.,.F.,.F.,.F.)
B_SPLINE_SURFACE_WITH_KNOTS((6,1,1,1,1,1,1,1,1,1,1,1,1,1,1,1,1,1,1,1,1,
1,1,1,1,1,1,1,1,1,1,1,1,1,1,6),(2,2),(-1.,-0.971428571428572,-0.942857142857143,
-0.914285714285714,-0.885714285714286,-0.857142857142857,-0.828571428571429,
-0.8,-0.771428571428572,-0.742857142857143,-0.714285714285714,-0.685714285714286,
-0.657142857142857,-0.628571428571429,-0.6,-0.571428571428572,-0.542857142857143,
-0.514285714285714,-0.485714285714286,-0.457142857142857,-0.428571428571429,
-0.4,-0.371428571428571,-0.342857142857143,-0.314285714285714,-0.285714285714286,
-0.257142857142857,-0.228571428571429,-0.2,-0.171428571428571,-0.142857142857143,
-0.114285714285714,-0.0857142857142857,-0.0571428571428571,-0.0285714285714286,
0.),(0.,2.9),.UNSPECIFIED.)
GEOMETRIC_REPRESENTATION_ITEM()
RATIONAL_B_SPLINE_SURFACE(((1.,1.),(1.,1.),(1.,1.),(1.,1.),(1.,1.),(1.,
1.),(1.,1.),(1.,1.),(1.,1.),(1.,1.),(1.,1.),(1.,1.),(1.,1.),(1.,1.),(1.,
1.),(1.,1.),(1.,1.),(1.,1.),(1.,1.),(1.,1.),(1.,1.),(1.,1.),(1.,1.),(1.,
1.),(1.,1.),(1.,1.),(1.,1.),(1.,1.),(1.,1.),(1.,1.),(1.,1.),(1.,1.),(1.,
1.),(1.,1.),(1.,1.),(1.,1.),(1.,1.),(1.,1.),(1.,1.),(1.,1.)))
REPRESENTATION_ITEM('')
SURFACE()
);
#544=(
BOUNDED_SURFACE()
B_SPLINE_SURFACE(5,1,((#55457,#55458),(#55459,#55460),(#55461,#55462),(#55463,
#55464),(#55465,#55466),(#55467,#55468),(#55469,#55470),(#55471,#55472),
(#55473,#55474),(#55475,#55476),(#55477,#55478),(#55479,#55480),(#55481,
#55482),(#55483,#55484),(#55485,#55486),(#55487,#55488),(#55489,#55490),
(#55491,#55492),(#55493,#55494),(#55495,#55496),(#55497,#55498),(#55499,
#55500),(#55501,#55502),(#55503,#55504),(#55505,#55506),(#55507,#55508),
(#55509,#55510),(#55511,#55512),(#55513,#55514),(#55515,#55516),(#55517,
#55518),(#55519,#55520),(#55521,#55522),(#55523,#55524),(#55525,#55526),
(#55527,#55528),(#55529,#55530),(#55531,#55532),(#55533,#55534),(#55535,
#55536)),.UNSPECIFIED.,.F.,.F.,.F.)
B_SPLINE_SURFACE_WITH_KNOTS((6,1,1,1,1,1,1,1,1,1,1,1,1,1,1,1,1,1,1,1,1,
1,1,1,1,1,1,1,1,1,1,1,1,1,1,6),(2,2),(-1.,-0.971428571428572,-0.942857142857143,
-0.914285714285714,-0.885714285714286,-0.857142857142857,-0.828571428571429,
-0.8,-0.771428571428572,-0.742857142857143,-0.714285714285714,-0.685714285714286,
-0.657142857142857,-0.628571428571429,-0.6,-0.571428571428572,-0.542857142857143,
-0.514285714285714,-0.485714285714286,-0.457142857142857,-0.428571428571429,
-0.4,-0.371428571428571,-0.342857142857143,-0.314285714285714,-0.285714285714286,
-0.257142857142857,-0.228571428571429,-0.2,-0.171428571428571,-0.142857142857143,
-0.114285714285714,-0.0857142857142857,-0.0571428571428571,-0.0285714285714286,
0.),(0.,2.9),.UNSPECIFIED.)
GEOMETRIC_REPRESENTATION_ITEM()
RATIONAL_B_SPLINE_SURFACE(((1.,1.),(1.,1.),(1.,1.),(1.,1.),(1.,1.),(1.,
1.),(1.,1.),(1.,1.),(1.,1.),(1.,1.),(1.,1.),(1.,1.),(1.,1.),(1.,1.),(1.,
1.),(1.,1.),(1.,1.),(1.,1.),(1.,1.),(1.,1.),(1.,1.),(1.,1.),(1.,1.),(1.,
1.),(1.,1.),(1.,1.),(1.,1.),(1.,1.),(1.,1.),(1.,1.),(1.,1.),(1.,1.),(1.,
1.),(1.,1.),(1.,1.),(1.,1.),(1.,1.),(1.,1.),(1.,1.),(1.,1.)))
REPRESENTATION_ITEM('')
SURFACE()
);
#545=(
BOUNDED_SURFACE()
B_SPLINE_SURFACE(5,1,((#55553,#55554),(#55555,#55556),(#55557,#55558),(#55559,
#55560),(#55561,#55562),(#55563,#55564),(#55565,#55566),(#55567,#55568),
(#55569,#55570),(#55571,#55572),(#55573,#55574),(#55575,#55576),(#55577,
#55578),(#55579,#55580),(#55581,#55582),(#55583,#55584),(#55585,#55586),
(#55587,#55588),(#55589,#55590),(#55591,#55592),(#55593,#55594),(#55595,
#55596),(#55597,#55598),(#55599,#55600),(#55601,#55602),(#55603,#55604),
(#55605,#55606),(#55607,#55608),(#55609,#55610),(#55611,#55612),(#55613,
#55614),(#55615,#55616),(#55617,#55618),(#55619,#55620),(#55621,#55622),
(#55623,#55624),(#55625,#55626),(#55627,#55628),(#55629,#55630),(#55631,
#55632)),.UNSPECIFIED.,.F.,.F.,.F.)
B_SPLINE_SURFACE_WITH_KNOTS((6,1,1,1,1,1,1,1,1,1,1,1,1,1,1,1,1,1,1,1,1,
1,1,1,1,1,1,1,1,1,1,1,1,1,1,6),(2,2),(-1.,-0.971428571428572,-0.942857142857143,
-0.914285714285714,-0.885714285714286,-0.857142857142857,-0.828571428571429,
-0.8,-0.771428571428572,-0.742857142857143,-0.714285714285714,-0.685714285714286,
-0.657142857142857,-0.628571428571429,-0.6,-0.571428571428572,-0.542857142857143,
-0.514285714285714,-0.485714285714286,-0.457142857142857,-0.428571428571429,
-0.4,-0.371428571428571,-0.342857142857143,-0.314285714285714,-0.285714285714286,
-0.257142857142857,-0.228571428571429,-0.2,-0.171428571428571,-0.142857142857143,
-0.114285714285714,-0.0857142857142857,-0.0571428571428571,-0.0285714285714286,
0.),(0.,2.9),.UNSPECIFIED.)
GEOMETRIC_REPRESENTATION_ITEM()
RATIONAL_B_SPLINE_SURFACE(((1.,1.),(1.,1.),(1.,1.),(1.,1.),(1.,1.),(1.,
1.),(1.,1.),(1.,1.),(1.,1.),(1.,1.),(1.,1.),(1.,1.),(1.,1.),(1.,1.),(1.,
1.),(1.,1.),(1.,1.),(1.,1.),(1.,1.),(1.,1.),(1.,1.),(1.,1.),(1.,1.),(1.,
1.),(1.,1.),(1.,1.),(1.,1.),(1.,1.),(1.,1.),(1.,1.),(1.,1.),(1.,1.),(1.,
1.),(1.,1.),(1.,1.),(1.,1.),(1.,1.),(1.,1.),(1.,1.),(1.,1.)))
REPRESENTATION_ITEM('')
SURFACE()
);
#546=(
BOUNDED_SURFACE()
B_SPLINE_SURFACE(5,1,((#55661,#55662),(#55663,#55664),(#55665,#55666),(#55667,
#55668),(#55669,#55670),(#55671,#55672),(#55673,#55674),(#55675,#55676),
(#55677,#55678),(#55679,#55680),(#55681,#55682),(#55683,#55684),(#55685,
#55686),(#55687,#55688),(#55689,#55690),(#55691,#55692),(#55693,#55694),
(#55695,#55696),(#55697,#55698),(#55699,#55700),(#55701,#55702),(#55703,
#55704),(#55705,#55706),(#55707,#55708),(#55709,#55710),(#55711,#55712),
(#55713,#55714),(#55715,#55716),(#55717,#55718),(#55719,#55720),(#55721,
#55722),(#55723,#55724),(#55725,#55726),(#55727,#55728),(#55729,#55730),
(#55731,#55732),(#55733,#55734),(#55735,#55736),(#55737,#55738),(#55739,
#55740)),.UNSPECIFIED.,.F.,.F.,.F.)
B_SPLINE_SURFACE_WITH_KNOTS((6,1,1,1,1,1,1,1,1,1,1,1,1,1,1,1,1,1,1,1,1,
1,1,1,1,1,1,1,1,1,1,1,1,1,1,6),(2,2),(-1.,-0.971428571428572,-0.942857142857143,
-0.914285714285714,-0.885714285714286,-0.857142857142857,-0.828571428571429,
-0.8,-0.771428571428572,-0.742857142857143,-0.714285714285714,-0.685714285714286,
-0.657142857142857,-0.628571428571429,-0.6,-0.571428571428572,-0.542857142857143,
-0.514285714285714,-0.485714285714286,-0.457142857142857,-0.428571428571429,
-0.4,-0.371428571428571,-0.342857142857143,-0.314285714285714,-0.285714285714286,
-0.257142857142857,-0.228571428571429,-0.2,-0.171428571428571,-0.142857142857143,
-0.114285714285714,-0.0857142857142857,-0.0571428571428571,-0.0285714285714286,
0.),(0.,2.9),.UNSPECIFIED.)
GEOMETRIC_REPRESENTATION_ITEM()
RATIONAL_B_SPLINE_SURFACE(((1.,1.),(1.,1.),(1.,1.),(1.,1.),(1.,1.),(1.,
1.),(1.,1.),(1.,1.),(1.,1.),(1.,1.),(1.,1.),(1.,1.),(1.,1.),(1.,1.),(1.,
1.),(1.,1.),(1.,1.),(1.,1.),(1.,1.),(1.,1.),(1.,1.),(1.,1.),(1.,1.),(1.,
1.),(1.,1.),(1.,1.),(1.,1.),(1.,1.),(1.,1.),(1.,1.),(1.,1.),(1.,1.),(1.,
1.),(1.,1.),(1.,1.),(1.,1.),(1.,1.),(1.,1.),(1.,1.),(1.,1.)))
REPRESENTATION_ITEM('')
SURFACE()
);
#547=(
BOUNDED_SURFACE()
B_SPLINE_SURFACE(5,1,((#55744,#55745),(#55746,#55747),(#55748,#55749),(#55750,
#55751),(#55752,#55753),(#55754,#55755),(#55756,#55757),(#55758,#55759),
(#55760,#55761),(#55762,#55763),(#55764,#55765),(#55766,#55767),(#55768,
#55769),(#55770,#55771),(#55772,#55773),(#55774,#55775),(#55776,#55777),
(#55778,#55779),(#55780,#55781),(#55782,#55783),(#55784,#55785),(#55786,
#55787),(#55788,#55789),(#55790,#55791),(#55792,#55793),(#55794,#55795),
(#55796,#55797),(#55798,#55799),(#55800,#55801),(#55802,#55803),(#55804,
#55805),(#55806,#55807),(#55808,#55809),(#55810,#55811),(#55812,#55813),
(#55814,#55815),(#55816,#55817),(#55818,#55819),(#55820,#55821),(#55822,
#55823)),.UNSPECIFIED.,.F.,.F.,.F.)
B_SPLINE_SURFACE_WITH_KNOTS((6,1,1,1,1,1,1,1,1,1,1,1,1,1,1,1,1,1,1,1,1,
1,1,1,1,1,1,1,1,1,1,1,1,1,1,6),(2,2),(-1.,-0.971428571428572,-0.942857142857143,
-0.914285714285714,-0.885714285714286,-0.857142857142857,-0.828571428571429,
-0.8,-0.771428571428572,-0.742857142857143,-0.714285714285714,-0.685714285714286,
-0.657142857142857,-0.628571428571429,-0.6,-0.571428571428572,-0.542857142857143,
-0.514285714285714,-0.485714285714286,-0.457142857142857,-0.428571428571429,
-0.4,-0.371428571428571,-0.342857142857143,-0.314285714285714,-0.285714285714286,
-0.257142857142857,-0.228571428571429,-0.2,-0.171428571428571,-0.142857142857143,
-0.114285714285714,-0.0857142857142857,-0.0571428571428571,-0.0285714285714286,
0.),(0.,2.9),.UNSPECIFIED.)
GEOMETRIC_REPRESENTATION_ITEM()
RATIONAL_B_SPLINE_SURFACE(((1.,1.),(1.,1.),(1.,1.),(1.,1.),(1.,1.),(1.,
1.),(1.,1.),(1.,1.),(1.,1.),(1.,1.),(1.,1.),(1.,1.),(1.,1.),(1.,1.),(1.,
1.),(1.,1.),(1.,1.),(1.,1.),(1.,1.),(1.,1.),(1.,1.),(1.,1.),(1.,1.),(1.,
1.),(1.,1.),(1.,1.),(1.,1.),(1.,1.),(1.,1.),(1.,1.),(1.,1.),(1.,1.),(1.,
1.),(1.,1.),(1.,1.),(1.,1.),(1.,1.),(1.,1.),(1.,1.),(1.,1.)))
REPRESENTATION_ITEM('')
SURFACE()
);
#548=(
BOUNDED_SURFACE()
B_SPLINE_SURFACE(5,1,((#55840,#55841),(#55842,#55843),(#55844,#55845),(#55846,
#55847),(#55848,#55849),(#55850,#55851),(#55852,#55853),(#55854,#55855),
(#55856,#55857),(#55858,#55859),(#55860,#55861),(#55862,#55863),(#55864,
#55865),(#55866,#55867),(#55868,#55869),(#55870,#55871),(#55872,#55873),
(#55874,#55875),(#55876,#55877),(#55878,#55879),(#55880,#55881),(#55882,
#55883),(#55884,#55885),(#55886,#55887),(#55888,#55889),(#55890,#55891),
(#55892,#55893),(#55894,#55895),(#55896,#55897),(#55898,#55899),(#55900,
#55901),(#55902,#55903),(#55904,#55905),(#55906,#55907),(#55908,#55909),
(#55910,#55911),(#55912,#55913),(#55914,#55915),(#55916,#55917),(#55918,
#55919)),.UNSPECIFIED.,.F.,.F.,.F.)
B_SPLINE_SURFACE_WITH_KNOTS((6,1,1,1,1,1,1,1,1,1,1,1,1,1,1,1,1,1,1,1,1,
1,1,1,1,1,1,1,1,1,1,1,1,1,1,6),(2,2),(-1.,-0.971428571428572,-0.942857142857143,
-0.914285714285714,-0.885714285714286,-0.857142857142857,-0.828571428571429,
-0.8,-0.771428571428572,-0.742857142857143,-0.714285714285714,-0.685714285714286,
-0.657142857142857,-0.628571428571429,-0.6,-0.571428571428572,-0.542857142857143,
-0.514285714285714,-0.485714285714286,-0.457142857142857,-0.428571428571429,
-0.4,-0.371428571428571,-0.342857142857143,-0.314285714285714,-0.285714285714286,
-0.257142857142857,-0.228571428571429,-0.2,-0.171428571428571,-0.142857142857143,
-0.114285714285714,-0.0857142857142857,-0.0571428571428571,-0.0285714285714286,
0.),(0.,2.9),.UNSPECIFIED.)
GEOMETRIC_REPRESENTATION_ITEM()
RATIONAL_B_SPLINE_SURFACE(((1.,1.),(1.,1.),(1.,1.),(1.,1.),(1.,1.),(1.,
1.),(1.,1.),(1.,1.),(1.,1.),(1.,1.),(1.,1.),(1.,1.),(1.,1.),(1.,1.),(1.,
1.),(1.,1.),(1.,1.),(1.,1.),(1.,1.),(1.,1.),(1.,1.),(1.,1.),(1.,1.),(1.,
1.),(1.,1.),(1.,1.),(1.,1.),(1.,1.),(1.,1.),(1.,1.),(1.,1.),(1.,1.),(1.,
1.),(1.,1.),(1.,1.),(1.,1.),(1.,1.),(1.,1.),(1.,1.),(1.,1.)))
REPRESENTATION_ITEM('')
SURFACE()
);
#549=(
BOUNDED_SURFACE()
B_SPLINE_SURFACE(5,1,((#55936,#55937),(#55938,#55939),(#55940,#55941),(#55942,
#55943),(#55944,#55945),(#55946,#55947),(#55948,#55949),(#55950,#55951),
(#55952,#55953),(#55954,#55955),(#55956,#55957),(#55958,#55959),(#55960,
#55961),(#55962,#55963),(#55964,#55965),(#55966,#55967),(#55968,#55969),
(#55970,#55971),(#55972,#55973),(#55974,#55975),(#55976,#55977),(#55978,
#55979),(#55980,#55981),(#55982,#55983),(#55984,#55985),(#55986,#55987),
(#55988,#55989),(#55990,#55991),(#55992,#55993),(#55994,#55995),(#55996,
#55997),(#55998,#55999),(#56000,#56001),(#56002,#56003),(#56004,#56005),
(#56006,#56007),(#56008,#56009),(#56010,#56011),(#56012,#56013),(#56014,
#56015)),.UNSPECIFIED.,.F.,.F.,.F.)
B_SPLINE_SURFACE_WITH_KNOTS((6,1,1,1,1,1,1,1,1,1,1,1,1,1,1,1,1,1,1,1,1,
1,1,1,1,1,1,1,1,1,1,1,1,1,1,6),(2,2),(-1.,-0.971428571428572,-0.942857142857143,
-0.914285714285714,-0.885714285714286,-0.857142857142857,-0.828571428571429,
-0.8,-0.771428571428572,-0.742857142857143,-0.714285714285714,-0.685714285714286,
-0.657142857142857,-0.628571428571429,-0.6,-0.571428571428572,-0.542857142857143,
-0.514285714285714,-0.485714285714286,-0.457142857142857,-0.428571428571429,
-0.4,-0.371428571428571,-0.342857142857143,-0.314285714285714,-0.285714285714286,
-0.257142857142857,-0.228571428571429,-0.2,-0.171428571428571,-0.142857142857143,
-0.114285714285714,-0.0857142857142857,-0.0571428571428571,-0.0285714285714286,
0.),(0.,2.9),.UNSPECIFIED.)
GEOMETRIC_REPRESENTATION_ITEM()
RATIONAL_B_SPLINE_SURFACE(((1.,1.),(1.,1.),(1.,1.),(1.,1.),(1.,1.),(1.,
1.),(1.,1.),(1.,1.),(1.,1.),(1.,1.),(1.,1.),(1.,1.),(1.,1.),(1.,1.),(1.,
1.),(1.,1.),(1.,1.),(1.,1.),(1.,1.),(1.,1.),(1.,1.),(1.,1.),(1.,1.),(1.,
1.),(1.,1.),(1.,1.),(1.,1.),(1.,1.),(1.,1.),(1.,1.),(1.,1.),(1.,1.),(1.,
1.),(1.,1.),(1.,1.),(1.,1.),(1.,1.),(1.,1.),(1.,1.),(1.,1.)))
REPRESENTATION_ITEM('')
SURFACE()
);
#550=(
BOUNDED_SURFACE()
B_SPLINE_SURFACE(5,1,((#56041,#56042),(#56043,#56044),(#56045,#56046),(#56047,
#56048),(#56049,#56050),(#56051,#56052),(#56053,#56054),(#56055,#56056),
(#56057,#56058),(#56059,#56060),(#56061,#56062),(#56063,#56064),(#56065,
#56066),(#56067,#56068),(#56069,#56070),(#56071,#56072),(#56073,#56074),
(#56075,#56076),(#56077,#56078),(#56079,#56080),(#56081,#56082),(#56083,
#56084),(#56085,#56086),(#56087,#56088),(#56089,#56090),(#56091,#56092),
(#56093,#56094),(#56095,#56096),(#56097,#56098),(#56099,#56100),(#56101,
#56102),(#56103,#56104),(#56105,#56106),(#56107,#56108),(#56109,#56110),
(#56111,#56112),(#56113,#56114),(#56115,#56116),(#56117,#56118),(#56119,
#56120)),.UNSPECIFIED.,.F.,.F.,.F.)
B_SPLINE_SURFACE_WITH_KNOTS((6,1,1,1,1,1,1,1,1,1,1,1,1,1,1,1,1,1,1,1,1,
1,1,1,1,1,1,1,1,1,1,1,1,1,1,6),(2,2),(-1.,-0.971428571428572,-0.942857142857143,
-0.914285714285714,-0.885714285714286,-0.857142857142857,-0.828571428571429,
-0.8,-0.771428571428572,-0.742857142857143,-0.714285714285714,-0.685714285714286,
-0.657142857142857,-0.628571428571429,-0.6,-0.571428571428572,-0.542857142857143,
-0.514285714285714,-0.485714285714286,-0.457142857142857,-0.428571428571429,
-0.4,-0.371428571428571,-0.342857142857143,-0.314285714285714,-0.285714285714286,
-0.257142857142857,-0.228571428571429,-0.2,-0.171428571428571,-0.142857142857143,
-0.114285714285714,-0.0857142857142857,-0.0571428571428571,-0.0285714285714286,
0.),(0.,2.9),.UNSPECIFIED.)
GEOMETRIC_REPRESENTATION_ITEM()
RATIONAL_B_SPLINE_SURFACE(((1.,1.),(1.,1.),(1.,1.),(1.,1.),(1.,1.),(1.,
1.),(1.,1.),(1.,1.),(1.,1.),(1.,1.),(1.,1.),(1.,1.),(1.,1.),(1.,1.),(1.,
1.),(1.,1.),(1.,1.),(1.,1.),(1.,1.),(1.,1.),(1.,1.),(1.,1.),(1.,1.),(1.,
1.),(1.,1.),(1.,1.),(1.,1.),(1.,1.),(1.,1.),(1.,1.),(1.,1.),(1.,1.),(1.,
1.),(1.,1.),(1.,1.),(1.,1.),(1.,1.),(1.,1.),(1.,1.),(1.,1.)))
REPRESENTATION_ITEM('')
SURFACE()
);
#551=(
BOUNDED_SURFACE()
B_SPLINE_SURFACE(5,1,((#56124,#56125),(#56126,#56127),(#56128,#56129),(#56130,
#56131),(#56132,#56133),(#56134,#56135),(#56136,#56137),(#56138,#56139),
(#56140,#56141),(#56142,#56143),(#56144,#56145),(#56146,#56147),(#56148,
#56149),(#56150,#56151),(#56152,#56153),(#56154,#56155),(#56156,#56157),
(#56158,#56159),(#56160,#56161),(#56162,#56163),(#56164,#56165),(#56166,
#56167),(#56168,#56169),(#56170,#56171),(#56172,#56173),(#56174,#56175),
(#56176,#56177),(#56178,#56179),(#56180,#56181),(#56182,#56183),(#56184,
#56185),(#56186,#56187),(#56188,#56189),(#56190,#56191),(#56192,#56193),
(#56194,#56195),(#56196,#56197),(#56198,#56199),(#56200,#56201),(#56202,
#56203)),.UNSPECIFIED.,.F.,.F.,.F.)
B_SPLINE_SURFACE_WITH_KNOTS((6,1,1,1,1,1,1,1,1,1,1,1,1,1,1,1,1,1,1,1,1,
1,1,1,1,1,1,1,1,1,1,1,1,1,1,6),(2,2),(-1.,-0.971428571428572,-0.942857142857143,
-0.914285714285714,-0.885714285714286,-0.857142857142857,-0.828571428571429,
-0.8,-0.771428571428572,-0.742857142857143,-0.714285714285714,-0.685714285714286,
-0.657142857142857,-0.628571428571429,-0.6,-0.571428571428572,-0.542857142857143,
-0.514285714285714,-0.485714285714286,-0.457142857142857,-0.428571428571429,
-0.4,-0.371428571428571,-0.342857142857143,-0.314285714285714,-0.285714285714286,
-0.257142857142857,-0.228571428571429,-0.2,-0.171428571428571,-0.142857142857143,
-0.114285714285714,-0.0857142857142857,-0.0571428571428571,-0.0285714285714286,
0.),(0.,2.9),.UNSPECIFIED.)
GEOMETRIC_REPRESENTATION_ITEM()
RATIONAL_B_SPLINE_SURFACE(((1.,1.),(1.,1.),(1.,1.),(1.,1.),(1.,1.),(1.,
1.),(1.,1.),(1.,1.),(1.,1.),(1.,1.),(1.,1.),(1.,1.),(1.,1.),(1.,1.),(1.,
1.),(1.,1.),(1.,1.),(1.,1.),(1.,1.),(1.,1.),(1.,1.),(1.,1.),(1.,1.),(1.,
1.),(1.,1.),(1.,1.),(1.,1.),(1.,1.),(1.,1.),(1.,1.),(1.,1.),(1.,1.),(1.,
1.),(1.,1.),(1.,1.),(1.,1.),(1.,1.),(1.,1.),(1.,1.),(1.,1.)))
REPRESENTATION_ITEM('')
SURFACE()
);
#552=(
BOUNDED_SURFACE()
B_SPLINE_SURFACE(5,1,((#56220,#56221),(#56222,#56223),(#56224,#56225),(#56226,
#56227),(#56228,#56229),(#56230,#56231),(#56232,#56233),(#56234,#56235),
(#56236,#56237),(#56238,#56239),(#56240,#56241),(#56242,#56243),(#56244,
#56245),(#56246,#56247),(#56248,#56249),(#56250,#56251),(#56252,#56253),
(#56254,#56255),(#56256,#56257),(#56258,#56259),(#56260,#56261),(#56262,
#56263),(#56264,#56265),(#56266,#56267),(#56268,#56269),(#56270,#56271),
(#56272,#56273),(#56274,#56275),(#56276,#56277),(#56278,#56279),(#56280,
#56281),(#56282,#56283),(#56284,#56285),(#56286,#56287),(#56288,#56289),
(#56290,#56291),(#56292,#56293),(#56294,#56295),(#56296,#56297),(#56298,
#56299)),.UNSPECIFIED.,.F.,.F.,.F.)
B_SPLINE_SURFACE_WITH_KNOTS((6,1,1,1,1,1,1,1,1,1,1,1,1,1,1,1,1,1,1,1,1,
1,1,1,1,1,1,1,1,1,1,1,1,1,1,6),(2,2),(-1.,-0.971428571428572,-0.942857142857143,
-0.914285714285714,-0.885714285714286,-0.857142857142857,-0.828571428571429,
-0.8,-0.771428571428572,-0.742857142857143,-0.714285714285714,-0.685714285714286,
-0.657142857142857,-0.628571428571429,-0.6,-0.571428571428572,-0.542857142857143,
-0.514285714285714,-0.485714285714286,-0.457142857142857,-0.428571428571429,
-0.4,-0.371428571428571,-0.342857142857143,-0.314285714285714,-0.285714285714286,
-0.257142857142857,-0.228571428571429,-0.2,-0.171428571428571,-0.142857142857143,
-0.114285714285714,-0.0857142857142857,-0.0571428571428571,-0.0285714285714286,
0.),(0.,2.9),.UNSPECIFIED.)
GEOMETRIC_REPRESENTATION_ITEM()
RATIONAL_B_SPLINE_SURFACE(((1.,1.),(1.,1.),(1.,1.),(1.,1.),(1.,1.),(1.,
1.),(1.,1.),(1.,1.),(1.,1.),(1.,1.),(1.,1.),(1.,1.),(1.,1.),(1.,1.),(1.,
1.),(1.,1.),(1.,1.),(1.,1.),(1.,1.),(1.,1.),(1.,1.),(1.,1.),(1.,1.),(1.,
1.),(1.,1.),(1.,1.),(1.,1.),(1.,1.),(1.,1.),(1.,1.),(1.,1.),(1.,1.),(1.,
1.),(1.,1.),(1.,1.),(1.,1.),(1.,1.),(1.,1.),(1.,1.),(1.,1.)))
REPRESENTATION_ITEM('')
SURFACE()
);
#553=(
BOUNDED_SURFACE()
B_SPLINE_SURFACE(5,1,((#56316,#56317),(#56318,#56319),(#56320,#56321),(#56322,
#56323),(#56324,#56325),(#56326,#56327),(#56328,#56329),(#56330,#56331),
(#56332,#56333),(#56334,#56335),(#56336,#56337),(#56338,#56339),(#56340,
#56341),(#56342,#56343),(#56344,#56345),(#56346,#56347),(#56348,#56349),
(#56350,#56351),(#56352,#56353),(#56354,#56355),(#56356,#56357),(#56358,
#56359),(#56360,#56361),(#56362,#56363),(#56364,#56365),(#56366,#56367),
(#56368,#56369),(#56370,#56371),(#56372,#56373),(#56374,#56375),(#56376,
#56377),(#56378,#56379),(#56380,#56381),(#56382,#56383),(#56384,#56385),
(#56386,#56387),(#56388,#56389),(#56390,#56391),(#56392,#56393),(#56394,
#56395)),.UNSPECIFIED.,.F.,.F.,.F.)
B_SPLINE_SURFACE_WITH_KNOTS((6,1,1,1,1,1,1,1,1,1,1,1,1,1,1,1,1,1,1,1,1,
1,1,1,1,1,1,1,1,1,1,1,1,1,1,6),(2,2),(-1.,-0.971428571428572,-0.942857142857143,
-0.914285714285714,-0.885714285714286,-0.857142857142857,-0.828571428571429,
-0.8,-0.771428571428572,-0.742857142857143,-0.714285714285714,-0.685714285714286,
-0.657142857142857,-0.628571428571429,-0.6,-0.571428571428572,-0.542857142857143,
-0.514285714285714,-0.485714285714286,-0.457142857142857,-0.428571428571429,
-0.4,-0.371428571428571,-0.342857142857143,-0.314285714285714,-0.285714285714286,
-0.257142857142857,-0.228571428571429,-0.2,-0.171428571428571,-0.142857142857143,
-0.114285714285714,-0.0857142857142857,-0.0571428571428571,-0.0285714285714286,
0.),(0.,2.9),.UNSPECIFIED.)
GEOMETRIC_REPRESENTATION_ITEM()
RATIONAL_B_SPLINE_SURFACE(((1.,1.),(1.,1.),(1.,1.),(1.,1.),(1.,1.),(1.,
1.),(1.,1.),(1.,1.),(1.,1.),(1.,1.),(1.,1.),(1.,1.),(1.,1.),(1.,1.),(1.,
1.),(1.,1.),(1.,1.),(1.,1.),(1.,1.),(1.,1.),(1.,1.),(1.,1.),(1.,1.),(1.,
1.),(1.,1.),(1.,1.),(1.,1.),(1.,1.),(1.,1.),(1.,1.),(1.,1.),(1.,1.),(1.,
1.),(1.,1.),(1.,1.),(1.,1.),(1.,1.),(1.,1.),(1.,1.),(1.,1.)))
REPRESENTATION_ITEM('')
SURFACE()
);
#554=(
BOUNDED_SURFACE()
B_SPLINE_SURFACE(5,1,((#56427,#56428),(#56429,#56430),(#56431,#56432),(#56433,
#56434),(#56435,#56436),(#56437,#56438),(#56439,#56440),(#56441,#56442),
(#56443,#56444),(#56445,#56446),(#56447,#56448),(#56449,#56450),(#56451,
#56452),(#56453,#56454),(#56455,#56456),(#56457,#56458),(#56459,#56460),
(#56461,#56462),(#56463,#56464),(#56465,#56466),(#56467,#56468),(#56469,
#56470),(#56471,#56472),(#56473,#56474),(#56475,#56476),(#56477,#56478),
(#56479,#56480),(#56481,#56482),(#56483,#56484),(#56485,#56486),(#56487,
#56488),(#56489,#56490),(#56491,#56492),(#56493,#56494),(#56495,#56496),
(#56497,#56498),(#56499,#56500),(#56501,#56502),(#56503,#56504),(#56505,
#56506)),.UNSPECIFIED.,.F.,.F.,.F.)
B_SPLINE_SURFACE_WITH_KNOTS((6,1,1,1,1,1,1,1,1,1,1,1,1,1,1,1,1,1,1,1,1,
1,1,1,1,1,1,1,1,1,1,1,1,1,1,6),(2,2),(-1.,-0.971428571428572,-0.942857142857143,
-0.914285714285714,-0.885714285714286,-0.857142857142857,-0.828571428571429,
-0.8,-0.771428571428572,-0.742857142857143,-0.714285714285714,-0.685714285714286,
-0.657142857142857,-0.628571428571429,-0.6,-0.571428571428572,-0.542857142857143,
-0.514285714285714,-0.485714285714286,-0.457142857142857,-0.428571428571429,
-0.4,-0.371428571428571,-0.342857142857143,-0.314285714285714,-0.285714285714286,
-0.257142857142857,-0.228571428571429,-0.2,-0.171428571428571,-0.142857142857143,
-0.114285714285714,-0.0857142857142857,-0.0571428571428571,-0.0285714285714286,
0.),(0.,2.9),.UNSPECIFIED.)
GEOMETRIC_REPRESENTATION_ITEM()
RATIONAL_B_SPLINE_SURFACE(((1.,1.),(1.,1.),(1.,1.),(1.,1.),(1.,1.),(1.,
1.),(1.,1.),(1.,1.),(1.,1.),(1.,1.),(1.,1.),(1.,1.),(1.,1.),(1.,1.),(1.,
1.),(1.,1.),(1.,1.),(1.,1.),(1.,1.),(1.,1.),(1.,1.),(1.,1.),(1.,1.),(1.,
1.),(1.,1.),(1.,1.),(1.,1.),(1.,1.),(1.,1.),(1.,1.),(1.,1.),(1.,1.),(1.,
1.),(1.,1.),(1.,1.),(1.,1.),(1.,1.),(1.,1.),(1.,1.),(1.,1.)))
REPRESENTATION_ITEM('')
SURFACE()
);
#555=(
BOUNDED_SURFACE()
B_SPLINE_SURFACE(5,1,((#56510,#56511),(#56512,#56513),(#56514,#56515),(#56516,
#56517),(#56518,#56519),(#56520,#56521),(#56522,#56523),(#56524,#56525),
(#56526,#56527),(#56528,#56529),(#56530,#56531),(#56532,#56533),(#56534,
#56535),(#56536,#56537),(#56538,#56539),(#56540,#56541),(#56542,#56543),
(#56544,#56545),(#56546,#56547),(#56548,#56549),(#56550,#56551),(#56552,
#56553),(#56554,#56555),(#56556,#56557),(#56558,#56559),(#56560,#56561),
(#56562,#56563),(#56564,#56565),(#56566,#56567),(#56568,#56569),(#56570,
#56571),(#56572,#56573),(#56574,#56575),(#56576,#56577),(#56578,#56579),
(#56580,#56581),(#56582,#56583),(#56584,#56585),(#56586,#56587),(#56588,
#56589)),.UNSPECIFIED.,.F.,.F.,.F.)
B_SPLINE_SURFACE_WITH_KNOTS((6,1,1,1,1,1,1,1,1,1,1,1,1,1,1,1,1,1,1,1,1,
1,1,1,1,1,1,1,1,1,1,1,1,1,1,6),(2,2),(-1.,-0.971428571428572,-0.942857142857143,
-0.914285714285714,-0.885714285714286,-0.857142857142857,-0.828571428571429,
-0.8,-0.771428571428572,-0.742857142857143,-0.714285714285714,-0.685714285714286,
-0.657142857142857,-0.628571428571429,-0.6,-0.571428571428572,-0.542857142857143,
-0.514285714285714,-0.485714285714286,-0.457142857142857,-0.428571428571429,
-0.4,-0.371428571428571,-0.342857142857143,-0.314285714285714,-0.285714285714286,
-0.257142857142857,-0.228571428571429,-0.2,-0.171428571428571,-0.142857142857143,
-0.114285714285714,-0.0857142857142857,-0.0571428571428571,-0.0285714285714286,
0.),(0.,2.9),.UNSPECIFIED.)
GEOMETRIC_REPRESENTATION_ITEM()
RATIONAL_B_SPLINE_SURFACE(((1.,1.),(1.,1.),(1.,1.),(1.,1.),(1.,1.),(1.,
1.),(1.,1.),(1.,1.),(1.,1.),(1.,1.),(1.,1.),(1.,1.),(1.,1.),(1.,1.),(1.,
1.),(1.,1.),(1.,1.),(1.,1.),(1.,1.),(1.,1.),(1.,1.),(1.,1.),(1.,1.),(1.,
1.),(1.,1.),(1.,1.),(1.,1.),(1.,1.),(1.,1.),(1.,1.),(1.,1.),(1.,1.),(1.,
1.),(1.,1.),(1.,1.),(1.,1.),(1.,1.),(1.,1.),(1.,1.),(1.,1.)))
REPRESENTATION_ITEM('')
SURFACE()
);
#556=(
BOUNDED_SURFACE()
B_SPLINE_SURFACE(5,1,((#56606,#56607),(#56608,#56609),(#56610,#56611),(#56612,
#56613),(#56614,#56615),(#56616,#56617),(#56618,#56619),(#56620,#56621),
(#56622,#56623),(#56624,#56625),(#56626,#56627),(#56628,#56629),(#56630,
#56631),(#56632,#56633),(#56634,#56635),(#56636,#56637),(#56638,#56639),
(#56640,#56641),(#56642,#56643),(#56644,#56645),(#56646,#56647),(#56648,
#56649),(#56650,#56651),(#56652,#56653),(#56654,#56655),(#56656,#56657),
(#56658,#56659),(#56660,#56661),(#56662,#56663),(#56664,#56665),(#56666,
#56667),(#56668,#56669),(#56670,#56671),(#56672,#56673),(#56674,#56675),
(#56676,#56677),(#56678,#56679),(#56680,#56681),(#56682,#56683),(#56684,
#56685)),.UNSPECIFIED.,.F.,.F.,.F.)
B_SPLINE_SURFACE_WITH_KNOTS((6,1,1,1,1,1,1,1,1,1,1,1,1,1,1,1,1,1,1,1,1,
1,1,1,1,1,1,1,1,1,1,1,1,1,1,6),(2,2),(-1.,-0.971428571428572,-0.942857142857143,
-0.914285714285714,-0.885714285714286,-0.857142857142857,-0.828571428571429,
-0.8,-0.771428571428572,-0.742857142857143,-0.714285714285714,-0.685714285714286,
-0.657142857142857,-0.628571428571429,-0.6,-0.571428571428572,-0.542857142857143,
-0.514285714285714,-0.485714285714286,-0.457142857142857,-0.428571428571429,
-0.4,-0.371428571428571,-0.342857142857143,-0.314285714285714,-0.285714285714286,
-0.257142857142857,-0.228571428571429,-0.2,-0.171428571428571,-0.142857142857143,
-0.114285714285714,-0.0857142857142857,-0.0571428571428571,-0.0285714285714286,
0.),(0.,2.9),.UNSPECIFIED.)
GEOMETRIC_REPRESENTATION_ITEM()
RATIONAL_B_SPLINE_SURFACE(((1.,1.),(1.,1.),(1.,1.),(1.,1.),(1.,1.),(1.,
1.),(1.,1.),(1.,1.),(1.,1.),(1.,1.),(1.,1.),(1.,1.),(1.,1.),(1.,1.),(1.,
1.),(1.,1.),(1.,1.),(1.,1.),(1.,1.),(1.,1.),(1.,1.),(1.,1.),(1.,1.),(1.,
1.),(1.,1.),(1.,1.),(1.,1.),(1.,1.),(1.,1.),(1.,1.),(1.,1.),(1.,1.),(1.,
1.),(1.,1.),(1.,1.),(1.,1.),(1.,1.),(1.,1.),(1.,1.),(1.,1.)))
REPRESENTATION_ITEM('')
SURFACE()
);
#557=(
BOUNDED_SURFACE()
B_SPLINE_SURFACE(5,1,((#56700,#56701),(#56702,#56703),(#56704,#56705),(#56706,
#56707),(#56708,#56709),(#56710,#56711),(#56712,#56713),(#56714,#56715),
(#56716,#56717),(#56718,#56719),(#56720,#56721),(#56722,#56723),(#56724,
#56725),(#56726,#56727),(#56728,#56729),(#56730,#56731),(#56732,#56733),
(#56734,#56735),(#56736,#56737),(#56738,#56739),(#56740,#56741),(#56742,
#56743),(#56744,#56745),(#56746,#56747),(#56748,#56749),(#56750,#56751),
(#56752,#56753),(#56754,#56755),(#56756,#56757),(#56758,#56759),(#56760,
#56761),(#56762,#56763),(#56764,#56765),(#56766,#56767),(#56768,#56769),
(#56770,#56771),(#56772,#56773),(#56774,#56775),(#56776,#56777),(#56778,
#56779)),.UNSPECIFIED.,.F.,.F.,.F.)
B_SPLINE_SURFACE_WITH_KNOTS((6,1,1,1,1,1,1,1,1,1,1,1,1,1,1,1,1,1,1,1,1,
1,1,1,1,1,1,1,1,1,1,1,1,1,1,6),(2,2),(-1.,-0.971428571428572,-0.942857142857143,
-0.914285714285714,-0.885714285714286,-0.857142857142857,-0.828571428571429,
-0.8,-0.771428571428572,-0.742857142857143,-0.714285714285714,-0.685714285714286,
-0.657142857142857,-0.628571428571429,-0.6,-0.571428571428572,-0.542857142857143,
-0.514285714285714,-0.485714285714286,-0.457142857142857,-0.428571428571429,
-0.4,-0.371428571428571,-0.342857142857143,-0.314285714285714,-0.285714285714286,
-0.257142857142857,-0.228571428571429,-0.2,-0.171428571428571,-0.142857142857143,
-0.114285714285714,-0.0857142857142857,-0.0571428571428571,-0.0285714285714286,
0.),(0.,2.9),.UNSPECIFIED.)
GEOMETRIC_REPRESENTATION_ITEM()
RATIONAL_B_SPLINE_SURFACE(((1.,1.),(1.,1.),(1.,1.),(1.,1.),(1.,1.),(1.,
1.),(1.,1.),(1.,1.),(1.,1.),(1.,1.),(1.,1.),(1.,1.),(1.,1.),(1.,1.),(1.,
1.),(1.,1.),(1.,1.),(1.,1.),(1.,1.),(1.,1.),(1.,1.),(1.,1.),(1.,1.),(1.,
1.),(1.,1.),(1.,1.),(1.,1.),(1.,1.),(1.,1.),(1.,1.),(1.,1.),(1.,1.),(1.,
1.),(1.,1.),(1.,1.),(1.,1.),(1.,1.),(1.,1.),(1.,1.),(1.,1.)))
REPRESENTATION_ITEM('')
SURFACE()
);
#558=(
BOUNDED_SURFACE()
B_SPLINE_SURFACE(5,1,((#56780,#56781),(#56782,#56783),(#56784,#56785),(#56786,
#56787),(#56788,#56789),(#56790,#56791),(#56792,#56793),(#56794,#56795),
(#56796,#56797),(#56798,#56799),(#56800,#56801),(#56802,#56803),(#56804,
#56805),(#56806,#56807),(#56808,#56809),(#56810,#56811),(#56812,#56813),
(#56814,#56815),(#56816,#56817),(#56818,#56819),(#56820,#56821),(#56822,
#56823),(#56824,#56825),(#56826,#56827),(#56828,#56829),(#56830,#56831),
(#56832,#56833),(#56834,#56835),(#56836,#56837),(#56838,#56839),(#56840,
#56841),(#56842,#56843),(#56844,#56845),(#56846,#56847),(#56848,#56849),
(#56850,#56851),(#56852,#56853),(#56854,#56855),(#56856,#56857),(#56858,
#56859)),.UNSPECIFIED.,.F.,.F.,.F.)
B_SPLINE_SURFACE_WITH_KNOTS((6,1,1,1,1,1,1,1,1,1,1,1,1,1,1,1,1,1,1,1,1,
1,1,1,1,1,1,1,1,1,1,1,1,1,1,6),(2,2),(-1.,-0.971428571428572,-0.942857142857143,
-0.914285714285714,-0.885714285714286,-0.857142857142857,-0.828571428571429,
-0.8,-0.771428571428572,-0.742857142857143,-0.714285714285714,-0.685714285714286,
-0.657142857142857,-0.628571428571429,-0.6,-0.571428571428572,-0.542857142857143,
-0.514285714285714,-0.485714285714286,-0.457142857142857,-0.428571428571429,
-0.4,-0.371428571428571,-0.342857142857143,-0.314285714285714,-0.285714285714286,
-0.257142857142857,-0.228571428571429,-0.2,-0.171428571428571,-0.142857142857143,
-0.114285714285714,-0.0857142857142857,-0.0571428571428571,-0.0285714285714286,
0.),(0.,1.6),.UNSPECIFIED.)
GEOMETRIC_REPRESENTATION_ITEM()
RATIONAL_B_SPLINE_SURFACE(((1.,1.),(1.,1.),(1.,1.),(1.,1.),(1.,1.),(1.,
1.),(1.,1.),(1.,1.),(1.,1.),(1.,1.),(1.,1.),(1.,1.),(1.,1.),(1.,1.),(1.,
1.),(1.,1.),(1.,1.),(1.,1.),(1.,1.),(1.,1.),(1.,1.),(1.,1.),(1.,1.),(1.,
1.),(1.,1.),(1.,1.),(1.,1.),(1.,1.),(1.,1.),(1.,1.),(1.,1.),(1.,1.),(1.,
1.),(1.,1.),(1.,1.),(1.,1.),(1.,1.),(1.,1.),(1.,1.),(1.,1.)))
REPRESENTATION_ITEM('')
SURFACE()
);
#559=(
BOUNDED_SURFACE()
B_SPLINE_SURFACE(5,1,((#56879,#56880),(#56881,#56882),(#56883,#56884),(#56885,
#56886),(#56887,#56888),(#56889,#56890),(#56891,#56892),(#56893,#56894),
(#56895,#56896),(#56897,#56898),(#56899,#56900),(#56901,#56902),(#56903,
#56904),(#56905,#56906),(#56907,#56908),(#56909,#56910),(#56911,#56912),
(#56913,#56914),(#56915,#56916),(#56917,#56918),(#56919,#56920),(#56921,
#56922),(#56923,#56924),(#56925,#56926),(#56927,#56928),(#56929,#56930),
(#56931,#56932),(#56933,#56934),(#56935,#56936),(#56937,#56938),(#56939,
#56940),(#56941,#56942),(#56943,#56944),(#56945,#56946),(#56947,#56948),
(#56949,#56950),(#56951,#56952),(#56953,#56954),(#56955,#56956),(#56957,
#56958)),.UNSPECIFIED.,.F.,.F.,.F.)
B_SPLINE_SURFACE_WITH_KNOTS((6,1,1,1,1,1,1,1,1,1,1,1,1,1,1,1,1,1,1,1,1,
1,1,1,1,1,1,1,1,1,1,1,1,1,1,6),(2,2),(-1.,-0.971428571428572,-0.942857142857143,
-0.914285714285714,-0.885714285714286,-0.857142857142857,-0.828571428571429,
-0.8,-0.771428571428572,-0.742857142857143,-0.714285714285714,-0.685714285714286,
-0.657142857142857,-0.628571428571429,-0.6,-0.571428571428572,-0.542857142857143,
-0.514285714285714,-0.485714285714286,-0.457142857142857,-0.428571428571429,
-0.4,-0.371428571428571,-0.342857142857143,-0.314285714285714,-0.285714285714286,
-0.257142857142857,-0.228571428571429,-0.2,-0.171428571428571,-0.142857142857143,
-0.114285714285714,-0.0857142857142857,-0.0571428571428571,-0.0285714285714286,
0.),(0.,1.6),.UNSPECIFIED.)
GEOMETRIC_REPRESENTATION_ITEM()
RATIONAL_B_SPLINE_SURFACE(((1.,1.),(1.,1.),(1.,1.),(1.,1.),(1.,1.),(1.,
1.),(1.,1.),(1.,1.),(1.,1.),(1.,1.),(1.,1.),(1.,1.),(1.,1.),(1.,1.),(1.,
1.),(1.,1.),(1.,1.),(1.,1.),(1.,1.),(1.,1.),(1.,1.),(1.,1.),(1.,1.),(1.,
1.),(1.,1.),(1.,1.),(1.,1.),(1.,1.),(1.,1.),(1.,1.),(1.,1.),(1.,1.),(1.,
1.),(1.,1.),(1.,1.),(1.,1.),(1.,1.),(1.,1.),(1.,1.),(1.,1.)))
REPRESENTATION_ITEM('')
SURFACE()
);
#560=(
BOUNDED_SURFACE()
B_SPLINE_SURFACE(5,1,((#57004,#57005),(#57006,#57007),(#57008,#57009),(#57010,
#57011),(#57012,#57013),(#57014,#57015),(#57016,#57017),(#57018,#57019),
(#57020,#57021),(#57022,#57023),(#57024,#57025),(#57026,#57027),(#57028,
#57029),(#57030,#57031),(#57032,#57033),(#57034,#57035),(#57036,#57037),
(#57038,#57039),(#57040,#57041),(#57042,#57043),(#57044,#57045),(#57046,
#57047),(#57048,#57049),(#57050,#57051),(#57052,#57053),(#57054,#57055),
(#57056,#57057),(#57058,#57059),(#57060,#57061),(#57062,#57063),(#57064,
#57065),(#57066,#57067),(#57068,#57069),(#57070,#57071),(#57072,#57073),
(#57074,#57075),(#57076,#57077),(#57078,#57079),(#57080,#57081),(#57082,
#57083)),.UNSPECIFIED.,.F.,.F.,.F.)
B_SPLINE_SURFACE_WITH_KNOTS((6,1,1,1,1,1,1,1,1,1,1,1,1,1,1,1,1,1,1,1,1,
1,1,1,1,1,1,1,1,1,1,1,1,1,1,6),(2,2),(-1.,-0.971428571428572,-0.942857142857143,
-0.914285714285714,-0.885714285714286,-0.857142857142857,-0.828571428571429,
-0.8,-0.771428571428572,-0.742857142857143,-0.714285714285714,-0.685714285714286,
-0.657142857142857,-0.628571428571429,-0.6,-0.571428571428572,-0.542857142857143,
-0.514285714285714,-0.485714285714286,-0.457142857142857,-0.428571428571429,
-0.4,-0.371428571428571,-0.342857142857143,-0.314285714285714,-0.285714285714286,
-0.257142857142857,-0.228571428571429,-0.2,-0.171428571428571,-0.142857142857143,
-0.114285714285714,-0.0857142857142857,-0.0571428571428571,-0.0285714285714286,
0.),(0.,1.6),.UNSPECIFIED.)
GEOMETRIC_REPRESENTATION_ITEM()
RATIONAL_B_SPLINE_SURFACE(((1.,1.),(1.,1.),(1.,1.),(1.,1.),(1.,1.),(1.,
1.),(1.,1.),(1.,1.),(1.,1.),(1.,1.),(1.,1.),(1.,1.),(1.,1.),(1.,1.),(1.,
1.),(1.,1.),(1.,1.),(1.,1.),(1.,1.),(1.,1.),(1.,1.),(1.,1.),(1.,1.),(1.,
1.),(1.,1.),(1.,1.),(1.,1.),(1.,1.),(1.,1.),(1.,1.),(1.,1.),(1.,1.),(1.,
1.),(1.,1.),(1.,1.),(1.,1.),(1.,1.),(1.,1.),(1.,1.),(1.,1.)))
REPRESENTATION_ITEM('')
SURFACE()
);
#561=(
BOUNDED_SURFACE()
B_SPLINE_SURFACE(5,1,((#57103,#57104),(#57105,#57106),(#57107,#57108),(#57109,
#57110),(#57111,#57112),(#57113,#57114),(#57115,#57116),(#57117,#57118),
(#57119,#57120),(#57121,#57122),(#57123,#57124),(#57125,#57126),(#57127,
#57128),(#57129,#57130),(#57131,#57132),(#57133,#57134),(#57135,#57136),
(#57137,#57138),(#57139,#57140),(#57141,#57142),(#57143,#57144),(#57145,
#57146),(#57147,#57148),(#57149,#57150),(#57151,#57152),(#57153,#57154),
(#57155,#57156),(#57157,#57158),(#57159,#57160),(#57161,#57162),(#57163,
#57164),(#57165,#57166),(#57167,#57168),(#57169,#57170),(#57171,#57172),
(#57173,#57174),(#57175,#57176),(#57177,#57178),(#57179,#57180),(#57181,
#57182)),.UNSPECIFIED.,.F.,.F.,.F.)
B_SPLINE_SURFACE_WITH_KNOTS((6,1,1,1,1,1,1,1,1,1,1,1,1,1,1,1,1,1,1,1,1,
1,1,1,1,1,1,1,1,1,1,1,1,1,1,6),(2,2),(-1.,-0.971428571428572,-0.942857142857143,
-0.914285714285714,-0.885714285714286,-0.857142857142857,-0.828571428571429,
-0.8,-0.771428571428572,-0.742857142857143,-0.714285714285714,-0.685714285714286,
-0.657142857142857,-0.628571428571429,-0.6,-0.571428571428572,-0.542857142857143,
-0.514285714285714,-0.485714285714286,-0.457142857142857,-0.428571428571429,
-0.4,-0.371428571428571,-0.342857142857143,-0.314285714285714,-0.285714285714286,
-0.257142857142857,-0.228571428571429,-0.2,-0.171428571428571,-0.142857142857143,
-0.114285714285714,-0.0857142857142857,-0.0571428571428571,-0.0285714285714286,
0.),(0.,1.6),.UNSPECIFIED.)
GEOMETRIC_REPRESENTATION_ITEM()
RATIONAL_B_SPLINE_SURFACE(((1.,1.),(1.,1.),(1.,1.),(1.,1.),(1.,1.),(1.,
1.),(1.,1.),(1.,1.),(1.,1.),(1.,1.),(1.,1.),(1.,1.),(1.,1.),(1.,1.),(1.,
1.),(1.,1.),(1.,1.),(1.,1.),(1.,1.),(1.,1.),(1.,1.),(1.,1.),(1.,1.),(1.,
1.),(1.,1.),(1.,1.),(1.,1.),(1.,1.),(1.,1.),(1.,1.),(1.,1.),(1.,1.),(1.,
1.),(1.,1.),(1.,1.),(1.,1.),(1.,1.),(1.,1.),(1.,1.),(1.,1.)))
REPRESENTATION_ITEM('')
SURFACE()
);
#562=(
BOUNDED_SURFACE()
B_SPLINE_SURFACE(5,1,((#57202,#57203),(#57204,#57205),(#57206,#57207),(#57208,
#57209),(#57210,#57211),(#57212,#57213),(#57214,#57215),(#57216,#57217),
(#57218,#57219),(#57220,#57221),(#57222,#57223),(#57224,#57225),(#57226,
#57227),(#57228,#57229),(#57230,#57231),(#57232,#57233),(#57234,#57235),
(#57236,#57237),(#57238,#57239),(#57240,#57241),(#57242,#57243),(#57244,
#57245),(#57246,#57247),(#57248,#57249),(#57250,#57251),(#57252,#57253),
(#57254,#57255),(#57256,#57257),(#57258,#57259),(#57260,#57261),(#57262,
#57263),(#57264,#57265),(#57266,#57267),(#57268,#57269),(#57270,#57271),
(#57272,#57273),(#57274,#57275),(#57276,#57277),(#57278,#57279),(#57280,
#57281)),.UNSPECIFIED.,.F.,.F.,.F.)
B_SPLINE_SURFACE_WITH_KNOTS((6,1,1,1,1,1,1,1,1,1,1,1,1,1,1,1,1,1,1,1,1,
1,1,1,1,1,1,1,1,1,1,1,1,1,1,6),(2,2),(-1.,-0.971428571428572,-0.942857142857143,
-0.914285714285714,-0.885714285714286,-0.857142857142857,-0.828571428571429,
-0.8,-0.771428571428572,-0.742857142857143,-0.714285714285714,-0.685714285714286,
-0.657142857142857,-0.628571428571429,-0.6,-0.571428571428572,-0.542857142857143,
-0.514285714285714,-0.485714285714286,-0.457142857142857,-0.428571428571429,
-0.4,-0.371428571428571,-0.342857142857143,-0.314285714285714,-0.285714285714286,
-0.257142857142857,-0.228571428571429,-0.2,-0.171428571428571,-0.142857142857143,
-0.114285714285714,-0.0857142857142857,-0.0571428571428571,-0.0285714285714286,
0.),(0.,1.6),.UNSPECIFIED.)
GEOMETRIC_REPRESENTATION_ITEM()
RATIONAL_B_SPLINE_SURFACE(((1.,1.),(1.,1.),(1.,1.),(1.,1.),(1.,1.),(1.,
1.),(1.,1.),(1.,1.),(1.,1.),(1.,1.),(1.,1.),(1.,1.),(1.,1.),(1.,1.),(1.,
1.),(1.,1.),(1.,1.),(1.,1.),(1.,1.),(1.,1.),(1.,1.),(1.,1.),(1.,1.),(1.,
1.),(1.,1.),(1.,1.),(1.,1.),(1.,1.),(1.,1.),(1.,1.),(1.,1.),(1.,1.),(1.,
1.),(1.,1.),(1.,1.),(1.,1.),(1.,1.),(1.,1.),(1.,1.),(1.,1.)))
REPRESENTATION_ITEM('')
SURFACE()
);
#563=(
BOUNDED_SURFACE()
B_SPLINE_SURFACE(5,1,((#57301,#57302),(#57303,#57304),(#57305,#57306),(#57307,
#57308),(#57309,#57310),(#57311,#57312),(#57313,#57314),(#57315,#57316),
(#57317,#57318),(#57319,#57320),(#57321,#57322),(#57323,#57324),(#57325,
#57326),(#57327,#57328),(#57329,#57330),(#57331,#57332),(#57333,#57334),
(#57335,#57336),(#57337,#57338),(#57339,#57340),(#57341,#57342),(#57343,
#57344),(#57345,#57346),(#57347,#57348),(#57349,#57350),(#57351,#57352),
(#57353,#57354),(#57355,#57356),(#57357,#57358),(#57359,#57360),(#57361,
#57362),(#57363,#57364),(#57365,#57366),(#57367,#57368),(#57369,#57370),
(#57371,#57372),(#57373,#57374),(#57375,#57376),(#57377,#57378),(#57379,
#57380)),.UNSPECIFIED.,.F.,.F.,.F.)
B_SPLINE_SURFACE_WITH_KNOTS((6,1,1,1,1,1,1,1,1,1,1,1,1,1,1,1,1,1,1,1,1,
1,1,1,1,1,1,1,1,1,1,1,1,1,1,6),(2,2),(-1.,-0.971428571428572,-0.942857142857143,
-0.914285714285714,-0.885714285714286,-0.857142857142857,-0.828571428571429,
-0.8,-0.771428571428572,-0.742857142857143,-0.714285714285714,-0.685714285714286,
-0.657142857142857,-0.628571428571429,-0.6,-0.571428571428572,-0.542857142857143,
-0.514285714285714,-0.485714285714286,-0.457142857142857,-0.428571428571429,
-0.4,-0.371428571428571,-0.342857142857143,-0.314285714285714,-0.285714285714286,
-0.257142857142857,-0.228571428571429,-0.2,-0.171428571428571,-0.142857142857143,
-0.114285714285714,-0.0857142857142857,-0.0571428571428571,-0.0285714285714286,
0.),(0.,1.6),.UNSPECIFIED.)
GEOMETRIC_REPRESENTATION_ITEM()
RATIONAL_B_SPLINE_SURFACE(((1.,1.),(1.,1.),(1.,1.),(1.,1.),(1.,1.),(1.,
1.),(1.,1.),(1.,1.),(1.,1.),(1.,1.),(1.,1.),(1.,1.),(1.,1.),(1.,1.),(1.,
1.),(1.,1.),(1.,1.),(1.,1.),(1.,1.),(1.,1.),(1.,1.),(1.,1.),(1.,1.),(1.,
1.),(1.,1.),(1.,1.),(1.,1.),(1.,1.),(1.,1.),(1.,1.),(1.,1.),(1.,1.),(1.,
1.),(1.,1.),(1.,1.),(1.,1.),(1.,1.),(1.,1.),(1.,1.),(1.,1.)))
REPRESENTATION_ITEM('')
SURFACE()
);
#564=(
BOUNDED_SURFACE()
B_SPLINE_SURFACE(5,1,((#57400,#57401),(#57402,#57403),(#57404,#57405),(#57406,
#57407),(#57408,#57409),(#57410,#57411),(#57412,#57413),(#57414,#57415),
(#57416,#57417),(#57418,#57419),(#57420,#57421),(#57422,#57423),(#57424,
#57425),(#57426,#57427),(#57428,#57429),(#57430,#57431),(#57432,#57433),
(#57434,#57435),(#57436,#57437),(#57438,#57439),(#57440,#57441),(#57442,
#57443),(#57444,#57445),(#57446,#57447),(#57448,#57449),(#57450,#57451),
(#57452,#57453),(#57454,#57455),(#57456,#57457),(#57458,#57459),(#57460,
#57461),(#57462,#57463),(#57464,#57465),(#57466,#57467),(#57468,#57469),
(#57470,#57471),(#57472,#57473),(#57474,#57475),(#57476,#57477),(#57478,
#57479)),.UNSPECIFIED.,.F.,.F.,.F.)
B_SPLINE_SURFACE_WITH_KNOTS((6,1,1,1,1,1,1,1,1,1,1,1,1,1,1,1,1,1,1,1,1,
1,1,1,1,1,1,1,1,1,1,1,1,1,1,6),(2,2),(-1.,-0.971428571428572,-0.942857142857143,
-0.914285714285714,-0.885714285714286,-0.857142857142857,-0.828571428571429,
-0.8,-0.771428571428572,-0.742857142857143,-0.714285714285714,-0.685714285714286,
-0.657142857142857,-0.628571428571429,-0.6,-0.571428571428572,-0.542857142857143,
-0.514285714285714,-0.485714285714286,-0.457142857142857,-0.428571428571429,
-0.4,-0.371428571428571,-0.342857142857143,-0.314285714285714,-0.285714285714286,
-0.257142857142857,-0.228571428571429,-0.2,-0.171428571428571,-0.142857142857143,
-0.114285714285714,-0.0857142857142857,-0.0571428571428571,-0.0285714285714286,
0.),(0.,1.6),.UNSPECIFIED.)
GEOMETRIC_REPRESENTATION_ITEM()
RATIONAL_B_SPLINE_SURFACE(((1.,1.),(1.,1.),(1.,1.),(1.,1.),(1.,1.),(1.,
1.),(1.,1.),(1.,1.),(1.,1.),(1.,1.),(1.,1.),(1.,1.),(1.,1.),(1.,1.),(1.,
1.),(1.,1.),(1.,1.),(1.,1.),(1.,1.),(1.,1.),(1.,1.),(1.,1.),(1.,1.),(1.,
1.),(1.,1.),(1.,1.),(1.,1.),(1.,1.),(1.,1.),(1.,1.),(1.,1.),(1.,1.),(1.,
1.),(1.,1.),(1.,1.),(1.,1.),(1.,1.),(1.,1.),(1.,1.),(1.,1.)))
REPRESENTATION_ITEM('')
SURFACE()
);
#565=(
BOUNDED_SURFACE()
B_SPLINE_SURFACE(5,1,((#57499,#57500),(#57501,#57502),(#57503,#57504),(#57505,
#57506),(#57507,#57508),(#57509,#57510),(#57511,#57512),(#57513,#57514),
(#57515,#57516),(#57517,#57518),(#57519,#57520),(#57521,#57522),(#57523,
#57524),(#57525,#57526),(#57527,#57528),(#57529,#57530),(#57531,#57532),
(#57533,#57534),(#57535,#57536),(#57537,#57538),(#57539,#57540),(#57541,
#57542),(#57543,#57544),(#57545,#57546),(#57547,#57548),(#57549,#57550),
(#57551,#57552),(#57553,#57554),(#57555,#57556),(#57557,#57558),(#57559,
#57560),(#57561,#57562),(#57563,#57564),(#57565,#57566),(#57567,#57568),
(#57569,#57570),(#57571,#57572),(#57573,#57574),(#57575,#57576),(#57577,
#57578)),.UNSPECIFIED.,.F.,.F.,.F.)
B_SPLINE_SURFACE_WITH_KNOTS((6,1,1,1,1,1,1,1,1,1,1,1,1,1,1,1,1,1,1,1,1,
1,1,1,1,1,1,1,1,1,1,1,1,1,1,6),(2,2),(-1.,-0.971428571428572,-0.942857142857143,
-0.914285714285714,-0.885714285714286,-0.857142857142857,-0.828571428571429,
-0.8,-0.771428571428572,-0.742857142857143,-0.714285714285714,-0.685714285714286,
-0.657142857142857,-0.628571428571429,-0.6,-0.571428571428572,-0.542857142857143,
-0.514285714285714,-0.485714285714286,-0.457142857142857,-0.428571428571429,
-0.4,-0.371428571428571,-0.342857142857143,-0.314285714285714,-0.285714285714286,
-0.257142857142857,-0.228571428571429,-0.2,-0.171428571428571,-0.142857142857143,
-0.114285714285714,-0.0857142857142857,-0.0571428571428571,-0.0285714285714286,
0.),(0.,1.6),.UNSPECIFIED.)
GEOMETRIC_REPRESENTATION_ITEM()
RATIONAL_B_SPLINE_SURFACE(((1.,1.),(1.,1.),(1.,1.),(1.,1.),(1.,1.),(1.,
1.),(1.,1.),(1.,1.),(1.,1.),(1.,1.),(1.,1.),(1.,1.),(1.,1.),(1.,1.),(1.,
1.),(1.,1.),(1.,1.),(1.,1.),(1.,1.),(1.,1.),(1.,1.),(1.,1.),(1.,1.),(1.,
1.),(1.,1.),(1.,1.),(1.,1.),(1.,1.),(1.,1.),(1.,1.),(1.,1.),(1.,1.),(1.,
1.),(1.,1.),(1.,1.),(1.,1.),(1.,1.),(1.,1.),(1.,1.),(1.,1.)))
REPRESENTATION_ITEM('')
SURFACE()
);
#566=(
BOUNDED_SURFACE()
B_SPLINE_SURFACE(5,1,((#57598,#57599),(#57600,#57601),(#57602,#57603),(#57604,
#57605),(#57606,#57607),(#57608,#57609),(#57610,#57611),(#57612,#57613),
(#57614,#57615),(#57616,#57617),(#57618,#57619),(#57620,#57621),(#57622,
#57623),(#57624,#57625),(#57626,#57627),(#57628,#57629),(#57630,#57631),
(#57632,#57633),(#57634,#57635),(#57636,#57637),(#57638,#57639),(#57640,
#57641),(#57642,#57643),(#57644,#57645),(#57646,#57647),(#57648,#57649),
(#57650,#57651),(#57652,#57653),(#57654,#57655),(#57656,#57657),(#57658,
#57659),(#57660,#57661),(#57662,#57663),(#57664,#57665),(#57666,#57667),
(#57668,#57669),(#57670,#57671),(#57672,#57673),(#57674,#57675),(#57676,
#57677)),.UNSPECIFIED.,.F.,.F.,.F.)
B_SPLINE_SURFACE_WITH_KNOTS((6,1,1,1,1,1,1,1,1,1,1,1,1,1,1,1,1,1,1,1,1,
1,1,1,1,1,1,1,1,1,1,1,1,1,1,6),(2,2),(-1.,-0.971428571428572,-0.942857142857143,
-0.914285714285714,-0.885714285714286,-0.857142857142857,-0.828571428571429,
-0.8,-0.771428571428572,-0.742857142857143,-0.714285714285714,-0.685714285714286,
-0.657142857142857,-0.628571428571429,-0.6,-0.571428571428572,-0.542857142857143,
-0.514285714285714,-0.485714285714286,-0.457142857142857,-0.428571428571429,
-0.4,-0.371428571428571,-0.342857142857143,-0.314285714285714,-0.285714285714286,
-0.257142857142857,-0.228571428571429,-0.2,-0.171428571428571,-0.142857142857143,
-0.114285714285714,-0.0857142857142857,-0.0571428571428571,-0.0285714285714286,
0.),(0.,1.6),.UNSPECIFIED.)
GEOMETRIC_REPRESENTATION_ITEM()
RATIONAL_B_SPLINE_SURFACE(((1.,1.),(1.,1.),(1.,1.),(1.,1.),(1.,1.),(1.,
1.),(1.,1.),(1.,1.),(1.,1.),(1.,1.),(1.,1.),(1.,1.),(1.,1.),(1.,1.),(1.,
1.),(1.,1.),(1.,1.),(1.,1.),(1.,1.),(1.,1.),(1.,1.),(1.,1.),(1.,1.),(1.,
1.),(1.,1.),(1.,1.),(1.,1.),(1.,1.),(1.,1.),(1.,1.),(1.,1.),(1.,1.),(1.,
1.),(1.,1.),(1.,1.),(1.,1.),(1.,1.),(1.,1.),(1.,1.),(1.,1.)))
REPRESENTATION_ITEM('')
SURFACE()
);
#567=(
BOUNDED_SURFACE()
B_SPLINE_SURFACE(5,1,((#57697,#57698),(#57699,#57700),(#57701,#57702),(#57703,
#57704),(#57705,#57706),(#57707,#57708),(#57709,#57710),(#57711,#57712),
(#57713,#57714),(#57715,#57716),(#57717,#57718),(#57719,#57720),(#57721,
#57722),(#57723,#57724),(#57725,#57726),(#57727,#57728),(#57729,#57730),
(#57731,#57732),(#57733,#57734),(#57735,#57736),(#57737,#57738),(#57739,
#57740),(#57741,#57742),(#57743,#57744),(#57745,#57746),(#57747,#57748),
(#57749,#57750),(#57751,#57752),(#57753,#57754),(#57755,#57756),(#57757,
#57758),(#57759,#57760),(#57761,#57762),(#57763,#57764),(#57765,#57766),
(#57767,#57768),(#57769,#57770),(#57771,#57772),(#57773,#57774),(#57775,
#57776)),.UNSPECIFIED.,.F.,.F.,.F.)
B_SPLINE_SURFACE_WITH_KNOTS((6,1,1,1,1,1,1,1,1,1,1,1,1,1,1,1,1,1,1,1,1,
1,1,1,1,1,1,1,1,1,1,1,1,1,1,6),(2,2),(-1.,-0.971428571428572,-0.942857142857143,
-0.914285714285714,-0.885714285714286,-0.857142857142857,-0.828571428571429,
-0.8,-0.771428571428572,-0.742857142857143,-0.714285714285714,-0.685714285714286,
-0.657142857142857,-0.628571428571429,-0.6,-0.571428571428572,-0.542857142857143,
-0.514285714285714,-0.485714285714286,-0.457142857142857,-0.428571428571429,
-0.4,-0.371428571428571,-0.342857142857143,-0.314285714285714,-0.285714285714286,
-0.257142857142857,-0.228571428571429,-0.2,-0.171428571428571,-0.142857142857143,
-0.114285714285714,-0.0857142857142857,-0.0571428571428571,-0.0285714285714286,
0.),(0.,1.6),.UNSPECIFIED.)
GEOMETRIC_REPRESENTATION_ITEM()
RATIONAL_B_SPLINE_SURFACE(((1.,1.),(1.,1.),(1.,1.),(1.,1.),(1.,1.),(1.,
1.),(1.,1.),(1.,1.),(1.,1.),(1.,1.),(1.,1.),(1.,1.),(1.,1.),(1.,1.),(1.,
1.),(1.,1.),(1.,1.),(1.,1.),(1.,1.),(1.,1.),(1.,1.),(1.,1.),(1.,1.),(1.,
1.),(1.,1.),(1.,1.),(1.,1.),(1.,1.),(1.,1.),(1.,1.),(1.,1.),(1.,1.),(1.,
1.),(1.,1.),(1.,1.),(1.,1.),(1.,1.),(1.,1.),(1.,1.),(1.,1.)))
REPRESENTATION_ITEM('')
SURFACE()
);
#568=(
BOUNDED_SURFACE()
B_SPLINE_SURFACE(5,1,((#57796,#57797),(#57798,#57799),(#57800,#57801),(#57802,
#57803),(#57804,#57805),(#57806,#57807),(#57808,#57809),(#57810,#57811),
(#57812,#57813),(#57814,#57815),(#57816,#57817),(#57818,#57819),(#57820,
#57821),(#57822,#57823),(#57824,#57825),(#57826,#57827),(#57828,#57829),
(#57830,#57831),(#57832,#57833),(#57834,#57835),(#57836,#57837),(#57838,
#57839),(#57840,#57841),(#57842,#57843),(#57844,#57845),(#57846,#57847),
(#57848,#57849),(#57850,#57851),(#57852,#57853),(#57854,#57855),(#57856,
#57857),(#57858,#57859),(#57860,#57861),(#57862,#57863),(#57864,#57865),
(#57866,#57867),(#57868,#57869),(#57870,#57871),(#57872,#57873),(#57874,
#57875)),.UNSPECIFIED.,.F.,.F.,.F.)
B_SPLINE_SURFACE_WITH_KNOTS((6,1,1,1,1,1,1,1,1,1,1,1,1,1,1,1,1,1,1,1,1,
1,1,1,1,1,1,1,1,1,1,1,1,1,1,6),(2,2),(-1.,-0.971428571428572,-0.942857142857143,
-0.914285714285714,-0.885714285714286,-0.857142857142857,-0.828571428571429,
-0.8,-0.771428571428572,-0.742857142857143,-0.714285714285714,-0.685714285714286,
-0.657142857142857,-0.628571428571429,-0.6,-0.571428571428572,-0.542857142857143,
-0.514285714285714,-0.485714285714286,-0.457142857142857,-0.428571428571429,
-0.4,-0.371428571428571,-0.342857142857143,-0.314285714285714,-0.285714285714286,
-0.257142857142857,-0.228571428571429,-0.2,-0.171428571428571,-0.142857142857143,
-0.114285714285714,-0.0857142857142857,-0.0571428571428571,-0.0285714285714286,
0.),(0.,1.6),.UNSPECIFIED.)
GEOMETRIC_REPRESENTATION_ITEM()
RATIONAL_B_SPLINE_SURFACE(((1.,1.),(1.,1.),(1.,1.),(1.,1.),(1.,1.),(1.,
1.),(1.,1.),(1.,1.),(1.,1.),(1.,1.),(1.,1.),(1.,1.),(1.,1.),(1.,1.),(1.,
1.),(1.,1.),(1.,1.),(1.,1.),(1.,1.),(1.,1.),(1.,1.),(1.,1.),(1.,1.),(1.,
1.),(1.,1.),(1.,1.),(1.,1.),(1.,1.),(1.,1.),(1.,1.),(1.,1.),(1.,1.),(1.,
1.),(1.,1.),(1.,1.),(1.,1.),(1.,1.),(1.,1.),(1.,1.),(1.,1.)))
REPRESENTATION_ITEM('')
SURFACE()
);
#569=(
BOUNDED_SURFACE()
B_SPLINE_SURFACE(5,1,((#57895,#57896),(#57897,#57898),(#57899,#57900),(#57901,
#57902),(#57903,#57904),(#57905,#57906),(#57907,#57908),(#57909,#57910),
(#57911,#57912),(#57913,#57914),(#57915,#57916),(#57917,#57918),(#57919,
#57920),(#57921,#57922),(#57923,#57924),(#57925,#57926),(#57927,#57928),
(#57929,#57930),(#57931,#57932),(#57933,#57934),(#57935,#57936),(#57937,
#57938),(#57939,#57940),(#57941,#57942),(#57943,#57944),(#57945,#57946),
(#57947,#57948),(#57949,#57950),(#57951,#57952),(#57953,#57954),(#57955,
#57956),(#57957,#57958),(#57959,#57960),(#57961,#57962),(#57963,#57964),
(#57965,#57966),(#57967,#57968),(#57969,#57970),(#57971,#57972),(#57973,
#57974)),.UNSPECIFIED.,.F.,.F.,.F.)
B_SPLINE_SURFACE_WITH_KNOTS((6,1,1,1,1,1,1,1,1,1,1,1,1,1,1,1,1,1,1,1,1,
1,1,1,1,1,1,1,1,1,1,1,1,1,1,6),(2,2),(-1.,-0.971428571428572,-0.942857142857143,
-0.914285714285714,-0.885714285714286,-0.857142857142857,-0.828571428571429,
-0.8,-0.771428571428572,-0.742857142857143,-0.714285714285714,-0.685714285714286,
-0.657142857142857,-0.628571428571429,-0.6,-0.571428571428572,-0.542857142857143,
-0.514285714285714,-0.485714285714286,-0.457142857142857,-0.428571428571429,
-0.4,-0.371428571428571,-0.342857142857143,-0.314285714285714,-0.285714285714286,
-0.257142857142857,-0.228571428571429,-0.2,-0.171428571428571,-0.142857142857143,
-0.114285714285714,-0.0857142857142857,-0.0571428571428571,-0.0285714285714286,
0.),(0.,1.6),.UNSPECIFIED.)
GEOMETRIC_REPRESENTATION_ITEM()
RATIONAL_B_SPLINE_SURFACE(((1.,1.),(1.,1.),(1.,1.),(1.,1.),(1.,1.),(1.,
1.),(1.,1.),(1.,1.),(1.,1.),(1.,1.),(1.,1.),(1.,1.),(1.,1.),(1.,1.),(1.,
1.),(1.,1.),(1.,1.),(1.,1.),(1.,1.),(1.,1.),(1.,1.),(1.,1.),(1.,1.),(1.,
1.),(1.,1.),(1.,1.),(1.,1.),(1.,1.),(1.,1.),(1.,1.),(1.,1.),(1.,1.),(1.,
1.),(1.,1.),(1.,1.),(1.,1.),(1.,1.),(1.,1.),(1.,1.),(1.,1.)))
REPRESENTATION_ITEM('')
SURFACE()
);
#570=(
BOUNDED_SURFACE()
B_SPLINE_SURFACE(5,1,((#58006,#58007),(#58008,#58009),(#58010,#58011),(#58012,
#58013),(#58014,#58015),(#58016,#58017),(#58018,#58019),(#58020,#58021),
(#58022,#58023),(#58024,#58025),(#58026,#58027),(#58028,#58029),(#58030,
#58031),(#58032,#58033),(#58034,#58035),(#58036,#58037),(#58038,#58039),
(#58040,#58041),(#58042,#58043),(#58044,#58045),(#58046,#58047),(#58048,
#58049),(#58050,#58051),(#58052,#58053),(#58054,#58055),(#58056,#58057),
(#58058,#58059),(#58060,#58061),(#58062,#58063),(#58064,#58065),(#58066,
#58067),(#58068,#58069),(#58070,#58071),(#58072,#58073),(#58074,#58075),
(#58076,#58077),(#58078,#58079),(#58080,#58081),(#58082,#58083),(#58084,
#58085)),.UNSPECIFIED.,.F.,.F.,.F.)
B_SPLINE_SURFACE_WITH_KNOTS((6,1,1,1,1,1,1,1,1,1,1,1,1,1,1,1,1,1,1,1,1,
1,1,1,1,1,1,1,1,1,1,1,1,1,1,6),(2,2),(-1.,-0.971428571428572,-0.942857142857143,
-0.914285714285714,-0.885714285714286,-0.857142857142857,-0.828571428571429,
-0.8,-0.771428571428572,-0.742857142857143,-0.714285714285714,-0.685714285714286,
-0.657142857142857,-0.628571428571429,-0.6,-0.571428571428572,-0.542857142857143,
-0.514285714285714,-0.485714285714286,-0.457142857142857,-0.428571428571429,
-0.4,-0.371428571428571,-0.342857142857143,-0.314285714285714,-0.285714285714286,
-0.257142857142857,-0.228571428571429,-0.2,-0.171428571428571,-0.142857142857143,
-0.114285714285714,-0.0857142857142857,-0.0571428571428571,-0.0285714285714286,
0.),(0.,1.6),.UNSPECIFIED.)
GEOMETRIC_REPRESENTATION_ITEM()
RATIONAL_B_SPLINE_SURFACE(((1.,1.),(1.,1.),(1.,1.),(1.,1.),(1.,1.),(1.,
1.),(1.,1.),(1.,1.),(1.,1.),(1.,1.),(1.,1.),(1.,1.),(1.,1.),(1.,1.),(1.,
1.),(1.,1.),(1.,1.),(1.,1.),(1.,1.),(1.,1.),(1.,1.),(1.,1.),(1.,1.),(1.,
1.),(1.,1.),(1.,1.),(1.,1.),(1.,1.),(1.,1.),(1.,1.),(1.,1.),(1.,1.),(1.,
1.),(1.,1.),(1.,1.),(1.,1.),(1.,1.),(1.,1.),(1.,1.),(1.,1.)))
REPRESENTATION_ITEM('')
SURFACE()
);
#571=(
BOUNDED_SURFACE()
B_SPLINE_SURFACE(5,1,((#58120,#58121),(#58122,#58123),(#58124,#58125),(#58126,
#58127),(#58128,#58129),(#58130,#58131),(#58132,#58133),(#58134,#58135),
(#58136,#58137),(#58138,#58139),(#58140,#58141),(#58142,#58143),(#58144,
#58145),(#58146,#58147),(#58148,#58149),(#58150,#58151),(#58152,#58153),
(#58154,#58155),(#58156,#58157),(#58158,#58159),(#58160,#58161),(#58162,
#58163),(#58164,#58165),(#58166,#58167),(#58168,#58169),(#58170,#58171),
(#58172,#58173),(#58174,#58175),(#58176,#58177),(#58178,#58179),(#58180,
#58181),(#58182,#58183),(#58184,#58185),(#58186,#58187),(#58188,#58189),
(#58190,#58191),(#58192,#58193),(#58194,#58195),(#58196,#58197),(#58198,
#58199)),.UNSPECIFIED.,.F.,.F.,.F.)
B_SPLINE_SURFACE_WITH_KNOTS((6,1,1,1,1,1,1,1,1,1,1,1,1,1,1,1,1,1,1,1,1,
1,1,1,1,1,1,1,1,1,1,1,1,1,1,6),(2,2),(-1.,-0.971428571428572,-0.942857142857143,
-0.914285714285714,-0.885714285714286,-0.857142857142857,-0.828571428571429,
-0.8,-0.771428571428572,-0.742857142857143,-0.714285714285714,-0.685714285714286,
-0.657142857142857,-0.628571428571429,-0.6,-0.571428571428572,-0.542857142857143,
-0.514285714285714,-0.485714285714286,-0.457142857142857,-0.428571428571429,
-0.4,-0.371428571428571,-0.342857142857143,-0.314285714285714,-0.285714285714286,
-0.257142857142857,-0.228571428571429,-0.2,-0.171428571428571,-0.142857142857143,
-0.114285714285714,-0.0857142857142857,-0.0571428571428571,-0.0285714285714286,
0.),(0.,1.6),.UNSPECIFIED.)
GEOMETRIC_REPRESENTATION_ITEM()
RATIONAL_B_SPLINE_SURFACE(((1.,1.),(1.,1.),(1.,1.),(1.,1.),(1.,1.),(1.,
1.),(1.,1.),(1.,1.),(1.,1.),(1.,1.),(1.,1.),(1.,1.),(1.,1.),(1.,1.),(1.,
1.),(1.,1.),(1.,1.),(1.,1.),(1.,1.),(1.,1.),(1.,1.),(1.,1.),(1.,1.),(1.,
1.),(1.,1.),(1.,1.),(1.,1.),(1.,1.),(1.,1.),(1.,1.),(1.,1.),(1.,1.),(1.,
1.),(1.,1.),(1.,1.),(1.,1.),(1.,1.),(1.,1.),(1.,1.),(1.,1.)))
REPRESENTATION_ITEM('')
SURFACE()
);
#572=(
BOUNDED_SURFACE()
B_SPLINE_SURFACE(5,1,((#58219,#58220),(#58221,#58222),(#58223,#58224),(#58225,
#58226),(#58227,#58228),(#58229,#58230),(#58231,#58232),(#58233,#58234),
(#58235,#58236),(#58237,#58238),(#58239,#58240),(#58241,#58242),(#58243,
#58244),(#58245,#58246),(#58247,#58248),(#58249,#58250),(#58251,#58252),
(#58253,#58254),(#58255,#58256),(#58257,#58258),(#58259,#58260),(#58261,
#58262),(#58263,#58264),(#58265,#58266),(#58267,#58268),(#58269,#58270),
(#58271,#58272),(#58273,#58274),(#58275,#58276),(#58277,#58278),(#58279,
#58280),(#58281,#58282),(#58283,#58284),(#58285,#58286),(#58287,#58288),
(#58289,#58290),(#58291,#58292),(#58293,#58294),(#58295,#58296),(#58297,
#58298)),.UNSPECIFIED.,.F.,.F.,.F.)
B_SPLINE_SURFACE_WITH_KNOTS((6,1,1,1,1,1,1,1,1,1,1,1,1,1,1,1,1,1,1,1,1,
1,1,1,1,1,1,1,1,1,1,1,1,1,1,6),(2,2),(-1.,-0.971428571428572,-0.942857142857143,
-0.914285714285714,-0.885714285714286,-0.857142857142857,-0.828571428571429,
-0.8,-0.771428571428572,-0.742857142857143,-0.714285714285714,-0.685714285714286,
-0.657142857142857,-0.628571428571429,-0.6,-0.571428571428572,-0.542857142857143,
-0.514285714285714,-0.485714285714286,-0.457142857142857,-0.428571428571429,
-0.4,-0.371428571428571,-0.342857142857143,-0.314285714285714,-0.285714285714286,
-0.257142857142857,-0.228571428571429,-0.2,-0.171428571428571,-0.142857142857143,
-0.114285714285714,-0.0857142857142857,-0.0571428571428571,-0.0285714285714286,
0.),(0.,1.6),.UNSPECIFIED.)
GEOMETRIC_REPRESENTATION_ITEM()
RATIONAL_B_SPLINE_SURFACE(((1.,1.),(1.,1.),(1.,1.),(1.,1.),(1.,1.),(1.,
1.),(1.,1.),(1.,1.),(1.,1.),(1.,1.),(1.,1.),(1.,1.),(1.,1.),(1.,1.),(1.,
1.),(1.,1.),(1.,1.),(1.,1.),(1.,1.),(1.,1.),(1.,1.),(1.,1.),(1.,1.),(1.,
1.),(1.,1.),(1.,1.),(1.,1.),(1.,1.),(1.,1.),(1.,1.),(1.,1.),(1.,1.),(1.,
1.),(1.,1.),(1.,1.),(1.,1.),(1.,1.),(1.,1.),(1.,1.),(1.,1.)))
REPRESENTATION_ITEM('')
SURFACE()
);
#573=(
BOUNDED_SURFACE()
B_SPLINE_SURFACE(5,1,((#58318,#58319),(#58320,#58321),(#58322,#58323),(#58324,
#58325),(#58326,#58327),(#58328,#58329),(#58330,#58331),(#58332,#58333),
(#58334,#58335),(#58336,#58337),(#58338,#58339),(#58340,#58341),(#58342,
#58343),(#58344,#58345),(#58346,#58347),(#58348,#58349),(#58350,#58351),
(#58352,#58353),(#58354,#58355),(#58356,#58357),(#58358,#58359),(#58360,
#58361),(#58362,#58363),(#58364,#58365),(#58366,#58367),(#58368,#58369),
(#58370,#58371),(#58372,#58373),(#58374,#58375),(#58376,#58377),(#58378,
#58379),(#58380,#58381),(#58382,#58383),(#58384,#58385),(#58386,#58387),
(#58388,#58389),(#58390,#58391),(#58392,#58393),(#58394,#58395),(#58396,
#58397)),.UNSPECIFIED.,.F.,.F.,.F.)
B_SPLINE_SURFACE_WITH_KNOTS((6,1,1,1,1,1,1,1,1,1,1,1,1,1,1,1,1,1,1,1,1,
1,1,1,1,1,1,1,1,1,1,1,1,1,1,6),(2,2),(-1.,-0.971428571428572,-0.942857142857143,
-0.914285714285714,-0.885714285714286,-0.857142857142857,-0.828571428571429,
-0.8,-0.771428571428572,-0.742857142857143,-0.714285714285714,-0.685714285714286,
-0.657142857142857,-0.628571428571429,-0.6,-0.571428571428572,-0.542857142857143,
-0.514285714285714,-0.485714285714286,-0.457142857142857,-0.428571428571429,
-0.4,-0.371428571428571,-0.342857142857143,-0.314285714285714,-0.285714285714286,
-0.257142857142857,-0.228571428571429,-0.2,-0.171428571428571,-0.142857142857143,
-0.114285714285714,-0.0857142857142857,-0.0571428571428571,-0.0285714285714286,
0.),(0.,1.6),.UNSPECIFIED.)
GEOMETRIC_REPRESENTATION_ITEM()
RATIONAL_B_SPLINE_SURFACE(((1.,1.),(1.,1.),(1.,1.),(1.,1.),(1.,1.),(1.,
1.),(1.,1.),(1.,1.),(1.,1.),(1.,1.),(1.,1.),(1.,1.),(1.,1.),(1.,1.),(1.,
1.),(1.,1.),(1.,1.),(1.,1.),(1.,1.),(1.,1.),(1.,1.),(1.,1.),(1.,1.),(1.,
1.),(1.,1.),(1.,1.),(1.,1.),(1.,1.),(1.,1.),(1.,1.),(1.,1.),(1.,1.),(1.,
1.),(1.,1.),(1.,1.),(1.,1.),(1.,1.),(1.,1.),(1.,1.),(1.,1.)))
REPRESENTATION_ITEM('')
SURFACE()
);
#574=(
BOUNDED_SURFACE()
B_SPLINE_SURFACE(5,1,((#58417,#58418),(#58419,#58420),(#58421,#58422),(#58423,
#58424),(#58425,#58426),(#58427,#58428),(#58429,#58430),(#58431,#58432),
(#58433,#58434),(#58435,#58436),(#58437,#58438),(#58439,#58440),(#58441,
#58442),(#58443,#58444),(#58445,#58446),(#58447,#58448),(#58449,#58450),
(#58451,#58452),(#58453,#58454),(#58455,#58456),(#58457,#58458),(#58459,
#58460),(#58461,#58462),(#58463,#58464),(#58465,#58466),(#58467,#58468),
(#58469,#58470),(#58471,#58472),(#58473,#58474),(#58475,#58476),(#58477,
#58478),(#58479,#58480),(#58481,#58482),(#58483,#58484),(#58485,#58486),
(#58487,#58488),(#58489,#58490),(#58491,#58492),(#58493,#58494),(#58495,
#58496)),.UNSPECIFIED.,.F.,.F.,.F.)
B_SPLINE_SURFACE_WITH_KNOTS((6,1,1,1,1,1,1,1,1,1,1,1,1,1,1,1,1,1,1,1,1,
1,1,1,1,1,1,1,1,1,1,1,1,1,1,6),(2,2),(-1.,-0.971428571428572,-0.942857142857143,
-0.914285714285714,-0.885714285714286,-0.857142857142857,-0.828571428571429,
-0.8,-0.771428571428572,-0.742857142857143,-0.714285714285714,-0.685714285714286,
-0.657142857142857,-0.628571428571429,-0.6,-0.571428571428572,-0.542857142857143,
-0.514285714285714,-0.485714285714286,-0.457142857142857,-0.428571428571429,
-0.4,-0.371428571428571,-0.342857142857143,-0.314285714285714,-0.285714285714286,
-0.257142857142857,-0.228571428571429,-0.2,-0.171428571428571,-0.142857142857143,
-0.114285714285714,-0.0857142857142857,-0.0571428571428571,-0.0285714285714286,
0.),(0.,1.6),.UNSPECIFIED.)
GEOMETRIC_REPRESENTATION_ITEM()
RATIONAL_B_SPLINE_SURFACE(((1.,1.),(1.,1.),(1.,1.),(1.,1.),(1.,1.),(1.,
1.),(1.,1.),(1.,1.),(1.,1.),(1.,1.),(1.,1.),(1.,1.),(1.,1.),(1.,1.),(1.,
1.),(1.,1.),(1.,1.),(1.,1.),(1.,1.),(1.,1.),(1.,1.),(1.,1.),(1.,1.),(1.,
1.),(1.,1.),(1.,1.),(1.,1.),(1.,1.),(1.,1.),(1.,1.),(1.,1.),(1.,1.),(1.,
1.),(1.,1.),(1.,1.),(1.,1.),(1.,1.),(1.,1.),(1.,1.),(1.,1.)))
REPRESENTATION_ITEM('')
SURFACE()
);
#575=(
BOUNDED_SURFACE()
B_SPLINE_SURFACE(5,1,((#58516,#58517),(#58518,#58519),(#58520,#58521),(#58522,
#58523),(#58524,#58525),(#58526,#58527),(#58528,#58529),(#58530,#58531),
(#58532,#58533),(#58534,#58535),(#58536,#58537),(#58538,#58539),(#58540,
#58541),(#58542,#58543),(#58544,#58545),(#58546,#58547),(#58548,#58549),
(#58550,#58551),(#58552,#58553),(#58554,#58555),(#58556,#58557),(#58558,
#58559),(#58560,#58561),(#58562,#58563),(#58564,#58565),(#58566,#58567),
(#58568,#58569),(#58570,#58571),(#58572,#58573),(#58574,#58575),(#58576,
#58577),(#58578,#58579),(#58580,#58581),(#58582,#58583),(#58584,#58585),
(#58586,#58587),(#58588,#58589),(#58590,#58591),(#58592,#58593),(#58594,
#58595)),.UNSPECIFIED.,.F.,.F.,.F.)
B_SPLINE_SURFACE_WITH_KNOTS((6,1,1,1,1,1,1,1,1,1,1,1,1,1,1,1,1,1,1,1,1,
1,1,1,1,1,1,1,1,1,1,1,1,1,1,6),(2,2),(-1.,-0.971428571428572,-0.942857142857143,
-0.914285714285714,-0.885714285714286,-0.857142857142857,-0.828571428571429,
-0.8,-0.771428571428572,-0.742857142857143,-0.714285714285714,-0.685714285714286,
-0.657142857142857,-0.628571428571429,-0.6,-0.571428571428572,-0.542857142857143,
-0.514285714285714,-0.485714285714286,-0.457142857142857,-0.428571428571429,
-0.4,-0.371428571428571,-0.342857142857143,-0.314285714285714,-0.285714285714286,
-0.257142857142857,-0.228571428571429,-0.2,-0.171428571428571,-0.142857142857143,
-0.114285714285714,-0.0857142857142857,-0.0571428571428571,-0.0285714285714286,
0.),(0.,1.6),.UNSPECIFIED.)
GEOMETRIC_REPRESENTATION_ITEM()
RATIONAL_B_SPLINE_SURFACE(((1.,1.),(1.,1.),(1.,1.),(1.,1.),(1.,1.),(1.,
1.),(1.,1.),(1.,1.),(1.,1.),(1.,1.),(1.,1.),(1.,1.),(1.,1.),(1.,1.),(1.,
1.),(1.,1.),(1.,1.),(1.,1.),(1.,1.),(1.,1.),(1.,1.),(1.,1.),(1.,1.),(1.,
1.),(1.,1.),(1.,1.),(1.,1.),(1.,1.),(1.,1.),(1.,1.),(1.,1.),(1.,1.),(1.,
1.),(1.,1.),(1.,1.),(1.,1.),(1.,1.),(1.,1.),(1.,1.),(1.,1.)))
REPRESENTATION_ITEM('')
SURFACE()
);
#576=(
BOUNDED_SURFACE()
B_SPLINE_SURFACE(5,1,((#58615,#58616),(#58617,#58618),(#58619,#58620),(#58621,
#58622),(#58623,#58624),(#58625,#58626),(#58627,#58628),(#58629,#58630),
(#58631,#58632),(#58633,#58634),(#58635,#58636),(#58637,#58638),(#58639,
#58640),(#58641,#58642),(#58643,#58644),(#58645,#58646),(#58647,#58648),
(#58649,#58650),(#58651,#58652),(#58653,#58654),(#58655,#58656),(#58657,
#58658),(#58659,#58660),(#58661,#58662),(#58663,#58664),(#58665,#58666),
(#58667,#58668),(#58669,#58670),(#58671,#58672),(#58673,#58674),(#58675,
#58676),(#58677,#58678),(#58679,#58680),(#58681,#58682),(#58683,#58684),
(#58685,#58686),(#58687,#58688),(#58689,#58690),(#58691,#58692),(#58693,
#58694)),.UNSPECIFIED.,.F.,.F.,.F.)
B_SPLINE_SURFACE_WITH_KNOTS((6,1,1,1,1,1,1,1,1,1,1,1,1,1,1,1,1,1,1,1,1,
1,1,1,1,1,1,1,1,1,1,1,1,1,1,6),(2,2),(-1.,-0.971428571428572,-0.942857142857143,
-0.914285714285714,-0.885714285714286,-0.857142857142857,-0.828571428571429,
-0.8,-0.771428571428572,-0.742857142857143,-0.714285714285714,-0.685714285714286,
-0.657142857142857,-0.628571428571429,-0.6,-0.571428571428572,-0.542857142857143,
-0.514285714285714,-0.485714285714286,-0.457142857142857,-0.428571428571429,
-0.4,-0.371428571428571,-0.342857142857143,-0.314285714285714,-0.285714285714286,
-0.257142857142857,-0.228571428571429,-0.2,-0.171428571428571,-0.142857142857143,
-0.114285714285714,-0.0857142857142857,-0.0571428571428571,-0.0285714285714286,
0.),(0.,1.6),.UNSPECIFIED.)
GEOMETRIC_REPRESENTATION_ITEM()
RATIONAL_B_SPLINE_SURFACE(((1.,1.),(1.,1.),(1.,1.),(1.,1.),(1.,1.),(1.,
1.),(1.,1.),(1.,1.),(1.,1.),(1.,1.),(1.,1.),(1.,1.),(1.,1.),(1.,1.),(1.,
1.),(1.,1.),(1.,1.),(1.,1.),(1.,1.),(1.,1.),(1.,1.),(1.,1.),(1.,1.),(1.,
1.),(1.,1.),(1.,1.),(1.,1.),(1.,1.),(1.,1.),(1.,1.),(1.,1.),(1.,1.),(1.,
1.),(1.,1.),(1.,1.),(1.,1.),(1.,1.),(1.,1.),(1.,1.),(1.,1.)))
REPRESENTATION_ITEM('')
SURFACE()
);
#577=(
BOUNDED_SURFACE()
B_SPLINE_SURFACE(5,1,((#58714,#58715),(#58716,#58717),(#58718,#58719),(#58720,
#58721),(#58722,#58723),(#58724,#58725),(#58726,#58727),(#58728,#58729),
(#58730,#58731),(#58732,#58733),(#58734,#58735),(#58736,#58737),(#58738,
#58739),(#58740,#58741),(#58742,#58743),(#58744,#58745),(#58746,#58747),
(#58748,#58749),(#58750,#58751),(#58752,#58753),(#58754,#58755),(#58756,
#58757),(#58758,#58759),(#58760,#58761),(#58762,#58763),(#58764,#58765),
(#58766,#58767),(#58768,#58769),(#58770,#58771),(#58772,#58773),(#58774,
#58775),(#58776,#58777),(#58778,#58779),(#58780,#58781),(#58782,#58783),
(#58784,#58785),(#58786,#58787),(#58788,#58789),(#58790,#58791),(#58792,
#58793)),.UNSPECIFIED.,.F.,.F.,.F.)
B_SPLINE_SURFACE_WITH_KNOTS((6,1,1,1,1,1,1,1,1,1,1,1,1,1,1,1,1,1,1,1,1,
1,1,1,1,1,1,1,1,1,1,1,1,1,1,6),(2,2),(-1.,-0.971428571428572,-0.942857142857143,
-0.914285714285714,-0.885714285714286,-0.857142857142857,-0.828571428571429,
-0.8,-0.771428571428572,-0.742857142857143,-0.714285714285714,-0.685714285714286,
-0.657142857142857,-0.628571428571429,-0.6,-0.571428571428572,-0.542857142857143,
-0.514285714285714,-0.485714285714286,-0.457142857142857,-0.428571428571429,
-0.4,-0.371428571428571,-0.342857142857143,-0.314285714285714,-0.285714285714286,
-0.257142857142857,-0.228571428571429,-0.2,-0.171428571428571,-0.142857142857143,
-0.114285714285714,-0.0857142857142857,-0.0571428571428571,-0.0285714285714286,
0.),(0.,1.6),.UNSPECIFIED.)
GEOMETRIC_REPRESENTATION_ITEM()
RATIONAL_B_SPLINE_SURFACE(((1.,1.),(1.,1.),(1.,1.),(1.,1.),(1.,1.),(1.,
1.),(1.,1.),(1.,1.),(1.,1.),(1.,1.),(1.,1.),(1.,1.),(1.,1.),(1.,1.),(1.,
1.),(1.,1.),(1.,1.),(1.,1.),(1.,1.),(1.,1.),(1.,1.),(1.,1.),(1.,1.),(1.,
1.),(1.,1.),(1.,1.),(1.,1.),(1.,1.),(1.,1.),(1.,1.),(1.,1.),(1.,1.),(1.,
1.),(1.,1.),(1.,1.),(1.,1.),(1.,1.),(1.,1.),(1.,1.),(1.,1.)))
REPRESENTATION_ITEM('')
SURFACE()
);
#578=(
BOUNDED_SURFACE()
B_SPLINE_SURFACE(5,1,((#58813,#58814),(#58815,#58816),(#58817,#58818),(#58819,
#58820),(#58821,#58822),(#58823,#58824),(#58825,#58826),(#58827,#58828),
(#58829,#58830),(#58831,#58832),(#58833,#58834),(#58835,#58836),(#58837,
#58838),(#58839,#58840),(#58841,#58842),(#58843,#58844),(#58845,#58846),
(#58847,#58848),(#58849,#58850),(#58851,#58852),(#58853,#58854),(#58855,
#58856),(#58857,#58858),(#58859,#58860),(#58861,#58862),(#58863,#58864),
(#58865,#58866),(#58867,#58868),(#58869,#58870),(#58871,#58872),(#58873,
#58874),(#58875,#58876),(#58877,#58878),(#58879,#58880),(#58881,#58882),
(#58883,#58884),(#58885,#58886),(#58887,#58888),(#58889,#58890),(#58891,
#58892)),.UNSPECIFIED.,.F.,.F.,.F.)
B_SPLINE_SURFACE_WITH_KNOTS((6,1,1,1,1,1,1,1,1,1,1,1,1,1,1,1,1,1,1,1,1,
1,1,1,1,1,1,1,1,1,1,1,1,1,1,6),(2,2),(-1.,-0.971428571428572,-0.942857142857143,
-0.914285714285714,-0.885714285714286,-0.857142857142857,-0.828571428571429,
-0.8,-0.771428571428572,-0.742857142857143,-0.714285714285714,-0.685714285714286,
-0.657142857142857,-0.628571428571429,-0.6,-0.571428571428572,-0.542857142857143,
-0.514285714285714,-0.485714285714286,-0.457142857142857,-0.428571428571429,
-0.4,-0.371428571428571,-0.342857142857143,-0.314285714285714,-0.285714285714286,
-0.257142857142857,-0.228571428571429,-0.2,-0.171428571428571,-0.142857142857143,
-0.114285714285714,-0.0857142857142857,-0.0571428571428571,-0.0285714285714286,
0.),(0.,1.6),.UNSPECIFIED.)
GEOMETRIC_REPRESENTATION_ITEM()
RATIONAL_B_SPLINE_SURFACE(((1.,1.),(1.,1.),(1.,1.),(1.,1.),(1.,1.),(1.,
1.),(1.,1.),(1.,1.),(1.,1.),(1.,1.),(1.,1.),(1.,1.),(1.,1.),(1.,1.),(1.,
1.),(1.,1.),(1.,1.),(1.,1.),(1.,1.),(1.,1.),(1.,1.),(1.,1.),(1.,1.),(1.,
1.),(1.,1.),(1.,1.),(1.,1.),(1.,1.),(1.,1.),(1.,1.),(1.,1.),(1.,1.),(1.,
1.),(1.,1.),(1.,1.),(1.,1.),(1.,1.),(1.,1.),(1.,1.),(1.,1.)))
REPRESENTATION_ITEM('')
SURFACE()
);
#579=(
BOUNDED_SURFACE()
B_SPLINE_SURFACE(5,1,((#58912,#58913),(#58914,#58915),(#58916,#58917),(#58918,
#58919),(#58920,#58921),(#58922,#58923),(#58924,#58925),(#58926,#58927),
(#58928,#58929),(#58930,#58931),(#58932,#58933),(#58934,#58935),(#58936,
#58937),(#58938,#58939),(#58940,#58941),(#58942,#58943),(#58944,#58945),
(#58946,#58947),(#58948,#58949),(#58950,#58951),(#58952,#58953),(#58954,
#58955),(#58956,#58957),(#58958,#58959),(#58960,#58961),(#58962,#58963),
(#58964,#58965),(#58966,#58967),(#58968,#58969),(#58970,#58971),(#58972,
#58973),(#58974,#58975),(#58976,#58977),(#58978,#58979),(#58980,#58981),
(#58982,#58983),(#58984,#58985),(#58986,#58987),(#58988,#58989),(#58990,
#58991)),.UNSPECIFIED.,.F.,.F.,.F.)
B_SPLINE_SURFACE_WITH_KNOTS((6,1,1,1,1,1,1,1,1,1,1,1,1,1,1,1,1,1,1,1,1,
1,1,1,1,1,1,1,1,1,1,1,1,1,1,6),(2,2),(-1.,-0.971428571428572,-0.942857142857143,
-0.914285714285714,-0.885714285714286,-0.857142857142857,-0.828571428571429,
-0.8,-0.771428571428572,-0.742857142857143,-0.714285714285714,-0.685714285714286,
-0.657142857142857,-0.628571428571429,-0.6,-0.571428571428572,-0.542857142857143,
-0.514285714285714,-0.485714285714286,-0.457142857142857,-0.428571428571429,
-0.4,-0.371428571428571,-0.342857142857143,-0.314285714285714,-0.285714285714286,
-0.257142857142857,-0.228571428571429,-0.2,-0.171428571428571,-0.142857142857143,
-0.114285714285714,-0.0857142857142857,-0.0571428571428571,-0.0285714285714286,
0.),(0.,1.6),.UNSPECIFIED.)
GEOMETRIC_REPRESENTATION_ITEM()
RATIONAL_B_SPLINE_SURFACE(((1.,1.),(1.,1.),(1.,1.),(1.,1.),(1.,1.),(1.,
1.),(1.,1.),(1.,1.),(1.,1.),(1.,1.),(1.,1.),(1.,1.),(1.,1.),(1.,1.),(1.,
1.),(1.,1.),(1.,1.),(1.,1.),(1.,1.),(1.,1.),(1.,1.),(1.,1.),(1.,1.),(1.,
1.),(1.,1.),(1.,1.),(1.,1.),(1.,1.),(1.,1.),(1.,1.),(1.,1.),(1.,1.),(1.,
1.),(1.,1.),(1.,1.),(1.,1.),(1.,1.),(1.,1.),(1.,1.),(1.,1.)))
REPRESENTATION_ITEM('')
SURFACE()
);
#580=(
BOUNDED_SURFACE()
B_SPLINE_SURFACE(5,1,((#59011,#59012),(#59013,#59014),(#59015,#59016),(#59017,
#59018),(#59019,#59020),(#59021,#59022),(#59023,#59024),(#59025,#59026),
(#59027,#59028),(#59029,#59030),(#59031,#59032),(#59033,#59034),(#59035,
#59036),(#59037,#59038),(#59039,#59040),(#59041,#59042),(#59043,#59044),
(#59045,#59046),(#59047,#59048),(#59049,#59050),(#59051,#59052),(#59053,
#59054),(#59055,#59056),(#59057,#59058),(#59059,#59060),(#59061,#59062),
(#59063,#59064),(#59065,#59066),(#59067,#59068),(#59069,#59070),(#59071,
#59072),(#59073,#59074),(#59075,#59076),(#59077,#59078),(#59079,#59080),
(#59081,#59082),(#59083,#59084),(#59085,#59086),(#59087,#59088),(#59089,
#59090)),.UNSPECIFIED.,.F.,.F.,.F.)
B_SPLINE_SURFACE_WITH_KNOTS((6,1,1,1,1,1,1,1,1,1,1,1,1,1,1,1,1,1,1,1,1,
1,1,1,1,1,1,1,1,1,1,1,1,1,1,6),(2,2),(-1.,-0.971428571428572,-0.942857142857143,
-0.914285714285714,-0.885714285714286,-0.857142857142857,-0.828571428571429,
-0.8,-0.771428571428572,-0.742857142857143,-0.714285714285714,-0.685714285714286,
-0.657142857142857,-0.628571428571429,-0.6,-0.571428571428572,-0.542857142857143,
-0.514285714285714,-0.485714285714286,-0.457142857142857,-0.428571428571429,
-0.4,-0.371428571428571,-0.342857142857143,-0.314285714285714,-0.285714285714286,
-0.257142857142857,-0.228571428571429,-0.2,-0.171428571428571,-0.142857142857143,
-0.114285714285714,-0.0857142857142857,-0.0571428571428571,-0.0285714285714286,
0.),(0.,1.6),.UNSPECIFIED.)
GEOMETRIC_REPRESENTATION_ITEM()
RATIONAL_B_SPLINE_SURFACE(((1.,1.),(1.,1.),(1.,1.),(1.,1.),(1.,1.),(1.,
1.),(1.,1.),(1.,1.),(1.,1.),(1.,1.),(1.,1.),(1.,1.),(1.,1.),(1.,1.),(1.,
1.),(1.,1.),(1.,1.),(1.,1.),(1.,1.),(1.,1.),(1.,1.),(1.,1.),(1.,1.),(1.,
1.),(1.,1.),(1.,1.),(1.,1.),(1.,1.),(1.,1.),(1.,1.),(1.,1.),(1.,1.),(1.,
1.),(1.,1.),(1.,1.),(1.,1.),(1.,1.),(1.,1.),(1.,1.),(1.,1.)))
REPRESENTATION_ITEM('')
SURFACE()
);
#581=(
BOUNDED_SURFACE()
B_SPLINE_SURFACE(5,1,((#59110,#59111),(#59112,#59113),(#59114,#59115),(#59116,
#59117),(#59118,#59119),(#59120,#59121),(#59122,#59123),(#59124,#59125),
(#59126,#59127),(#59128,#59129),(#59130,#59131),(#59132,#59133),(#59134,
#59135),(#59136,#59137),(#59138,#59139),(#59140,#59141),(#59142,#59143),
(#59144,#59145),(#59146,#59147),(#59148,#59149),(#59150,#59151),(#59152,
#59153),(#59154,#59155),(#59156,#59157),(#59158,#59159),(#59160,#59161),
(#59162,#59163),(#59164,#59165),(#59166,#59167),(#59168,#59169),(#59170,
#59171),(#59172,#59173),(#59174,#59175),(#59176,#59177),(#59178,#59179),
(#59180,#59181),(#59182,#59183),(#59184,#59185),(#59186,#59187),(#59188,
#59189)),.UNSPECIFIED.,.F.,.F.,.F.)
B_SPLINE_SURFACE_WITH_KNOTS((6,1,1,1,1,1,1,1,1,1,1,1,1,1,1,1,1,1,1,1,1,
1,1,1,1,1,1,1,1,1,1,1,1,1,1,6),(2,2),(-1.,-0.971428571428572,-0.942857142857143,
-0.914285714285714,-0.885714285714286,-0.857142857142857,-0.828571428571429,
-0.8,-0.771428571428572,-0.742857142857143,-0.714285714285714,-0.685714285714286,
-0.657142857142857,-0.628571428571429,-0.6,-0.571428571428572,-0.542857142857143,
-0.514285714285714,-0.485714285714286,-0.457142857142857,-0.428571428571429,
-0.4,-0.371428571428571,-0.342857142857143,-0.314285714285714,-0.285714285714286,
-0.257142857142857,-0.228571428571429,-0.2,-0.171428571428571,-0.142857142857143,
-0.114285714285714,-0.0857142857142857,-0.0571428571428571,-0.0285714285714286,
0.),(0.,1.6),.UNSPECIFIED.)
GEOMETRIC_REPRESENTATION_ITEM()
RATIONAL_B_SPLINE_SURFACE(((1.,1.),(1.,1.),(1.,1.),(1.,1.),(1.,1.),(1.,
1.),(1.,1.),(1.,1.),(1.,1.),(1.,1.),(1.,1.),(1.,1.),(1.,1.),(1.,1.),(1.,
1.),(1.,1.),(1.,1.),(1.,1.),(1.,1.),(1.,1.),(1.,1.),(1.,1.),(1.,1.),(1.,
1.),(1.,1.),(1.,1.),(1.,1.),(1.,1.),(1.,1.),(1.,1.),(1.,1.),(1.,1.),(1.,
1.),(1.,1.),(1.,1.),(1.,1.),(1.,1.),(1.,1.),(1.,1.),(1.,1.)))
REPRESENTATION_ITEM('')
SURFACE()
);
#582=(
BOUNDED_SURFACE()
B_SPLINE_SURFACE(5,1,((#59221,#59222),(#59223,#59224),(#59225,#59226),(#59227,
#59228),(#59229,#59230),(#59231,#59232),(#59233,#59234),(#59235,#59236),
(#59237,#59238),(#59239,#59240),(#59241,#59242),(#59243,#59244),(#59245,
#59246),(#59247,#59248),(#59249,#59250),(#59251,#59252),(#59253,#59254),
(#59255,#59256),(#59257,#59258),(#59259,#59260),(#59261,#59262),(#59263,
#59264),(#59265,#59266),(#59267,#59268),(#59269,#59270),(#59271,#59272),
(#59273,#59274),(#59275,#59276),(#59277,#59278),(#59279,#59280),(#59281,
#59282),(#59283,#59284),(#59285,#59286),(#59287,#59288),(#59289,#59290),
(#59291,#59292),(#59293,#59294),(#59295,#59296),(#59297,#59298),(#59299,
#59300)),.UNSPECIFIED.,.F.,.F.,.F.)
B_SPLINE_SURFACE_WITH_KNOTS((6,1,1,1,1,1,1,1,1,1,1,1,1,1,1,1,1,1,1,1,1,
1,1,1,1,1,1,1,1,1,1,1,1,1,1,6),(2,2),(-1.,-0.971428571428572,-0.942857142857143,
-0.914285714285714,-0.885714285714286,-0.857142857142857,-0.828571428571429,
-0.8,-0.771428571428572,-0.742857142857143,-0.714285714285714,-0.685714285714286,
-0.657142857142857,-0.628571428571429,-0.6,-0.571428571428572,-0.542857142857143,
-0.514285714285714,-0.485714285714286,-0.457142857142857,-0.428571428571429,
-0.4,-0.371428571428571,-0.342857142857143,-0.314285714285714,-0.285714285714286,
-0.257142857142857,-0.228571428571429,-0.2,-0.171428571428571,-0.142857142857143,
-0.114285714285714,-0.0857142857142857,-0.0571428571428571,-0.0285714285714286,
0.),(0.,1.6),.UNSPECIFIED.)
GEOMETRIC_REPRESENTATION_ITEM()
RATIONAL_B_SPLINE_SURFACE(((1.,1.),(1.,1.),(1.,1.),(1.,1.),(1.,1.),(1.,
1.),(1.,1.),(1.,1.),(1.,1.),(1.,1.),(1.,1.),(1.,1.),(1.,1.),(1.,1.),(1.,
1.),(1.,1.),(1.,1.),(1.,1.),(1.,1.),(1.,1.),(1.,1.),(1.,1.),(1.,1.),(1.,
1.),(1.,1.),(1.,1.),(1.,1.),(1.,1.),(1.,1.),(1.,1.),(1.,1.),(1.,1.),(1.,
1.),(1.,1.),(1.,1.),(1.,1.),(1.,1.),(1.,1.),(1.,1.),(1.,1.)))
REPRESENTATION_ITEM('')
SURFACE()
);
#583=(
BOUNDED_SURFACE()
B_SPLINE_SURFACE(5,1,((#59324,#59325),(#59326,#59327),(#59328,#59329),(#59330,
#59331),(#59332,#59333),(#59334,#59335),(#59336,#59337),(#59338,#59339),
(#59340,#59341),(#59342,#59343),(#59344,#59345),(#59346,#59347),(#59348,
#59349),(#59350,#59351),(#59352,#59353),(#59354,#59355),(#59356,#59357),
(#59358,#59359),(#59360,#59361),(#59362,#59363),(#59364,#59365),(#59366,
#59367),(#59368,#59369),(#59370,#59371),(#59372,#59373),(#59374,#59375),
(#59376,#59377),(#59378,#59379),(#59380,#59381),(#59382,#59383),(#59384,
#59385),(#59386,#59387),(#59388,#59389),(#59390,#59391),(#59392,#59393),
(#59394,#59395),(#59396,#59397),(#59398,#59399),(#59400,#59401),(#59402,
#59403)),.UNSPECIFIED.,.F.,.F.,.F.)
B_SPLINE_SURFACE_WITH_KNOTS((6,1,1,1,1,1,1,1,1,1,1,1,1,1,1,1,1,1,1,1,1,
1,1,1,1,1,1,1,1,1,1,1,1,1,1,6),(2,2),(-1.,-0.971428571428572,-0.942857142857143,
-0.914285714285714,-0.885714285714286,-0.857142857142857,-0.828571428571429,
-0.8,-0.771428571428572,-0.742857142857143,-0.714285714285714,-0.685714285714286,
-0.657142857142857,-0.628571428571429,-0.6,-0.571428571428572,-0.542857142857143,
-0.514285714285714,-0.485714285714286,-0.457142857142857,-0.428571428571429,
-0.4,-0.371428571428571,-0.342857142857143,-0.314285714285714,-0.285714285714286,
-0.257142857142857,-0.228571428571429,-0.2,-0.171428571428571,-0.142857142857143,
-0.114285714285714,-0.0857142857142857,-0.0571428571428571,-0.0285714285714286,
0.),(0.,1.6),.UNSPECIFIED.)
GEOMETRIC_REPRESENTATION_ITEM()
RATIONAL_B_SPLINE_SURFACE(((1.,1.),(1.,1.),(1.,1.),(1.,1.),(1.,1.),(1.,
1.),(1.,1.),(1.,1.),(1.,1.),(1.,1.),(1.,1.),(1.,1.),(1.,1.),(1.,1.),(1.,
1.),(1.,1.),(1.,1.),(1.,1.),(1.,1.),(1.,1.),(1.,1.),(1.,1.),(1.,1.),(1.,
1.),(1.,1.),(1.,1.),(1.,1.),(1.,1.),(1.,1.),(1.,1.),(1.,1.),(1.,1.),(1.,
1.),(1.,1.),(1.,1.),(1.,1.),(1.,1.),(1.,1.),(1.,1.),(1.,1.)))
REPRESENTATION_ITEM('')
SURFACE()
);
#584=(
BOUNDED_SURFACE()
B_SPLINE_SURFACE(5,1,((#59435,#59436),(#59437,#59438),(#59439,#59440),(#59441,
#59442),(#59443,#59444),(#59445,#59446),(#59447,#59448),(#59449,#59450),
(#59451,#59452),(#59453,#59454),(#59455,#59456),(#59457,#59458),(#59459,
#59460),(#59461,#59462),(#59463,#59464),(#59465,#59466),(#59467,#59468),
(#59469,#59470),(#59471,#59472),(#59473,#59474),(#59475,#59476),(#59477,
#59478),(#59479,#59480),(#59481,#59482),(#59483,#59484),(#59485,#59486),
(#59487,#59488),(#59489,#59490),(#59491,#59492),(#59493,#59494),(#59495,
#59496),(#59497,#59498),(#59499,#59500),(#59501,#59502),(#59503,#59504),
(#59505,#59506),(#59507,#59508),(#59509,#59510),(#59511,#59512),(#59513,
#59514)),.UNSPECIFIED.,.F.,.F.,.F.)
B_SPLINE_SURFACE_WITH_KNOTS((6,1,1,1,1,1,1,1,1,1,1,1,1,1,1,1,1,1,1,1,1,
1,1,1,1,1,1,1,1,1,1,1,1,1,1,6),(2,2),(-1.,-0.971428571428572,-0.942857142857143,
-0.914285714285714,-0.885714285714286,-0.857142857142857,-0.828571428571429,
-0.8,-0.771428571428572,-0.742857142857143,-0.714285714285714,-0.685714285714286,
-0.657142857142857,-0.628571428571429,-0.6,-0.571428571428572,-0.542857142857143,
-0.514285714285714,-0.485714285714286,-0.457142857142857,-0.428571428571429,
-0.4,-0.371428571428571,-0.342857142857143,-0.314285714285714,-0.285714285714286,
-0.257142857142857,-0.228571428571429,-0.2,-0.171428571428571,-0.142857142857143,
-0.114285714285714,-0.0857142857142857,-0.0571428571428571,-0.0285714285714286,
0.),(0.,1.6),.UNSPECIFIED.)
GEOMETRIC_REPRESENTATION_ITEM()
RATIONAL_B_SPLINE_SURFACE(((1.,1.),(1.,1.),(1.,1.),(1.,1.),(1.,1.),(1.,
1.),(1.,1.),(1.,1.),(1.,1.),(1.,1.),(1.,1.),(1.,1.),(1.,1.),(1.,1.),(1.,
1.),(1.,1.),(1.,1.),(1.,1.),(1.,1.),(1.,1.),(1.,1.),(1.,1.),(1.,1.),(1.,
1.),(1.,1.),(1.,1.),(1.,1.),(1.,1.),(1.,1.),(1.,1.),(1.,1.),(1.,1.),(1.,
1.),(1.,1.),(1.,1.),(1.,1.),(1.,1.),(1.,1.),(1.,1.),(1.,1.)))
REPRESENTATION_ITEM('')
SURFACE()
);
#585=(
BOUNDED_SURFACE()
B_SPLINE_SURFACE(5,1,((#59534,#59535),(#59536,#59537),(#59538,#59539),(#59540,
#59541),(#59542,#59543),(#59544,#59545),(#59546,#59547),(#59548,#59549),
(#59550,#59551),(#59552,#59553),(#59554,#59555),(#59556,#59557),(#59558,
#59559),(#59560,#59561),(#59562,#59563),(#59564,#59565),(#59566,#59567),
(#59568,#59569),(#59570,#59571),(#59572,#59573),(#59574,#59575),(#59576,
#59577),(#59578,#59579),(#59580,#59581),(#59582,#59583),(#59584,#59585),
(#59586,#59587),(#59588,#59589),(#59590,#59591),(#59592,#59593),(#59594,
#59595),(#59596,#59597),(#59598,#59599),(#59600,#59601),(#59602,#59603),
(#59604,#59605),(#59606,#59607),(#59608,#59609),(#59610,#59611),(#59612,
#59613)),.UNSPECIFIED.,.F.,.F.,.F.)
B_SPLINE_SURFACE_WITH_KNOTS((6,1,1,1,1,1,1,1,1,1,1,1,1,1,1,1,1,1,1,1,1,
1,1,1,1,1,1,1,1,1,1,1,1,1,1,6),(2,2),(-1.,-0.971428571428572,-0.942857142857143,
-0.914285714285714,-0.885714285714286,-0.857142857142857,-0.828571428571429,
-0.8,-0.771428571428572,-0.742857142857143,-0.714285714285714,-0.685714285714286,
-0.657142857142857,-0.628571428571429,-0.6,-0.571428571428572,-0.542857142857143,
-0.514285714285714,-0.485714285714286,-0.457142857142857,-0.428571428571429,
-0.4,-0.371428571428571,-0.342857142857143,-0.314285714285714,-0.285714285714286,
-0.257142857142857,-0.228571428571429,-0.2,-0.171428571428571,-0.142857142857143,
-0.114285714285714,-0.0857142857142857,-0.0571428571428571,-0.0285714285714286,
0.),(0.,1.6),.UNSPECIFIED.)
GEOMETRIC_REPRESENTATION_ITEM()
RATIONAL_B_SPLINE_SURFACE(((1.,1.),(1.,1.),(1.,1.),(1.,1.),(1.,1.),(1.,
1.),(1.,1.),(1.,1.),(1.,1.),(1.,1.),(1.,1.),(1.,1.),(1.,1.),(1.,1.),(1.,
1.),(1.,1.),(1.,1.),(1.,1.),(1.,1.),(1.,1.),(1.,1.),(1.,1.),(1.,1.),(1.,
1.),(1.,1.),(1.,1.),(1.,1.),(1.,1.),(1.,1.),(1.,1.),(1.,1.),(1.,1.),(1.,
1.),(1.,1.),(1.,1.),(1.,1.),(1.,1.),(1.,1.),(1.,1.),(1.,1.)))
REPRESENTATION_ITEM('')
SURFACE()
);
#586=(
BOUNDED_SURFACE()
B_SPLINE_SURFACE(5,1,((#59633,#59634),(#59635,#59636),(#59637,#59638),(#59639,
#59640),(#59641,#59642),(#59643,#59644),(#59645,#59646),(#59647,#59648),
(#59649,#59650),(#59651,#59652),(#59653,#59654),(#59655,#59656),(#59657,
#59658),(#59659,#59660),(#59661,#59662),(#59663,#59664),(#59665,#59666),
(#59667,#59668),(#59669,#59670),(#59671,#59672),(#59673,#59674),(#59675,
#59676),(#59677,#59678),(#59679,#59680),(#59681,#59682),(#59683,#59684),
(#59685,#59686),(#59687,#59688),(#59689,#59690),(#59691,#59692),(#59693,
#59694),(#59695,#59696),(#59697,#59698),(#59699,#59700),(#59701,#59702),
(#59703,#59704),(#59705,#59706),(#59707,#59708),(#59709,#59710),(#59711,
#59712)),.UNSPECIFIED.,.F.,.F.,.F.)
B_SPLINE_SURFACE_WITH_KNOTS((6,1,1,1,1,1,1,1,1,1,1,1,1,1,1,1,1,1,1,1,1,
1,1,1,1,1,1,1,1,1,1,1,1,1,1,6),(2,2),(-1.,-0.971428571428572,-0.942857142857143,
-0.914285714285714,-0.885714285714286,-0.857142857142857,-0.828571428571429,
-0.8,-0.771428571428572,-0.742857142857143,-0.714285714285714,-0.685714285714286,
-0.657142857142857,-0.628571428571429,-0.6,-0.571428571428572,-0.542857142857143,
-0.514285714285714,-0.485714285714286,-0.457142857142857,-0.428571428571429,
-0.4,-0.371428571428571,-0.342857142857143,-0.314285714285714,-0.285714285714286,
-0.257142857142857,-0.228571428571429,-0.2,-0.171428571428571,-0.142857142857143,
-0.114285714285714,-0.0857142857142857,-0.0571428571428571,-0.0285714285714286,
0.),(0.,1.6),.UNSPECIFIED.)
GEOMETRIC_REPRESENTATION_ITEM()
RATIONAL_B_SPLINE_SURFACE(((1.,1.),(1.,1.),(1.,1.),(1.,1.),(1.,1.),(1.,
1.),(1.,1.),(1.,1.),(1.,1.),(1.,1.),(1.,1.),(1.,1.),(1.,1.),(1.,1.),(1.,
1.),(1.,1.),(1.,1.),(1.,1.),(1.,1.),(1.,1.),(1.,1.),(1.,1.),(1.,1.),(1.,
1.),(1.,1.),(1.,1.),(1.,1.),(1.,1.),(1.,1.),(1.,1.),(1.,1.),(1.,1.),(1.,
1.),(1.,1.),(1.,1.),(1.,1.),(1.,1.),(1.,1.),(1.,1.),(1.,1.)))
REPRESENTATION_ITEM('')
SURFACE()
);
#587=(
BOUNDED_SURFACE()
B_SPLINE_SURFACE(5,1,((#59732,#59733),(#59734,#59735),(#59736,#59737),(#59738,
#59739),(#59740,#59741),(#59742,#59743),(#59744,#59745),(#59746,#59747),
(#59748,#59749),(#59750,#59751),(#59752,#59753),(#59754,#59755),(#59756,
#59757),(#59758,#59759),(#59760,#59761),(#59762,#59763),(#59764,#59765),
(#59766,#59767),(#59768,#59769),(#59770,#59771),(#59772,#59773),(#59774,
#59775),(#59776,#59777),(#59778,#59779),(#59780,#59781),(#59782,#59783),
(#59784,#59785),(#59786,#59787),(#59788,#59789),(#59790,#59791),(#59792,
#59793),(#59794,#59795),(#59796,#59797),(#59798,#59799),(#59800,#59801),
(#59802,#59803),(#59804,#59805),(#59806,#59807),(#59808,#59809),(#59810,
#59811)),.UNSPECIFIED.,.F.,.F.,.F.)
B_SPLINE_SURFACE_WITH_KNOTS((6,1,1,1,1,1,1,1,1,1,1,1,1,1,1,1,1,1,1,1,1,
1,1,1,1,1,1,1,1,1,1,1,1,1,1,6),(2,2),(-1.,-0.971428571428572,-0.942857142857143,
-0.914285714285714,-0.885714285714286,-0.857142857142857,-0.828571428571429,
-0.8,-0.771428571428572,-0.742857142857143,-0.714285714285714,-0.685714285714286,
-0.657142857142857,-0.628571428571429,-0.6,-0.571428571428572,-0.542857142857143,
-0.514285714285714,-0.485714285714286,-0.457142857142857,-0.428571428571429,
-0.4,-0.371428571428571,-0.342857142857143,-0.314285714285714,-0.285714285714286,
-0.257142857142857,-0.228571428571429,-0.2,-0.171428571428571,-0.142857142857143,
-0.114285714285714,-0.0857142857142857,-0.0571428571428571,-0.0285714285714286,
0.),(0.,1.6),.UNSPECIFIED.)
GEOMETRIC_REPRESENTATION_ITEM()
RATIONAL_B_SPLINE_SURFACE(((1.,1.),(1.,1.),(1.,1.),(1.,1.),(1.,1.),(1.,
1.),(1.,1.),(1.,1.),(1.,1.),(1.,1.),(1.,1.),(1.,1.),(1.,1.),(1.,1.),(1.,
1.),(1.,1.),(1.,1.),(1.,1.),(1.,1.),(1.,1.),(1.,1.),(1.,1.),(1.,1.),(1.,
1.),(1.,1.),(1.,1.),(1.,1.),(1.,1.),(1.,1.),(1.,1.),(1.,1.),(1.,1.),(1.,
1.),(1.,1.),(1.,1.),(1.,1.),(1.,1.),(1.,1.),(1.,1.),(1.,1.)))
REPRESENTATION_ITEM('')
SURFACE()
);
#588=(
BOUNDED_SURFACE()
B_SPLINE_SURFACE(5,1,((#59831,#59832),(#59833,#59834),(#59835,#59836),(#59837,
#59838),(#59839,#59840),(#59841,#59842),(#59843,#59844),(#59845,#59846),
(#59847,#59848),(#59849,#59850),(#59851,#59852),(#59853,#59854),(#59855,
#59856),(#59857,#59858),(#59859,#59860),(#59861,#59862),(#59863,#59864),
(#59865,#59866),(#59867,#59868),(#59869,#59870),(#59871,#59872),(#59873,
#59874),(#59875,#59876),(#59877,#59878),(#59879,#59880),(#59881,#59882),
(#59883,#59884),(#59885,#59886),(#59887,#59888),(#59889,#59890),(#59891,
#59892),(#59893,#59894),(#59895,#59896),(#59897,#59898),(#59899,#59900),
(#59901,#59902),(#59903,#59904),(#59905,#59906),(#59907,#59908),(#59909,
#59910)),.UNSPECIFIED.,.F.,.F.,.F.)
B_SPLINE_SURFACE_WITH_KNOTS((6,1,1,1,1,1,1,1,1,1,1,1,1,1,1,1,1,1,1,1,1,
1,1,1,1,1,1,1,1,1,1,1,1,1,1,6),(2,2),(-1.,-0.971428571428572,-0.942857142857143,
-0.914285714285714,-0.885714285714286,-0.857142857142857,-0.828571428571429,
-0.8,-0.771428571428572,-0.742857142857143,-0.714285714285714,-0.685714285714286,
-0.657142857142857,-0.628571428571429,-0.6,-0.571428571428572,-0.542857142857143,
-0.514285714285714,-0.485714285714286,-0.457142857142857,-0.428571428571429,
-0.4,-0.371428571428571,-0.342857142857143,-0.314285714285714,-0.285714285714286,
-0.257142857142857,-0.228571428571429,-0.2,-0.171428571428571,-0.142857142857143,
-0.114285714285714,-0.0857142857142857,-0.0571428571428571,-0.0285714285714286,
0.),(0.,1.6),.UNSPECIFIED.)
GEOMETRIC_REPRESENTATION_ITEM()
RATIONAL_B_SPLINE_SURFACE(((1.,1.),(1.,1.),(1.,1.),(1.,1.),(1.,1.),(1.,
1.),(1.,1.),(1.,1.),(1.,1.),(1.,1.),(1.,1.),(1.,1.),(1.,1.),(1.,1.),(1.,
1.),(1.,1.),(1.,1.),(1.,1.),(1.,1.),(1.,1.),(1.,1.),(1.,1.),(1.,1.),(1.,
1.),(1.,1.),(1.,1.),(1.,1.),(1.,1.),(1.,1.),(1.,1.),(1.,1.),(1.,1.),(1.,
1.),(1.,1.),(1.,1.),(1.,1.),(1.,1.),(1.,1.),(1.,1.),(1.,1.)))
REPRESENTATION_ITEM('')
SURFACE()
);
#589=(
BOUNDED_SURFACE()
B_SPLINE_SURFACE(5,1,((#59930,#59931),(#59932,#59933),(#59934,#59935),(#59936,
#59937),(#59938,#59939),(#59940,#59941),(#59942,#59943),(#59944,#59945),
(#59946,#59947),(#59948,#59949),(#59950,#59951),(#59952,#59953),(#59954,
#59955),(#59956,#59957),(#59958,#59959),(#59960,#59961),(#59962,#59963),
(#59964,#59965),(#59966,#59967),(#59968,#59969),(#59970,#59971),(#59972,
#59973),(#59974,#59975),(#59976,#59977),(#59978,#59979),(#59980,#59981),
(#59982,#59983),(#59984,#59985),(#59986,#59987),(#59988,#59989),(#59990,
#59991),(#59992,#59993),(#59994,#59995),(#59996,#59997),(#59998,#59999),
(#60000,#60001),(#60002,#60003),(#60004,#60005),(#60006,#60007),(#60008,
#60009)),.UNSPECIFIED.,.F.,.F.,.F.)
B_SPLINE_SURFACE_WITH_KNOTS((6,1,1,1,1,1,1,1,1,1,1,1,1,1,1,1,1,1,1,1,1,
1,1,1,1,1,1,1,1,1,1,1,1,1,1,6),(2,2),(-1.,-0.971428571428572,-0.942857142857143,
-0.914285714285714,-0.885714285714286,-0.857142857142857,-0.828571428571429,
-0.8,-0.771428571428572,-0.742857142857143,-0.714285714285714,-0.685714285714286,
-0.657142857142857,-0.628571428571429,-0.6,-0.571428571428572,-0.542857142857143,
-0.514285714285714,-0.485714285714286,-0.457142857142857,-0.428571428571429,
-0.4,-0.371428571428571,-0.342857142857143,-0.314285714285714,-0.285714285714286,
-0.257142857142857,-0.228571428571429,-0.2,-0.171428571428571,-0.142857142857143,
-0.114285714285714,-0.0857142857142857,-0.0571428571428571,-0.0285714285714286,
0.),(0.,1.6),.UNSPECIFIED.)
GEOMETRIC_REPRESENTATION_ITEM()
RATIONAL_B_SPLINE_SURFACE(((1.,1.),(1.,1.),(1.,1.),(1.,1.),(1.,1.),(1.,
1.),(1.,1.),(1.,1.),(1.,1.),(1.,1.),(1.,1.),(1.,1.),(1.,1.),(1.,1.),(1.,
1.),(1.,1.),(1.,1.),(1.,1.),(1.,1.),(1.,1.),(1.,1.),(1.,1.),(1.,1.),(1.,
1.),(1.,1.),(1.,1.),(1.,1.),(1.,1.),(1.,1.),(1.,1.),(1.,1.),(1.,1.),(1.,
1.),(1.,1.),(1.,1.),(1.,1.),(1.,1.),(1.,1.),(1.,1.),(1.,1.)))
REPRESENTATION_ITEM('')
SURFACE()
);
#590=(
BOUNDED_SURFACE()
B_SPLINE_SURFACE(5,1,((#60029,#60030),(#60031,#60032),(#60033,#60034),(#60035,
#60036),(#60037,#60038),(#60039,#60040),(#60041,#60042),(#60043,#60044),
(#60045,#60046),(#60047,#60048),(#60049,#60050),(#60051,#60052),(#60053,
#60054),(#60055,#60056),(#60057,#60058),(#60059,#60060),(#60061,#60062),
(#60063,#60064),(#60065,#60066),(#60067,#60068),(#60069,#60070),(#60071,
#60072),(#60073,#60074),(#60075,#60076),(#60077,#60078),(#60079,#60080),
(#60081,#60082),(#60083,#60084),(#60085,#60086),(#60087,#60088),(#60089,
#60090),(#60091,#60092),(#60093,#60094),(#60095,#60096),(#60097,#60098),
(#60099,#60100),(#60101,#60102),(#60103,#60104),(#60105,#60106),(#60107,
#60108)),.UNSPECIFIED.,.F.,.F.,.F.)
B_SPLINE_SURFACE_WITH_KNOTS((6,1,1,1,1,1,1,1,1,1,1,1,1,1,1,1,1,1,1,1,1,
1,1,1,1,1,1,1,1,1,1,1,1,1,1,6),(2,2),(-1.,-0.971428571428572,-0.942857142857143,
-0.914285714285714,-0.885714285714286,-0.857142857142857,-0.828571428571429,
-0.8,-0.771428571428572,-0.742857142857143,-0.714285714285714,-0.685714285714286,
-0.657142857142857,-0.628571428571429,-0.6,-0.571428571428572,-0.542857142857143,
-0.514285714285714,-0.485714285714286,-0.457142857142857,-0.428571428571429,
-0.4,-0.371428571428571,-0.342857142857143,-0.314285714285714,-0.285714285714286,
-0.257142857142857,-0.228571428571429,-0.2,-0.171428571428571,-0.142857142857143,
-0.114285714285714,-0.0857142857142857,-0.0571428571428571,-0.0285714285714286,
0.),(0.,1.6),.UNSPECIFIED.)
GEOMETRIC_REPRESENTATION_ITEM()
RATIONAL_B_SPLINE_SURFACE(((1.,1.),(1.,1.),(1.,1.),(1.,1.),(1.,1.),(1.,
1.),(1.,1.),(1.,1.),(1.,1.),(1.,1.),(1.,1.),(1.,1.),(1.,1.),(1.,1.),(1.,
1.),(1.,1.),(1.,1.),(1.,1.),(1.,1.),(1.,1.),(1.,1.),(1.,1.),(1.,1.),(1.,
1.),(1.,1.),(1.,1.),(1.,1.),(1.,1.),(1.,1.),(1.,1.),(1.,1.),(1.,1.),(1.,
1.),(1.,1.),(1.,1.),(1.,1.),(1.,1.),(1.,1.),(1.,1.),(1.,1.)))
REPRESENTATION_ITEM('')
SURFACE()
);
#591=(
BOUNDED_SURFACE()
B_SPLINE_SURFACE(5,1,((#60128,#60129),(#60130,#60131),(#60132,#60133),(#60134,
#60135),(#60136,#60137),(#60138,#60139),(#60140,#60141),(#60142,#60143),
(#60144,#60145),(#60146,#60147),(#60148,#60149),(#60150,#60151),(#60152,
#60153),(#60154,#60155),(#60156,#60157),(#60158,#60159),(#60160,#60161),
(#60162,#60163),(#60164,#60165),(#60166,#60167),(#60168,#60169),(#60170,
#60171),(#60172,#60173),(#60174,#60175),(#60176,#60177),(#60178,#60179),
(#60180,#60181),(#60182,#60183),(#60184,#60185),(#60186,#60187),(#60188,
#60189),(#60190,#60191),(#60192,#60193),(#60194,#60195),(#60196,#60197),
(#60198,#60199),(#60200,#60201),(#60202,#60203),(#60204,#60205),(#60206,
#60207)),.UNSPECIFIED.,.F.,.F.,.F.)
B_SPLINE_SURFACE_WITH_KNOTS((6,1,1,1,1,1,1,1,1,1,1,1,1,1,1,1,1,1,1,1,1,
1,1,1,1,1,1,1,1,1,1,1,1,1,1,6),(2,2),(-1.,-0.971428571428572,-0.942857142857143,
-0.914285714285714,-0.885714285714286,-0.857142857142857,-0.828571428571429,
-0.8,-0.771428571428572,-0.742857142857143,-0.714285714285714,-0.685714285714286,
-0.657142857142857,-0.628571428571429,-0.6,-0.571428571428572,-0.542857142857143,
-0.514285714285714,-0.485714285714286,-0.457142857142857,-0.428571428571429,
-0.4,-0.371428571428571,-0.342857142857143,-0.314285714285714,-0.285714285714286,
-0.257142857142857,-0.228571428571429,-0.2,-0.171428571428571,-0.142857142857143,
-0.114285714285714,-0.0857142857142857,-0.0571428571428571,-0.0285714285714286,
0.),(0.,1.6),.UNSPECIFIED.)
GEOMETRIC_REPRESENTATION_ITEM()
RATIONAL_B_SPLINE_SURFACE(((1.,1.),(1.,1.),(1.,1.),(1.,1.),(1.,1.),(1.,
1.),(1.,1.),(1.,1.),(1.,1.),(1.,1.),(1.,1.),(1.,1.),(1.,1.),(1.,1.),(1.,
1.),(1.,1.),(1.,1.),(1.,1.),(1.,1.),(1.,1.),(1.,1.),(1.,1.),(1.,1.),(1.,
1.),(1.,1.),(1.,1.),(1.,1.),(1.,1.),(1.,1.),(1.,1.),(1.,1.),(1.,1.),(1.,
1.),(1.,1.),(1.,1.),(1.,1.),(1.,1.),(1.,1.),(1.,1.),(1.,1.)))
REPRESENTATION_ITEM('')
SURFACE()
);
#592=(
BOUNDED_SURFACE()
B_SPLINE_SURFACE(5,1,((#60227,#60228),(#60229,#60230),(#60231,#60232),(#60233,
#60234),(#60235,#60236),(#60237,#60238),(#60239,#60240),(#60241,#60242),
(#60243,#60244),(#60245,#60246),(#60247,#60248),(#60249,#60250),(#60251,
#60252),(#60253,#60254),(#60255,#60256),(#60257,#60258),(#60259,#60260),
(#60261,#60262),(#60263,#60264),(#60265,#60266),(#60267,#60268),(#60269,
#60270),(#60271,#60272),(#60273,#60274),(#60275,#60276),(#60277,#60278),
(#60279,#60280),(#60281,#60282),(#60283,#60284),(#60285,#60286),(#60287,
#60288),(#60289,#60290),(#60291,#60292),(#60293,#60294),(#60295,#60296),
(#60297,#60298),(#60299,#60300),(#60301,#60302),(#60303,#60304),(#60305,
#60306)),.UNSPECIFIED.,.F.,.F.,.F.)
B_SPLINE_SURFACE_WITH_KNOTS((6,1,1,1,1,1,1,1,1,1,1,1,1,1,1,1,1,1,1,1,1,
1,1,1,1,1,1,1,1,1,1,1,1,1,1,6),(2,2),(-1.,-0.971428571428572,-0.942857142857143,
-0.914285714285714,-0.885714285714286,-0.857142857142857,-0.828571428571429,
-0.8,-0.771428571428572,-0.742857142857143,-0.714285714285714,-0.685714285714286,
-0.657142857142857,-0.628571428571429,-0.6,-0.571428571428572,-0.542857142857143,
-0.514285714285714,-0.485714285714286,-0.457142857142857,-0.428571428571429,
-0.4,-0.371428571428571,-0.342857142857143,-0.314285714285714,-0.285714285714286,
-0.257142857142857,-0.228571428571429,-0.2,-0.171428571428571,-0.142857142857143,
-0.114285714285714,-0.0857142857142857,-0.0571428571428571,-0.0285714285714286,
0.),(0.,1.6),.UNSPECIFIED.)
GEOMETRIC_REPRESENTATION_ITEM()
RATIONAL_B_SPLINE_SURFACE(((1.,1.),(1.,1.),(1.,1.),(1.,1.),(1.,1.),(1.,
1.),(1.,1.),(1.,1.),(1.,1.),(1.,1.),(1.,1.),(1.,1.),(1.,1.),(1.,1.),(1.,
1.),(1.,1.),(1.,1.),(1.,1.),(1.,1.),(1.,1.),(1.,1.),(1.,1.),(1.,1.),(1.,
1.),(1.,1.),(1.,1.),(1.,1.),(1.,1.),(1.,1.),(1.,1.),(1.,1.),(1.,1.),(1.,
1.),(1.,1.),(1.,1.),(1.,1.),(1.,1.),(1.,1.),(1.,1.),(1.,1.)))
REPRESENTATION_ITEM('')
SURFACE()
);
#593=(
BOUNDED_SURFACE()
B_SPLINE_SURFACE(5,1,((#60326,#60327),(#60328,#60329),(#60330,#60331),(#60332,
#60333),(#60334,#60335),(#60336,#60337),(#60338,#60339),(#60340,#60341),
(#60342,#60343),(#60344,#60345),(#60346,#60347),(#60348,#60349),(#60350,
#60351),(#60352,#60353),(#60354,#60355),(#60356,#60357),(#60358,#60359),
(#60360,#60361),(#60362,#60363),(#60364,#60365),(#60366,#60367),(#60368,
#60369),(#60370,#60371),(#60372,#60373),(#60374,#60375),(#60376,#60377),
(#60378,#60379),(#60380,#60381),(#60382,#60383),(#60384,#60385),(#60386,
#60387),(#60388,#60389),(#60390,#60391),(#60392,#60393),(#60394,#60395),
(#60396,#60397),(#60398,#60399),(#60400,#60401),(#60402,#60403),(#60404,
#60405)),.UNSPECIFIED.,.F.,.F.,.F.)
B_SPLINE_SURFACE_WITH_KNOTS((6,1,1,1,1,1,1,1,1,1,1,1,1,1,1,1,1,1,1,1,1,
1,1,1,1,1,1,1,1,1,1,1,1,1,1,6),(2,2),(-1.,-0.971428571428572,-0.942857142857143,
-0.914285714285714,-0.885714285714286,-0.857142857142857,-0.828571428571429,
-0.8,-0.771428571428572,-0.742857142857143,-0.714285714285714,-0.685714285714286,
-0.657142857142857,-0.628571428571429,-0.6,-0.571428571428572,-0.542857142857143,
-0.514285714285714,-0.485714285714286,-0.457142857142857,-0.428571428571429,
-0.4,-0.371428571428571,-0.342857142857143,-0.314285714285714,-0.285714285714286,
-0.257142857142857,-0.228571428571429,-0.2,-0.171428571428571,-0.142857142857143,
-0.114285714285714,-0.0857142857142857,-0.0571428571428571,-0.0285714285714286,
0.),(0.,1.6),.UNSPECIFIED.)
GEOMETRIC_REPRESENTATION_ITEM()
RATIONAL_B_SPLINE_SURFACE(((1.,1.),(1.,1.),(1.,1.),(1.,1.),(1.,1.),(1.,
1.),(1.,1.),(1.,1.),(1.,1.),(1.,1.),(1.,1.),(1.,1.),(1.,1.),(1.,1.),(1.,
1.),(1.,1.),(1.,1.),(1.,1.),(1.,1.),(1.,1.),(1.,1.),(1.,1.),(1.,1.),(1.,
1.),(1.,1.),(1.,1.),(1.,1.),(1.,1.),(1.,1.),(1.,1.),(1.,1.),(1.,1.),(1.,
1.),(1.,1.),(1.,1.),(1.,1.),(1.,1.),(1.,1.),(1.,1.),(1.,1.)))
REPRESENTATION_ITEM('')
SURFACE()
);
#594=(
BOUNDED_SURFACE()
B_SPLINE_SURFACE(5,1,((#60437,#60438),(#60439,#60440),(#60441,#60442),(#60443,
#60444),(#60445,#60446),(#60447,#60448),(#60449,#60450),(#60451,#60452),
(#60453,#60454),(#60455,#60456),(#60457,#60458),(#60459,#60460),(#60461,
#60462),(#60463,#60464),(#60465,#60466),(#60467,#60468),(#60469,#60470),
(#60471,#60472),(#60473,#60474),(#60475,#60476),(#60477,#60478),(#60479,
#60480),(#60481,#60482),(#60483,#60484),(#60485,#60486),(#60487,#60488),
(#60489,#60490),(#60491,#60492),(#60493,#60494),(#60495,#60496),(#60497,
#60498),(#60499,#60500),(#60501,#60502),(#60503,#60504),(#60505,#60506),
(#60507,#60508),(#60509,#60510),(#60511,#60512),(#60513,#60514),(#60515,
#60516)),.UNSPECIFIED.,.F.,.F.,.F.)
B_SPLINE_SURFACE_WITH_KNOTS((6,1,1,1,1,1,1,1,1,1,1,1,1,1,1,1,1,1,1,1,1,
1,1,1,1,1,1,1,1,1,1,1,1,1,1,6),(2,2),(-1.,-0.971428571428572,-0.942857142857143,
-0.914285714285714,-0.885714285714286,-0.857142857142857,-0.828571428571429,
-0.8,-0.771428571428572,-0.742857142857143,-0.714285714285714,-0.685714285714286,
-0.657142857142857,-0.628571428571429,-0.6,-0.571428571428572,-0.542857142857143,
-0.514285714285714,-0.485714285714286,-0.457142857142857,-0.428571428571429,
-0.4,-0.371428571428571,-0.342857142857143,-0.314285714285714,-0.285714285714286,
-0.257142857142857,-0.228571428571429,-0.2,-0.171428571428571,-0.142857142857143,
-0.114285714285714,-0.0857142857142857,-0.0571428571428571,-0.0285714285714286,
0.),(0.,1.6),.UNSPECIFIED.)
GEOMETRIC_REPRESENTATION_ITEM()
RATIONAL_B_SPLINE_SURFACE(((1.,1.),(1.,1.),(1.,1.),(1.,1.),(1.,1.),(1.,
1.),(1.,1.),(1.,1.),(1.,1.),(1.,1.),(1.,1.),(1.,1.),(1.,1.),(1.,1.),(1.,
1.),(1.,1.),(1.,1.),(1.,1.),(1.,1.),(1.,1.),(1.,1.),(1.,1.),(1.,1.),(1.,
1.),(1.,1.),(1.,1.),(1.,1.),(1.,1.),(1.,1.),(1.,1.),(1.,1.),(1.,1.),(1.,
1.),(1.,1.),(1.,1.),(1.,1.),(1.,1.),(1.,1.),(1.,1.),(1.,1.)))
REPRESENTATION_ITEM('')
SURFACE()
);
#595=(
BOUNDED_SURFACE()
B_SPLINE_SURFACE(5,1,((#60538,#60539),(#60540,#60541),(#60542,#60543),(#60544,
#60545),(#60546,#60547),(#60548,#60549),(#60550,#60551),(#60552,#60553),
(#60554,#60555),(#60556,#60557),(#60558,#60559),(#60560,#60561),(#60562,
#60563),(#60564,#60565),(#60566,#60567),(#60568,#60569),(#60570,#60571),
(#60572,#60573),(#60574,#60575),(#60576,#60577),(#60578,#60579),(#60580,
#60581),(#60582,#60583),(#60584,#60585),(#60586,#60587),(#60588,#60589),
(#60590,#60591),(#60592,#60593),(#60594,#60595),(#60596,#60597),(#60598,
#60599),(#60600,#60601),(#60602,#60603),(#60604,#60605),(#60606,#60607),
(#60608,#60609),(#60610,#60611),(#60612,#60613),(#60614,#60615),(#60616,
#60617)),.UNSPECIFIED.,.F.,.F.,.F.)
B_SPLINE_SURFACE_WITH_KNOTS((6,1,1,1,1,1,1,1,1,1,1,1,1,1,1,1,1,1,1,1,1,
1,1,1,1,1,1,1,1,1,1,1,1,1,1,6),(2,2),(-1.,-0.971428571428572,-0.942857142857143,
-0.914285714285714,-0.885714285714286,-0.857142857142857,-0.828571428571429,
-0.8,-0.771428571428572,-0.742857142857143,-0.714285714285714,-0.685714285714286,
-0.657142857142857,-0.628571428571429,-0.6,-0.571428571428572,-0.542857142857143,
-0.514285714285714,-0.485714285714286,-0.457142857142857,-0.428571428571429,
-0.4,-0.371428571428571,-0.342857142857143,-0.314285714285714,-0.285714285714286,
-0.257142857142857,-0.228571428571429,-0.2,-0.171428571428571,-0.142857142857143,
-0.114285714285714,-0.0857142857142857,-0.0571428571428571,-0.0285714285714286,
0.),(0.,1.6),.UNSPECIFIED.)
GEOMETRIC_REPRESENTATION_ITEM()
RATIONAL_B_SPLINE_SURFACE(((1.,1.),(1.,1.),(1.,1.),(1.,1.),(1.,1.),(1.,
1.),(1.,1.),(1.,1.),(1.,1.),(1.,1.),(1.,1.),(1.,1.),(1.,1.),(1.,1.),(1.,
1.),(1.,1.),(1.,1.),(1.,1.),(1.,1.),(1.,1.),(1.,1.),(1.,1.),(1.,1.),(1.,
1.),(1.,1.),(1.,1.),(1.,1.),(1.,1.),(1.,1.),(1.,1.),(1.,1.),(1.,1.),(1.,
1.),(1.,1.),(1.,1.),(1.,1.),(1.,1.),(1.,1.),(1.,1.),(1.,1.)))
REPRESENTATION_ITEM('')
SURFACE()
);
#596=(
BOUNDED_SURFACE()
B_SPLINE_SURFACE(5,1,((#60649,#60650),(#60651,#60652),(#60653,#60654),(#60655,
#60656),(#60657,#60658),(#60659,#60660),(#60661,#60662),(#60663,#60664),
(#60665,#60666),(#60667,#60668),(#60669,#60670),(#60671,#60672),(#60673,
#60674),(#60675,#60676),(#60677,#60678),(#60679,#60680),(#60681,#60682),
(#60683,#60684),(#60685,#60686),(#60687,#60688),(#60689,#60690),(#60691,
#60692),(#60693,#60694),(#60695,#60696),(#60697,#60698),(#60699,#60700),
(#60701,#60702),(#60703,#60704),(#60705,#60706),(#60707,#60708),(#60709,
#60710),(#60711,#60712),(#60713,#60714),(#60715,#60716),(#60717,#60718),
(#60719,#60720),(#60721,#60722),(#60723,#60724),(#60725,#60726),(#60727,
#60728)),.UNSPECIFIED.,.F.,.F.,.F.)
B_SPLINE_SURFACE_WITH_KNOTS((6,1,1,1,1,1,1,1,1,1,1,1,1,1,1,1,1,1,1,1,1,
1,1,1,1,1,1,1,1,1,1,1,1,1,1,6),(2,2),(-1.,-0.971428571428572,-0.942857142857143,
-0.914285714285714,-0.885714285714286,-0.857142857142857,-0.828571428571429,
-0.8,-0.771428571428572,-0.742857142857143,-0.714285714285714,-0.685714285714286,
-0.657142857142857,-0.628571428571429,-0.6,-0.571428571428572,-0.542857142857143,
-0.514285714285714,-0.485714285714286,-0.457142857142857,-0.428571428571429,
-0.4,-0.371428571428571,-0.342857142857143,-0.314285714285714,-0.285714285714286,
-0.257142857142857,-0.228571428571429,-0.2,-0.171428571428571,-0.142857142857143,
-0.114285714285714,-0.0857142857142857,-0.0571428571428571,-0.0285714285714286,
0.),(0.,1.6),.UNSPECIFIED.)
GEOMETRIC_REPRESENTATION_ITEM()
RATIONAL_B_SPLINE_SURFACE(((1.,1.),(1.,1.),(1.,1.),(1.,1.),(1.,1.),(1.,
1.),(1.,1.),(1.,1.),(1.,1.),(1.,1.),(1.,1.),(1.,1.),(1.,1.),(1.,1.),(1.,
1.),(1.,1.),(1.,1.),(1.,1.),(1.,1.),(1.,1.),(1.,1.),(1.,1.),(1.,1.),(1.,
1.),(1.,1.),(1.,1.),(1.,1.),(1.,1.),(1.,1.),(1.,1.),(1.,1.),(1.,1.),(1.,
1.),(1.,1.),(1.,1.),(1.,1.),(1.,1.),(1.,1.),(1.,1.),(1.,1.)))
REPRESENTATION_ITEM('')
SURFACE()
);
#597=(
BOUNDED_SURFACE()
B_SPLINE_SURFACE(5,1,((#60748,#60749),(#60750,#60751),(#60752,#60753),(#60754,
#60755),(#60756,#60757),(#60758,#60759),(#60760,#60761),(#60762,#60763),
(#60764,#60765),(#60766,#60767),(#60768,#60769),(#60770,#60771),(#60772,
#60773),(#60774,#60775),(#60776,#60777),(#60778,#60779),(#60780,#60781),
(#60782,#60783),(#60784,#60785),(#60786,#60787),(#60788,#60789),(#60790,
#60791),(#60792,#60793),(#60794,#60795),(#60796,#60797),(#60798,#60799),
(#60800,#60801),(#60802,#60803),(#60804,#60805),(#60806,#60807),(#60808,
#60809),(#60810,#60811),(#60812,#60813),(#60814,#60815),(#60816,#60817),
(#60818,#60819),(#60820,#60821),(#60822,#60823),(#60824,#60825),(#60826,
#60827)),.UNSPECIFIED.,.F.,.F.,.F.)
B_SPLINE_SURFACE_WITH_KNOTS((6,1,1,1,1,1,1,1,1,1,1,1,1,1,1,1,1,1,1,1,1,
1,1,1,1,1,1,1,1,1,1,1,1,1,1,6),(2,2),(-1.,-0.971428571428572,-0.942857142857143,
-0.914285714285714,-0.885714285714286,-0.857142857142857,-0.828571428571429,
-0.8,-0.771428571428572,-0.742857142857143,-0.714285714285714,-0.685714285714286,
-0.657142857142857,-0.628571428571429,-0.6,-0.571428571428572,-0.542857142857143,
-0.514285714285714,-0.485714285714286,-0.457142857142857,-0.428571428571429,
-0.4,-0.371428571428571,-0.342857142857143,-0.314285714285714,-0.285714285714286,
-0.257142857142857,-0.228571428571429,-0.2,-0.171428571428571,-0.142857142857143,
-0.114285714285714,-0.0857142857142857,-0.0571428571428571,-0.0285714285714286,
0.),(0.,1.6),.UNSPECIFIED.)
GEOMETRIC_REPRESENTATION_ITEM()
RATIONAL_B_SPLINE_SURFACE(((1.,1.),(1.,1.),(1.,1.),(1.,1.),(1.,1.),(1.,
1.),(1.,1.),(1.,1.),(1.,1.),(1.,1.),(1.,1.),(1.,1.),(1.,1.),(1.,1.),(1.,
1.),(1.,1.),(1.,1.),(1.,1.),(1.,1.),(1.,1.),(1.,1.),(1.,1.),(1.,1.),(1.,
1.),(1.,1.),(1.,1.),(1.,1.),(1.,1.),(1.,1.),(1.,1.),(1.,1.),(1.,1.),(1.,
1.),(1.,1.),(1.,1.),(1.,1.),(1.,1.),(1.,1.),(1.,1.),(1.,1.)))
REPRESENTATION_ITEM('')
SURFACE()
);
#598=(
BOUNDED_SURFACE()
B_SPLINE_SURFACE(5,1,((#60847,#60848),(#60849,#60850),(#60851,#60852),(#60853,
#60854),(#60855,#60856),(#60857,#60858),(#60859,#60860),(#60861,#60862),
(#60863,#60864),(#60865,#60866),(#60867,#60868),(#60869,#60870),(#60871,
#60872),(#60873,#60874),(#60875,#60876),(#60877,#60878),(#60879,#60880),
(#60881,#60882),(#60883,#60884),(#60885,#60886),(#60887,#60888),(#60889,
#60890),(#60891,#60892),(#60893,#60894),(#60895,#60896),(#60897,#60898),
(#60899,#60900),(#60901,#60902),(#60903,#60904),(#60905,#60906),(#60907,
#60908),(#60909,#60910),(#60911,#60912),(#60913,#60914),(#60915,#60916),
(#60917,#60918),(#60919,#60920),(#60921,#60922),(#60923,#60924),(#60925,
#60926)),.UNSPECIFIED.,.F.,.F.,.F.)
B_SPLINE_SURFACE_WITH_KNOTS((6,1,1,1,1,1,1,1,1,1,1,1,1,1,1,1,1,1,1,1,1,
1,1,1,1,1,1,1,1,1,1,1,1,1,1,6),(2,2),(-1.,-0.971428571428572,-0.942857142857143,
-0.914285714285714,-0.885714285714286,-0.857142857142857,-0.828571428571429,
-0.8,-0.771428571428572,-0.742857142857143,-0.714285714285714,-0.685714285714286,
-0.657142857142857,-0.628571428571429,-0.6,-0.571428571428572,-0.542857142857143,
-0.514285714285714,-0.485714285714286,-0.457142857142857,-0.428571428571429,
-0.4,-0.371428571428571,-0.342857142857143,-0.314285714285714,-0.285714285714286,
-0.257142857142857,-0.228571428571429,-0.2,-0.171428571428571,-0.142857142857143,
-0.114285714285714,-0.0857142857142857,-0.0571428571428571,-0.0285714285714286,
0.),(0.,1.6),.UNSPECIFIED.)
GEOMETRIC_REPRESENTATION_ITEM()
RATIONAL_B_SPLINE_SURFACE(((1.,1.),(1.,1.),(1.,1.),(1.,1.),(1.,1.),(1.,
1.),(1.,1.),(1.,1.),(1.,1.),(1.,1.),(1.,1.),(1.,1.),(1.,1.),(1.,1.),(1.,
1.),(1.,1.),(1.,1.),(1.,1.),(1.,1.),(1.,1.),(1.,1.),(1.,1.),(1.,1.),(1.,
1.),(1.,1.),(1.,1.),(1.,1.),(1.,1.),(1.,1.),(1.,1.),(1.,1.),(1.,1.),(1.,
1.),(1.,1.),(1.,1.),(1.,1.),(1.,1.),(1.,1.),(1.,1.),(1.,1.)))
REPRESENTATION_ITEM('')
SURFACE()
);
#599=(
BOUNDED_SURFACE()
B_SPLINE_SURFACE(5,1,((#60946,#60947),(#60948,#60949),(#60950,#60951),(#60952,
#60953),(#60954,#60955),(#60956,#60957),(#60958,#60959),(#60960,#60961),
(#60962,#60963),(#60964,#60965),(#60966,#60967),(#60968,#60969),(#60970,
#60971),(#60972,#60973),(#60974,#60975),(#60976,#60977),(#60978,#60979),
(#60980,#60981),(#60982,#60983),(#60984,#60985),(#60986,#60987),(#60988,
#60989),(#60990,#60991),(#60992,#60993),(#60994,#60995),(#60996,#60997),
(#60998,#60999),(#61000,#61001),(#61002,#61003),(#61004,#61005),(#61006,
#61007),(#61008,#61009),(#61010,#61011),(#61012,#61013),(#61014,#61015),
(#61016,#61017),(#61018,#61019),(#61020,#61021),(#61022,#61023),(#61024,
#61025)),.UNSPECIFIED.,.F.,.F.,.F.)
B_SPLINE_SURFACE_WITH_KNOTS((6,1,1,1,1,1,1,1,1,1,1,1,1,1,1,1,1,1,1,1,1,
1,1,1,1,1,1,1,1,1,1,1,1,1,1,6),(2,2),(-1.,-0.971428571428572,-0.942857142857143,
-0.914285714285714,-0.885714285714286,-0.857142857142857,-0.828571428571429,
-0.8,-0.771428571428572,-0.742857142857143,-0.714285714285714,-0.685714285714286,
-0.657142857142857,-0.628571428571429,-0.6,-0.571428571428572,-0.542857142857143,
-0.514285714285714,-0.485714285714286,-0.457142857142857,-0.428571428571429,
-0.4,-0.371428571428571,-0.342857142857143,-0.314285714285714,-0.285714285714286,
-0.257142857142857,-0.228571428571429,-0.2,-0.171428571428571,-0.142857142857143,
-0.114285714285714,-0.0857142857142857,-0.0571428571428571,-0.0285714285714286,
0.),(0.,1.6),.UNSPECIFIED.)
GEOMETRIC_REPRESENTATION_ITEM()
RATIONAL_B_SPLINE_SURFACE(((1.,1.),(1.,1.),(1.,1.),(1.,1.),(1.,1.),(1.,
1.),(1.,1.),(1.,1.),(1.,1.),(1.,1.),(1.,1.),(1.,1.),(1.,1.),(1.,1.),(1.,
1.),(1.,1.),(1.,1.),(1.,1.),(1.,1.),(1.,1.),(1.,1.),(1.,1.),(1.,1.),(1.,
1.),(1.,1.),(1.,1.),(1.,1.),(1.,1.),(1.,1.),(1.,1.),(1.,1.),(1.,1.),(1.,
1.),(1.,1.),(1.,1.),(1.,1.),(1.,1.),(1.,1.),(1.,1.),(1.,1.)))
REPRESENTATION_ITEM('')
SURFACE()
);
#600=(
BOUNDED_SURFACE()
B_SPLINE_SURFACE(5,1,((#61045,#61046),(#61047,#61048),(#61049,#61050),(#61051,
#61052),(#61053,#61054),(#61055,#61056),(#61057,#61058),(#61059,#61060),
(#61061,#61062),(#61063,#61064),(#61065,#61066),(#61067,#61068),(#61069,
#61070),(#61071,#61072),(#61073,#61074),(#61075,#61076),(#61077,#61078),
(#61079,#61080),(#61081,#61082),(#61083,#61084),(#61085,#61086),(#61087,
#61088),(#61089,#61090),(#61091,#61092),(#61093,#61094),(#61095,#61096),
(#61097,#61098),(#61099,#61100),(#61101,#61102),(#61103,#61104),(#61105,
#61106),(#61107,#61108),(#61109,#61110),(#61111,#61112),(#61113,#61114),
(#61115,#61116),(#61117,#61118),(#61119,#61120),(#61121,#61122),(#61123,
#61124)),.UNSPECIFIED.,.F.,.F.,.F.)
B_SPLINE_SURFACE_WITH_KNOTS((6,1,1,1,1,1,1,1,1,1,1,1,1,1,1,1,1,1,1,1,1,
1,1,1,1,1,1,1,1,1,1,1,1,1,1,6),(2,2),(-1.,-0.971428571428572,-0.942857142857143,
-0.914285714285714,-0.885714285714286,-0.857142857142857,-0.828571428571429,
-0.8,-0.771428571428572,-0.742857142857143,-0.714285714285714,-0.685714285714286,
-0.657142857142857,-0.628571428571429,-0.6,-0.571428571428572,-0.542857142857143,
-0.514285714285714,-0.485714285714286,-0.457142857142857,-0.428571428571429,
-0.4,-0.371428571428571,-0.342857142857143,-0.314285714285714,-0.285714285714286,
-0.257142857142857,-0.228571428571429,-0.2,-0.171428571428571,-0.142857142857143,
-0.114285714285714,-0.0857142857142857,-0.0571428571428571,-0.0285714285714286,
0.),(0.,1.6),.UNSPECIFIED.)
GEOMETRIC_REPRESENTATION_ITEM()
RATIONAL_B_SPLINE_SURFACE(((1.,1.),(1.,1.),(1.,1.),(1.,1.),(1.,1.),(1.,
1.),(1.,1.),(1.,1.),(1.,1.),(1.,1.),(1.,1.),(1.,1.),(1.,1.),(1.,1.),(1.,
1.),(1.,1.),(1.,1.),(1.,1.),(1.,1.),(1.,1.),(1.,1.),(1.,1.),(1.,1.),(1.,
1.),(1.,1.),(1.,1.),(1.,1.),(1.,1.),(1.,1.),(1.,1.),(1.,1.),(1.,1.),(1.,
1.),(1.,1.),(1.,1.),(1.,1.),(1.,1.),(1.,1.),(1.,1.),(1.,1.)))
REPRESENTATION_ITEM('')
SURFACE()
);
#601=(
BOUNDED_SURFACE()
B_SPLINE_SURFACE(5,1,((#61144,#61145),(#61146,#61147),(#61148,#61149),(#61150,
#61151),(#61152,#61153),(#61154,#61155),(#61156,#61157),(#61158,#61159),
(#61160,#61161),(#61162,#61163),(#61164,#61165),(#61166,#61167),(#61168,
#61169),(#61170,#61171),(#61172,#61173),(#61174,#61175),(#61176,#61177),
(#61178,#61179),(#61180,#61181),(#61182,#61183),(#61184,#61185),(#61186,
#61187),(#61188,#61189),(#61190,#61191),(#61192,#61193),(#61194,#61195),
(#61196,#61197),(#61198,#61199),(#61200,#61201),(#61202,#61203),(#61204,
#61205),(#61206,#61207),(#61208,#61209),(#61210,#61211),(#61212,#61213),
(#61214,#61215),(#61216,#61217),(#61218,#61219),(#61220,#61221),(#61222,
#61223)),.UNSPECIFIED.,.F.,.F.,.F.)
B_SPLINE_SURFACE_WITH_KNOTS((6,1,1,1,1,1,1,1,1,1,1,1,1,1,1,1,1,1,1,1,1,
1,1,1,1,1,1,1,1,1,1,1,1,1,1,6),(2,2),(-1.,-0.971428571428572,-0.942857142857143,
-0.914285714285714,-0.885714285714286,-0.857142857142857,-0.828571428571429,
-0.8,-0.771428571428572,-0.742857142857143,-0.714285714285714,-0.685714285714286,
-0.657142857142857,-0.628571428571429,-0.6,-0.571428571428572,-0.542857142857143,
-0.514285714285714,-0.485714285714286,-0.457142857142857,-0.428571428571429,
-0.4,-0.371428571428571,-0.342857142857143,-0.314285714285714,-0.285714285714286,
-0.257142857142857,-0.228571428571429,-0.2,-0.171428571428571,-0.142857142857143,
-0.114285714285714,-0.0857142857142857,-0.0571428571428571,-0.0285714285714286,
0.),(0.,1.6),.UNSPECIFIED.)
GEOMETRIC_REPRESENTATION_ITEM()
RATIONAL_B_SPLINE_SURFACE(((1.,1.),(1.,1.),(1.,1.),(1.,1.),(1.,1.),(1.,
1.),(1.,1.),(1.,1.),(1.,1.),(1.,1.),(1.,1.),(1.,1.),(1.,1.),(1.,1.),(1.,
1.),(1.,1.),(1.,1.),(1.,1.),(1.,1.),(1.,1.),(1.,1.),(1.,1.),(1.,1.),(1.,
1.),(1.,1.),(1.,1.),(1.,1.),(1.,1.),(1.,1.),(1.,1.),(1.,1.),(1.,1.),(1.,
1.),(1.,1.),(1.,1.),(1.,1.),(1.,1.),(1.,1.),(1.,1.),(1.,1.)))
REPRESENTATION_ITEM('')
SURFACE()
);
#602=(
BOUNDED_SURFACE()
B_SPLINE_SURFACE(5,1,((#61243,#61244),(#61245,#61246),(#61247,#61248),(#61249,
#61250),(#61251,#61252),(#61253,#61254),(#61255,#61256),(#61257,#61258),
(#61259,#61260),(#61261,#61262),(#61263,#61264),(#61265,#61266),(#61267,
#61268),(#61269,#61270),(#61271,#61272),(#61273,#61274),(#61275,#61276),
(#61277,#61278),(#61279,#61280),(#61281,#61282),(#61283,#61284),(#61285,
#61286),(#61287,#61288),(#61289,#61290),(#61291,#61292),(#61293,#61294),
(#61295,#61296),(#61297,#61298),(#61299,#61300),(#61301,#61302),(#61303,
#61304),(#61305,#61306),(#61307,#61308),(#61309,#61310),(#61311,#61312),
(#61313,#61314),(#61315,#61316),(#61317,#61318),(#61319,#61320),(#61321,
#61322)),.UNSPECIFIED.,.F.,.F.,.F.)
B_SPLINE_SURFACE_WITH_KNOTS((6,1,1,1,1,1,1,1,1,1,1,1,1,1,1,1,1,1,1,1,1,
1,1,1,1,1,1,1,1,1,1,1,1,1,1,6),(2,2),(-1.,-0.971428571428572,-0.942857142857143,
-0.914285714285714,-0.885714285714286,-0.857142857142857,-0.828571428571429,
-0.8,-0.771428571428572,-0.742857142857143,-0.714285714285714,-0.685714285714286,
-0.657142857142857,-0.628571428571429,-0.6,-0.571428571428572,-0.542857142857143,
-0.514285714285714,-0.485714285714286,-0.457142857142857,-0.428571428571429,
-0.4,-0.371428571428571,-0.342857142857143,-0.314285714285714,-0.285714285714286,
-0.257142857142857,-0.228571428571429,-0.2,-0.171428571428571,-0.142857142857143,
-0.114285714285714,-0.0857142857142857,-0.0571428571428571,-0.0285714285714286,
0.),(0.,1.6),.UNSPECIFIED.)
GEOMETRIC_REPRESENTATION_ITEM()
RATIONAL_B_SPLINE_SURFACE(((1.,1.),(1.,1.),(1.,1.),(1.,1.),(1.,1.),(1.,
1.),(1.,1.),(1.,1.),(1.,1.),(1.,1.),(1.,1.),(1.,1.),(1.,1.),(1.,1.),(1.,
1.),(1.,1.),(1.,1.),(1.,1.),(1.,1.),(1.,1.),(1.,1.),(1.,1.),(1.,1.),(1.,
1.),(1.,1.),(1.,1.),(1.,1.),(1.,1.),(1.,1.),(1.,1.),(1.,1.),(1.,1.),(1.,
1.),(1.,1.),(1.,1.),(1.,1.),(1.,1.),(1.,1.),(1.,1.),(1.,1.)))
REPRESENTATION_ITEM('')
SURFACE()
);
#603=(
BOUNDED_SURFACE()
B_SPLINE_SURFACE(5,1,((#61342,#61343),(#61344,#61345),(#61346,#61347),(#61348,
#61349),(#61350,#61351),(#61352,#61353),(#61354,#61355),(#61356,#61357),
(#61358,#61359),(#61360,#61361),(#61362,#61363),(#61364,#61365),(#61366,
#61367),(#61368,#61369),(#61370,#61371),(#61372,#61373),(#61374,#61375),
(#61376,#61377),(#61378,#61379),(#61380,#61381),(#61382,#61383),(#61384,
#61385),(#61386,#61387),(#61388,#61389),(#61390,#61391),(#61392,#61393),
(#61394,#61395),(#61396,#61397),(#61398,#61399),(#61400,#61401),(#61402,
#61403),(#61404,#61405),(#61406,#61407),(#61408,#61409),(#61410,#61411),
(#61412,#61413),(#61414,#61415),(#61416,#61417),(#61418,#61419),(#61420,
#61421)),.UNSPECIFIED.,.F.,.F.,.F.)
B_SPLINE_SURFACE_WITH_KNOTS((6,1,1,1,1,1,1,1,1,1,1,1,1,1,1,1,1,1,1,1,1,
1,1,1,1,1,1,1,1,1,1,1,1,1,1,6),(2,2),(-1.,-0.971428571428572,-0.942857142857143,
-0.914285714285714,-0.885714285714286,-0.857142857142857,-0.828571428571429,
-0.8,-0.771428571428572,-0.742857142857143,-0.714285714285714,-0.685714285714286,
-0.657142857142857,-0.628571428571429,-0.6,-0.571428571428572,-0.542857142857143,
-0.514285714285714,-0.485714285714286,-0.457142857142857,-0.428571428571429,
-0.4,-0.371428571428571,-0.342857142857143,-0.314285714285714,-0.285714285714286,
-0.257142857142857,-0.228571428571429,-0.2,-0.171428571428571,-0.142857142857143,
-0.114285714285714,-0.0857142857142857,-0.0571428571428571,-0.0285714285714286,
0.),(0.,1.6),.UNSPECIFIED.)
GEOMETRIC_REPRESENTATION_ITEM()
RATIONAL_B_SPLINE_SURFACE(((1.,1.),(1.,1.),(1.,1.),(1.,1.),(1.,1.),(1.,
1.),(1.,1.),(1.,1.),(1.,1.),(1.,1.),(1.,1.),(1.,1.),(1.,1.),(1.,1.),(1.,
1.),(1.,1.),(1.,1.),(1.,1.),(1.,1.),(1.,1.),(1.,1.),(1.,1.),(1.,1.),(1.,
1.),(1.,1.),(1.,1.),(1.,1.),(1.,1.),(1.,1.),(1.,1.),(1.,1.),(1.,1.),(1.,
1.),(1.,1.),(1.,1.),(1.,1.),(1.,1.),(1.,1.),(1.,1.),(1.,1.)))
REPRESENTATION_ITEM('')
SURFACE()
);
#604=(
BOUNDED_SURFACE()
B_SPLINE_SURFACE(5,1,((#61441,#61442),(#61443,#61444),(#61445,#61446),(#61447,
#61448),(#61449,#61450),(#61451,#61452),(#61453,#61454),(#61455,#61456),
(#61457,#61458),(#61459,#61460),(#61461,#61462),(#61463,#61464),(#61465,
#61466),(#61467,#61468),(#61469,#61470),(#61471,#61472),(#61473,#61474),
(#61475,#61476),(#61477,#61478),(#61479,#61480),(#61481,#61482),(#61483,
#61484),(#61485,#61486),(#61487,#61488),(#61489,#61490),(#61491,#61492),
(#61493,#61494),(#61495,#61496),(#61497,#61498),(#61499,#61500),(#61501,
#61502),(#61503,#61504),(#61505,#61506),(#61507,#61508),(#61509,#61510),
(#61511,#61512),(#61513,#61514),(#61515,#61516),(#61517,#61518),(#61519,
#61520)),.UNSPECIFIED.,.F.,.F.,.F.)
B_SPLINE_SURFACE_WITH_KNOTS((6,1,1,1,1,1,1,1,1,1,1,1,1,1,1,1,1,1,1,1,1,
1,1,1,1,1,1,1,1,1,1,1,1,1,1,6),(2,2),(-1.,-0.971428571428572,-0.942857142857143,
-0.914285714285714,-0.885714285714286,-0.857142857142857,-0.828571428571429,
-0.8,-0.771428571428572,-0.742857142857143,-0.714285714285714,-0.685714285714286,
-0.657142857142857,-0.628571428571429,-0.6,-0.571428571428572,-0.542857142857143,
-0.514285714285714,-0.485714285714286,-0.457142857142857,-0.428571428571429,
-0.4,-0.371428571428571,-0.342857142857143,-0.314285714285714,-0.285714285714286,
-0.257142857142857,-0.228571428571429,-0.2,-0.171428571428571,-0.142857142857143,
-0.114285714285714,-0.0857142857142857,-0.0571428571428571,-0.0285714285714286,
0.),(0.,1.6),.UNSPECIFIED.)
GEOMETRIC_REPRESENTATION_ITEM()
RATIONAL_B_SPLINE_SURFACE(((1.,1.),(1.,1.),(1.,1.),(1.,1.),(1.,1.),(1.,
1.),(1.,1.),(1.,1.),(1.,1.),(1.,1.),(1.,1.),(1.,1.),(1.,1.),(1.,1.),(1.,
1.),(1.,1.),(1.,1.),(1.,1.),(1.,1.),(1.,1.),(1.,1.),(1.,1.),(1.,1.),(1.,
1.),(1.,1.),(1.,1.),(1.,1.),(1.,1.),(1.,1.),(1.,1.),(1.,1.),(1.,1.),(1.,
1.),(1.,1.),(1.,1.),(1.,1.),(1.,1.),(1.,1.),(1.,1.),(1.,1.)))
REPRESENTATION_ITEM('')
SURFACE()
);
#605=(
BOUNDED_SURFACE()
B_SPLINE_SURFACE(5,1,((#61540,#61541),(#61542,#61543),(#61544,#61545),(#61546,
#61547),(#61548,#61549),(#61550,#61551),(#61552,#61553),(#61554,#61555),
(#61556,#61557),(#61558,#61559),(#61560,#61561),(#61562,#61563),(#61564,
#61565),(#61566,#61567),(#61568,#61569),(#61570,#61571),(#61572,#61573),
(#61574,#61575),(#61576,#61577),(#61578,#61579),(#61580,#61581),(#61582,
#61583),(#61584,#61585),(#61586,#61587),(#61588,#61589),(#61590,#61591),
(#61592,#61593),(#61594,#61595),(#61596,#61597),(#61598,#61599),(#61600,
#61601),(#61602,#61603),(#61604,#61605),(#61606,#61607),(#61608,#61609),
(#61610,#61611),(#61612,#61613),(#61614,#61615),(#61616,#61617),(#61618,
#61619)),.UNSPECIFIED.,.F.,.F.,.F.)
B_SPLINE_SURFACE_WITH_KNOTS((6,1,1,1,1,1,1,1,1,1,1,1,1,1,1,1,1,1,1,1,1,
1,1,1,1,1,1,1,1,1,1,1,1,1,1,6),(2,2),(-1.,-0.971428571428572,-0.942857142857143,
-0.914285714285714,-0.885714285714286,-0.857142857142857,-0.828571428571429,
-0.8,-0.771428571428572,-0.742857142857143,-0.714285714285714,-0.685714285714286,
-0.657142857142857,-0.628571428571429,-0.6,-0.571428571428572,-0.542857142857143,
-0.514285714285714,-0.485714285714286,-0.457142857142857,-0.428571428571429,
-0.4,-0.371428571428571,-0.342857142857143,-0.314285714285714,-0.285714285714286,
-0.257142857142857,-0.228571428571429,-0.2,-0.171428571428571,-0.142857142857143,
-0.114285714285714,-0.0857142857142857,-0.0571428571428571,-0.0285714285714286,
0.),(0.,1.6),.UNSPECIFIED.)
GEOMETRIC_REPRESENTATION_ITEM()
RATIONAL_B_SPLINE_SURFACE(((1.,1.),(1.,1.),(1.,1.),(1.,1.),(1.,1.),(1.,
1.),(1.,1.),(1.,1.),(1.,1.),(1.,1.),(1.,1.),(1.,1.),(1.,1.),(1.,1.),(1.,
1.),(1.,1.),(1.,1.),(1.,1.),(1.,1.),(1.,1.),(1.,1.),(1.,1.),(1.,1.),(1.,
1.),(1.,1.),(1.,1.),(1.,1.),(1.,1.),(1.,1.),(1.,1.),(1.,1.),(1.,1.),(1.,
1.),(1.,1.),(1.,1.),(1.,1.),(1.,1.),(1.,1.),(1.,1.),(1.,1.)))
REPRESENTATION_ITEM('')
SURFACE()
);
#606=(
BOUNDED_SURFACE()
B_SPLINE_SURFACE(5,1,((#61639,#61640),(#61641,#61642),(#61643,#61644),(#61645,
#61646),(#61647,#61648),(#61649,#61650),(#61651,#61652),(#61653,#61654),
(#61655,#61656),(#61657,#61658),(#61659,#61660),(#61661,#61662),(#61663,
#61664),(#61665,#61666),(#61667,#61668),(#61669,#61670),(#61671,#61672),
(#61673,#61674),(#61675,#61676),(#61677,#61678),(#61679,#61680),(#61681,
#61682),(#61683,#61684),(#61685,#61686),(#61687,#61688),(#61689,#61690),
(#61691,#61692),(#61693,#61694),(#61695,#61696),(#61697,#61698),(#61699,
#61700),(#61701,#61702),(#61703,#61704),(#61705,#61706),(#61707,#61708),
(#61709,#61710),(#61711,#61712),(#61713,#61714),(#61715,#61716),(#61717,
#61718)),.UNSPECIFIED.,.F.,.F.,.F.)
B_SPLINE_SURFACE_WITH_KNOTS((6,1,1,1,1,1,1,1,1,1,1,1,1,1,1,1,1,1,1,1,1,
1,1,1,1,1,1,1,1,1,1,1,1,1,1,6),(2,2),(-1.,-0.971428571428572,-0.942857142857143,
-0.914285714285714,-0.885714285714286,-0.857142857142857,-0.828571428571429,
-0.8,-0.771428571428572,-0.742857142857143,-0.714285714285714,-0.685714285714286,
-0.657142857142857,-0.628571428571429,-0.6,-0.571428571428572,-0.542857142857143,
-0.514285714285714,-0.485714285714286,-0.457142857142857,-0.428571428571429,
-0.4,-0.371428571428571,-0.342857142857143,-0.314285714285714,-0.285714285714286,
-0.257142857142857,-0.228571428571429,-0.2,-0.171428571428571,-0.142857142857143,
-0.114285714285714,-0.0857142857142857,-0.0571428571428571,-0.0285714285714286,
0.),(0.,1.6),.UNSPECIFIED.)
GEOMETRIC_REPRESENTATION_ITEM()
RATIONAL_B_SPLINE_SURFACE(((1.,1.),(1.,1.),(1.,1.),(1.,1.),(1.,1.),(1.,
1.),(1.,1.),(1.,1.),(1.,1.),(1.,1.),(1.,1.),(1.,1.),(1.,1.),(1.,1.),(1.,
1.),(1.,1.),(1.,1.),(1.,1.),(1.,1.),(1.,1.),(1.,1.),(1.,1.),(1.,1.),(1.,
1.),(1.,1.),(1.,1.),(1.,1.),(1.,1.),(1.,1.),(1.,1.),(1.,1.),(1.,1.),(1.,
1.),(1.,1.),(1.,1.),(1.,1.),(1.,1.),(1.,1.),(1.,1.),(1.,1.)))
REPRESENTATION_ITEM('')
SURFACE()
);
#607=(
BOUNDED_SURFACE()
B_SPLINE_SURFACE(5,1,((#61738,#61739),(#61740,#61741),(#61742,#61743),(#61744,
#61745),(#61746,#61747),(#61748,#61749),(#61750,#61751),(#61752,#61753),
(#61754,#61755),(#61756,#61757),(#61758,#61759),(#61760,#61761),(#61762,
#61763),(#61764,#61765),(#61766,#61767),(#61768,#61769),(#61770,#61771),
(#61772,#61773),(#61774,#61775),(#61776,#61777),(#61778,#61779),(#61780,
#61781),(#61782,#61783),(#61784,#61785),(#61786,#61787),(#61788,#61789),
(#61790,#61791),(#61792,#61793),(#61794,#61795),(#61796,#61797),(#61798,
#61799),(#61800,#61801),(#61802,#61803),(#61804,#61805),(#61806,#61807),
(#61808,#61809),(#61810,#61811),(#61812,#61813),(#61814,#61815),(#61816,
#61817)),.UNSPECIFIED.,.F.,.F.,.F.)
B_SPLINE_SURFACE_WITH_KNOTS((6,1,1,1,1,1,1,1,1,1,1,1,1,1,1,1,1,1,1,1,1,
1,1,1,1,1,1,1,1,1,1,1,1,1,1,6),(2,2),(-1.,-0.971428571428572,-0.942857142857143,
-0.914285714285714,-0.885714285714286,-0.857142857142857,-0.828571428571429,
-0.8,-0.771428571428572,-0.742857142857143,-0.714285714285714,-0.685714285714286,
-0.657142857142857,-0.628571428571429,-0.6,-0.571428571428572,-0.542857142857143,
-0.514285714285714,-0.485714285714286,-0.457142857142857,-0.428571428571429,
-0.4,-0.371428571428571,-0.342857142857143,-0.314285714285714,-0.285714285714286,
-0.257142857142857,-0.228571428571429,-0.2,-0.171428571428571,-0.142857142857143,
-0.114285714285714,-0.0857142857142857,-0.0571428571428571,-0.0285714285714286,
0.),(0.,1.6),.UNSPECIFIED.)
GEOMETRIC_REPRESENTATION_ITEM()
RATIONAL_B_SPLINE_SURFACE(((1.,1.),(1.,1.),(1.,1.),(1.,1.),(1.,1.),(1.,
1.),(1.,1.),(1.,1.),(1.,1.),(1.,1.),(1.,1.),(1.,1.),(1.,1.),(1.,1.),(1.,
1.),(1.,1.),(1.,1.),(1.,1.),(1.,1.),(1.,1.),(1.,1.),(1.,1.),(1.,1.),(1.,
1.),(1.,1.),(1.,1.),(1.,1.),(1.,1.),(1.,1.),(1.,1.),(1.,1.),(1.,1.),(1.,
1.),(1.,1.),(1.,1.),(1.,1.),(1.,1.),(1.,1.),(1.,1.),(1.,1.)))
REPRESENTATION_ITEM('')
SURFACE()
);
#608=(
BOUNDED_CURVE()
B_SPLINE_CURVE(5,(#42367,#42368,#42369,#42370,#42371,#42372,#42373,#42374,
#42375,#42376,#42377,#42378,#42379,#42380,#42381,#42382,#42383,#42384,#42385,
#42386,#42387,#42388,#42389,#42390,#42391,#42392,#42393,#42394,#42395),
 .UNSPECIFIED.,.F.,.F.)
B_SPLINE_CURVE_WITH_KNOTS((6,1,1,1,1,1,1,1,1,1,1,1,1,1,1,1,1,1,1,1,1,1,
1,1,6),(0.,0.0285714285714286,0.0571428571428571,0.0857142857142857,0.114285714285714,
0.142857142857143,0.171428571428571,0.2,0.228571428571429,0.257142857142857,
0.285714285714286,0.314285714285714,0.342857142857143,0.371428571428571,
0.4,0.428571428571429,0.457142857142857,0.485714285714286,0.514285714285714,
0.542857142857143,0.571428571428572,0.6,0.628571428571429,0.657142857142857,
0.667078900656917),.UNSPECIFIED.)
CURVE()
GEOMETRIC_REPRESENTATION_ITEM()
RATIONAL_B_SPLINE_CURVE((1.,1.,1.,1.,1.,1.,1.,1.,1.,1.,1.,1.,1.,1.,1.,1.,
1.,1.,1.,1.,1.,1.,1.,1.,1.,1.,1.,1.,1.))
REPRESENTATION_ITEM('')
);
#609=(
BOUNDED_CURVE()
B_SPLINE_CURVE(5,(#42398,#42399,#42400,#42401,#42402,#42403,#42404,#42405,
#42406,#42407,#42408,#42409,#42410,#42411,#42412,#42413,#42414,#42415,#42416,
#42417,#42418,#42419,#42420,#42421,#42422),.UNSPECIFIED.,.F.,.F.)
B_SPLINE_CURVE_WITH_KNOTS((6,1,1,1,1,1,1,1,1,1,1,1,1,1,1,1,1,1,1,1,6),(0.436331539942223,
0.457142857142857,0.485714285714286,0.514285714285714,0.542857142857143,
0.571428571428572,0.6,0.628571428571429,0.657142857142857,0.685714285714286,
0.714285714285714,0.742857142857143,0.771428571428572,0.8,0.828571428571429,
0.857142857142857,0.885714285714286,0.914285714285714,0.942857142857143,
0.971428571428572,1.),.UNSPECIFIED.)
CURVE()
GEOMETRIC_REPRESENTATION_ITEM()
RATIONAL_B_SPLINE_CURVE((1.,1.,1.,1.,1.,1.,1.,1.,1.,1.,1.,1.,1.,1.,1.,1.,
1.,1.,1.,1.,1.,1.,1.,1.,1.))
REPRESENTATION_ITEM('')
);
#610=(
BOUNDED_CURVE()
B_SPLINE_CURVE(5,(#42511,#42512,#42513,#42514,#42515,#42516,#42517,#42518,
#42519,#42520,#42521,#42522,#42523,#42524,#42525,#42526,#42527,#42528,#42529,
#42530,#42531,#42532,#42533,#42534,#42535),.UNSPECIFIED.,.F.,.F.)
B_SPLINE_CURVE_WITH_KNOTS((6,1,1,1,1,1,1,1,1,1,1,1,1,1,1,1,1,1,1,1,6),(-1.,
-0.971428571428572,-0.942857142857143,-0.914285714285714,-0.885714285714286,
-0.857142857142857,-0.828571428571429,-0.8,-0.771428571428572,-0.742857142857143,
-0.714285714285714,-0.685714285714286,-0.657142857142857,-0.628571428571429,
-0.6,-0.571428571428572,-0.542857142857143,-0.514285714285714,-0.485714285714286,
-0.457142857142857,-0.436331539942219),.UNSPECIFIED.)
CURVE()
GEOMETRIC_REPRESENTATION_ITEM()
RATIONAL_B_SPLINE_CURVE((1.,1.,1.,1.,1.,1.,1.,1.,1.,1.,1.,1.,1.,1.,1.,1.,
1.,1.,1.,1.,1.,1.,1.,1.,1.))
REPRESENTATION_ITEM('')
);
#611=(
BOUNDED_CURVE()
B_SPLINE_CURVE(5,(#42652,#42653,#42654,#42655,#42656,#42657,#42658,#42659,
#42660,#42661,#42662,#42663,#42664,#42665,#42666,#42667,#42668,#42669,#42670,
#42671,#42672,#42673,#42674,#42675,#42676,#42677,#42678,#42679,#42680),
 .UNSPECIFIED.,.F.,.F.)
B_SPLINE_CURVE_WITH_KNOTS((6,1,1,1,1,1,1,1,1,1,1,1,1,1,1,1,1,1,1,1,1,1,
1,1,6),(-0.667078900656922,-0.657142857142857,-0.628571428571429,-0.6,-0.571428571428572,
-0.542857142857143,-0.514285714285714,-0.485714285714286,-0.457142857142857,
-0.428571428571429,-0.4,-0.371428571428571,-0.342857142857143,-0.314285714285714,
-0.285714285714286,-0.257142857142857,-0.228571428571429,-0.2,-0.171428571428571,
-0.142857142857143,-0.114285714285714,-0.0857142857142857,-0.0571428571428571,
-0.0285714285714286,0.),.UNSPECIFIED.)
CURVE()
GEOMETRIC_REPRESENTATION_ITEM()
RATIONAL_B_SPLINE_CURVE((1.,1.,1.,1.,1.,1.,1.,1.,1.,1.,1.,1.,1.,1.,1.,1.,
1.,1.,1.,1.,1.,1.,1.,1.,1.,1.,1.,1.,1.))
REPRESENTATION_ITEM('')
);
#612=(
BOUNDED_CURVE()
B_SPLINE_CURVE(5,(#42719,#42720,#42721,#42722,#42723,#42724,#42725,#42726,
#42727,#42728,#42729,#42730,#42731,#42732,#42733,#42734,#42735,#42736,#42737,
#42738,#42739,#42740,#42741,#42742,#42743,#42744,#42745,#42746,#42747),
 .UNSPECIFIED.,.F.,.F.)
B_SPLINE_CURVE_WITH_KNOTS((6,1,1,1,1,1,1,1,1,1,1,1,1,1,1,1,1,1,1,1,1,1,
1,1,6),(0.,0.0285714285714286,0.0571428571428571,0.0857142857142857,0.114285714285714,
0.142857142857143,0.171428571428571,0.2,0.228571428571429,0.257142857142857,
0.285714285714286,0.314285714285714,0.342857142857143,0.371428571428571,
0.4,0.428571428571429,0.457142857142857,0.485714285714286,0.514285714285714,
0.542857142857143,0.571428571428572,0.6,0.628571428571429,0.657142857142857,
0.667078900656917),.UNSPECIFIED.)
CURVE()
GEOMETRIC_REPRESENTATION_ITEM()
RATIONAL_B_SPLINE_CURVE((1.,1.,1.,1.,1.,1.,1.,1.,1.,1.,1.,1.,1.,1.,1.,1.,
1.,1.,1.,1.,1.,1.,1.,1.,1.,1.,1.,1.,1.))
REPRESENTATION_ITEM('')
);
#613=(
BOUNDED_CURVE()
B_SPLINE_CURVE(5,(#42750,#42751,#42752,#42753,#42754,#42755,#42756,#42757,
#42758,#42759,#42760,#42761,#42762,#42763,#42764,#42765,#42766,#42767,#42768,
#42769,#42770,#42771,#42772,#42773,#42774),.UNSPECIFIED.,.F.,.F.)
B_SPLINE_CURVE_WITH_KNOTS((6,1,1,1,1,1,1,1,1,1,1,1,1,1,1,1,1,1,1,1,6),(0.436331539942223,
0.457142857142857,0.485714285714286,0.514285714285714,0.542857142857143,
0.571428571428572,0.6,0.628571428571429,0.657142857142857,0.685714285714286,
0.714285714285714,0.742857142857143,0.771428571428572,0.8,0.828571428571429,
0.857142857142857,0.885714285714286,0.914285714285714,0.942857142857143,
0.971428571428572,1.),.UNSPECIFIED.)
CURVE()
GEOMETRIC_REPRESENTATION_ITEM()
RATIONAL_B_SPLINE_CURVE((1.,1.,1.,1.,1.,1.,1.,1.,1.,1.,1.,1.,1.,1.,1.,1.,
1.,1.,1.,1.,1.,1.,1.,1.,1.))
REPRESENTATION_ITEM('')
);
#614=(
BOUNDED_CURVE()
B_SPLINE_CURVE(5,(#42863,#42864,#42865,#42866,#42867,#42868,#42869,#42870,
#42871,#42872,#42873,#42874,#42875,#42876,#42877,#42878,#42879,#42880,#42881,
#42882,#42883,#42884,#42885,#42886,#42887),.UNSPECIFIED.,.F.,.F.)
B_SPLINE_CURVE_WITH_KNOTS((6,1,1,1,1,1,1,1,1,1,1,1,1,1,1,1,1,1,1,1,6),(-1.,
-0.971428571428572,-0.942857142857143,-0.914285714285714,-0.885714285714286,
-0.857142857142857,-0.828571428571429,-0.8,-0.771428571428572,-0.742857142857143,
-0.714285714285714,-0.685714285714286,-0.657142857142857,-0.628571428571429,
-0.6,-0.571428571428572,-0.542857142857143,-0.514285714285714,-0.485714285714286,
-0.457142857142857,-0.436331539942219),.UNSPECIFIED.)
CURVE()
GEOMETRIC_REPRESENTATION_ITEM()
RATIONAL_B_SPLINE_CURVE((1.,1.,1.,1.,1.,1.,1.,1.,1.,1.,1.,1.,1.,1.,1.,1.,
1.,1.,1.,1.,1.,1.,1.,1.,1.))
REPRESENTATION_ITEM('')
);
#615=(
BOUNDED_CURVE()
B_SPLINE_CURVE(5,(#42983,#42984,#42985,#42986,#42987,#42988,#42989,#42990,
#42991,#42992,#42993,#42994,#42995,#42996,#42997,#42998,#42999,#43000,#43001,
#43002,#43003,#43004,#43005,#43006,#43007,#43008,#43009,#43010,#43011),
 .UNSPECIFIED.,.F.,.F.)
B_SPLINE_CURVE_WITH_KNOTS((6,1,1,1,1,1,1,1,1,1,1,1,1,1,1,1,1,1,1,1,1,1,
1,1,6),(-0.667078900656922,-0.657142857142857,-0.628571428571429,-0.6,-0.571428571428572,
-0.542857142857143,-0.514285714285714,-0.485714285714286,-0.457142857142857,
-0.428571428571429,-0.4,-0.371428571428571,-0.342857142857143,-0.314285714285714,
-0.285714285714286,-0.257142857142857,-0.228571428571429,-0.2,-0.171428571428571,
-0.142857142857143,-0.114285714285714,-0.0857142857142857,-0.0571428571428571,
-0.0285714285714286,0.),.UNSPECIFIED.)
CURVE()
GEOMETRIC_REPRESENTATION_ITEM()
RATIONAL_B_SPLINE_CURVE((1.,1.,1.,1.,1.,1.,1.,1.,1.,1.,1.,1.,1.,1.,1.,1.,
1.,1.,1.,1.,1.,1.,1.,1.,1.,1.,1.,1.,1.))
REPRESENTATION_ITEM('')
);
#616=(
BOUNDED_CURVE()
B_SPLINE_CURVE(5,(#43041,#43042,#43043,#43044,#43045,#43046,#43047,#43048,
#43049,#43050,#43051,#43052,#43053,#43054,#43055,#43056,#43057,#43058,#43059,
#43060,#43061,#43062,#43063,#43064,#43065,#43066,#43067,#43068,#43069),
 .UNSPECIFIED.,.F.,.F.)
B_SPLINE_CURVE_WITH_KNOTS((6,1,1,1,1,1,1,1,1,1,1,1,1,1,1,1,1,1,1,1,1,1,
1,1,6),(0.,0.0285714285714286,0.0571428571428571,0.0857142857142857,0.114285714285714,
0.142857142857143,0.171428571428571,0.2,0.228571428571429,0.257142857142857,
0.285714285714286,0.314285714285714,0.342857142857143,0.371428571428571,
0.4,0.428571428571429,0.457142857142857,0.485714285714286,0.514285714285714,
0.542857142857143,0.571428571428572,0.6,0.628571428571429,0.657142857142857,
0.667078900656917),.UNSPECIFIED.)
CURVE()
GEOMETRIC_REPRESENTATION_ITEM()
RATIONAL_B_SPLINE_CURVE((1.,1.,1.,1.,1.,1.,1.,1.,1.,1.,1.,1.,1.,1.,1.,1.,
1.,1.,1.,1.,1.,1.,1.,1.,1.,1.,1.,1.,1.))
REPRESENTATION_ITEM('')
);
#617=(
BOUNDED_CURVE()
B_SPLINE_CURVE(5,(#43072,#43073,#43074,#43075,#43076,#43077,#43078,#43079,
#43080,#43081,#43082,#43083,#43084,#43085,#43086,#43087,#43088,#43089,#43090,
#43091,#43092,#43093,#43094,#43095,#43096),.UNSPECIFIED.,.F.,.F.)
B_SPLINE_CURVE_WITH_KNOTS((6,1,1,1,1,1,1,1,1,1,1,1,1,1,1,1,1,1,1,1,6),(0.436331539942223,
0.457142857142857,0.485714285714286,0.514285714285714,0.542857142857143,
0.571428571428572,0.6,0.628571428571429,0.657142857142857,0.685714285714286,
0.714285714285714,0.742857142857143,0.771428571428572,0.8,0.828571428571429,
0.857142857142857,0.885714285714286,0.914285714285714,0.942857142857143,
0.971428571428572,1.),.UNSPECIFIED.)
CURVE()
GEOMETRIC_REPRESENTATION_ITEM()
RATIONAL_B_SPLINE_CURVE((1.,1.,1.,1.,1.,1.,1.,1.,1.,1.,1.,1.,1.,1.,1.,1.,
1.,1.,1.,1.,1.,1.,1.,1.,1.))
REPRESENTATION_ITEM('')
);
#618=(
BOUNDED_CURVE()
B_SPLINE_CURVE(5,(#43185,#43186,#43187,#43188,#43189,#43190,#43191,#43192,
#43193,#43194,#43195,#43196,#43197,#43198,#43199,#43200,#43201,#43202,#43203,
#43204,#43205,#43206,#43207,#43208,#43209),.UNSPECIFIED.,.F.,.F.)
B_SPLINE_CURVE_WITH_KNOTS((6,1,1,1,1,1,1,1,1,1,1,1,1,1,1,1,1,1,1,1,6),(-1.,
-0.971428571428572,-0.942857142857143,-0.914285714285714,-0.885714285714286,
-0.857142857142857,-0.828571428571429,-0.8,-0.771428571428572,-0.742857142857143,
-0.714285714285714,-0.685714285714286,-0.657142857142857,-0.628571428571429,
-0.6,-0.571428571428572,-0.542857142857143,-0.514285714285714,-0.485714285714286,
-0.457142857142857,-0.436331539942219),.UNSPECIFIED.)
CURVE()
GEOMETRIC_REPRESENTATION_ITEM()
RATIONAL_B_SPLINE_CURVE((1.,1.,1.,1.,1.,1.,1.,1.,1.,1.,1.,1.,1.,1.,1.,1.,
1.,1.,1.,1.,1.,1.,1.,1.,1.))
REPRESENTATION_ITEM('')
);
#619=(
BOUNDED_CURVE()
B_SPLINE_CURVE(5,(#43305,#43306,#43307,#43308,#43309,#43310,#43311,#43312,
#43313,#43314,#43315,#43316,#43317,#43318,#43319,#43320,#43321,#43322,#43323,
#43324,#43325,#43326,#43327,#43328,#43329,#43330,#43331,#43332,#43333),
 .UNSPECIFIED.,.F.,.F.)
B_SPLINE_CURVE_WITH_KNOTS((6,1,1,1,1,1,1,1,1,1,1,1,1,1,1,1,1,1,1,1,1,1,
1,1,6),(-0.667078900656922,-0.657142857142857,-0.628571428571429,-0.6,-0.571428571428572,
-0.542857142857143,-0.514285714285714,-0.485714285714286,-0.457142857142857,
-0.428571428571429,-0.4,-0.371428571428571,-0.342857142857143,-0.314285714285714,
-0.285714285714286,-0.257142857142857,-0.228571428571429,-0.2,-0.171428571428571,
-0.142857142857143,-0.114285714285714,-0.0857142857142857,-0.0571428571428571,
-0.0285714285714286,0.),.UNSPECIFIED.)
CURVE()
GEOMETRIC_REPRESENTATION_ITEM()
RATIONAL_B_SPLINE_CURVE((1.,1.,1.,1.,1.,1.,1.,1.,1.,1.,1.,1.,1.,1.,1.,1.,
1.,1.,1.,1.,1.,1.,1.,1.,1.,1.,1.,1.,1.))
REPRESENTATION_ITEM('')
);
#620=(
BOUNDED_CURVE()
B_SPLINE_CURVE(5,(#43363,#43364,#43365,#43366,#43367,#43368,#43369,#43370,
#43371,#43372,#43373,#43374,#43375,#43376,#43377,#43378,#43379,#43380,#43381,
#43382,#43383,#43384,#43385,#43386,#43387,#43388,#43389,#43390,#43391),
 .UNSPECIFIED.,.F.,.F.)
B_SPLINE_CURVE_WITH_KNOTS((6,1,1,1,1,1,1,1,1,1,1,1,1,1,1,1,1,1,1,1,1,1,
1,1,6),(0.,0.0285714285714286,0.0571428571428571,0.0857142857142857,0.114285714285714,
0.142857142857143,0.171428571428571,0.2,0.228571428571429,0.257142857142857,
0.285714285714286,0.314285714285714,0.342857142857143,0.371428571428571,
0.4,0.428571428571429,0.457142857142857,0.485714285714286,0.514285714285714,
0.542857142857143,0.571428571428572,0.6,0.628571428571429,0.657142857142857,
0.667078900656917),.UNSPECIFIED.)
CURVE()
GEOMETRIC_REPRESENTATION_ITEM()
RATIONAL_B_SPLINE_CURVE((1.,1.,1.,1.,1.,1.,1.,1.,1.,1.,1.,1.,1.,1.,1.,1.,
1.,1.,1.,1.,1.,1.,1.,1.,1.,1.,1.,1.,1.))
REPRESENTATION_ITEM('')
);
#621=(
BOUNDED_CURVE()
B_SPLINE_CURVE(5,(#43394,#43395,#43396,#43397,#43398,#43399,#43400,#43401,
#43402,#43403,#43404,#43405,#43406,#43407,#43408,#43409,#43410,#43411,#43412,
#43413,#43414,#43415,#43416,#43417,#43418),.UNSPECIFIED.,.F.,.F.)
B_SPLINE_CURVE_WITH_KNOTS((6,1,1,1,1,1,1,1,1,1,1,1,1,1,1,1,1,1,1,1,6),(0.436331539942223,
0.457142857142857,0.485714285714286,0.514285714285714,0.542857142857143,
0.571428571428572,0.6,0.628571428571429,0.657142857142857,0.685714285714286,
0.714285714285714,0.742857142857143,0.771428571428572,0.8,0.828571428571429,
0.857142857142857,0.885714285714286,0.914285714285714,0.942857142857143,
0.971428571428572,1.),.UNSPECIFIED.)
CURVE()
GEOMETRIC_REPRESENTATION_ITEM()
RATIONAL_B_SPLINE_CURVE((1.,1.,1.,1.,1.,1.,1.,1.,1.,1.,1.,1.,1.,1.,1.,1.,
1.,1.,1.,1.,1.,1.,1.,1.,1.))
REPRESENTATION_ITEM('')
);
#622=(
BOUNDED_CURVE()
B_SPLINE_CURVE(5,(#43507,#43508,#43509,#43510,#43511,#43512,#43513,#43514,
#43515,#43516,#43517,#43518,#43519,#43520,#43521,#43522,#43523,#43524,#43525,
#43526,#43527,#43528,#43529,#43530,#43531),.UNSPECIFIED.,.F.,.F.)
B_SPLINE_CURVE_WITH_KNOTS((6,1,1,1,1,1,1,1,1,1,1,1,1,1,1,1,1,1,1,1,6),(-1.,
-0.971428571428572,-0.942857142857143,-0.914285714285714,-0.885714285714286,
-0.857142857142857,-0.828571428571429,-0.8,-0.771428571428572,-0.742857142857143,
-0.714285714285714,-0.685714285714286,-0.657142857142857,-0.628571428571429,
-0.6,-0.571428571428572,-0.542857142857143,-0.514285714285714,-0.485714285714286,
-0.457142857142857,-0.436331539942219),.UNSPECIFIED.)
CURVE()
GEOMETRIC_REPRESENTATION_ITEM()
RATIONAL_B_SPLINE_CURVE((1.,1.,1.,1.,1.,1.,1.,1.,1.,1.,1.,1.,1.,1.,1.,1.,
1.,1.,1.,1.,1.,1.,1.,1.,1.))
REPRESENTATION_ITEM('')
);
#623=(
BOUNDED_CURVE()
B_SPLINE_CURVE(5,(#43627,#43628,#43629,#43630,#43631,#43632,#43633,#43634,
#43635,#43636,#43637,#43638,#43639,#43640,#43641,#43642,#43643,#43644,#43645,
#43646,#43647,#43648,#43649,#43650,#43651,#43652,#43653,#43654,#43655),
 .UNSPECIFIED.,.F.,.F.)
B_SPLINE_CURVE_WITH_KNOTS((6,1,1,1,1,1,1,1,1,1,1,1,1,1,1,1,1,1,1,1,1,1,
1,1,6),(-0.667078900656922,-0.657142857142857,-0.628571428571429,-0.6,-0.571428571428572,
-0.542857142857143,-0.514285714285714,-0.485714285714286,-0.457142857142857,
-0.428571428571429,-0.4,-0.371428571428571,-0.342857142857143,-0.314285714285714,
-0.285714285714286,-0.257142857142857,-0.228571428571429,-0.2,-0.171428571428571,
-0.142857142857143,-0.114285714285714,-0.0857142857142857,-0.0571428571428571,
-0.0285714285714286,0.),.UNSPECIFIED.)
CURVE()
GEOMETRIC_REPRESENTATION_ITEM()
RATIONAL_B_SPLINE_CURVE((1.,1.,1.,1.,1.,1.,1.,1.,1.,1.,1.,1.,1.,1.,1.,1.,
1.,1.,1.,1.,1.,1.,1.,1.,1.,1.,1.,1.,1.))
REPRESENTATION_ITEM('')
);
#624=(
BOUNDED_CURVE()
B_SPLINE_CURVE(5,(#43685,#43686,#43687,#43688,#43689,#43690,#43691,#43692,
#43693,#43694,#43695,#43696,#43697,#43698,#43699,#43700,#43701,#43702,#43703,
#43704,#43705,#43706,#43707,#43708,#43709,#43710,#43711,#43712,#43713),
 .UNSPECIFIED.,.F.,.F.)
B_SPLINE_CURVE_WITH_KNOTS((6,1,1,1,1,1,1,1,1,1,1,1,1,1,1,1,1,1,1,1,1,1,
1,1,6),(0.,0.0285714285714286,0.0571428571428571,0.0857142857142857,0.114285714285714,
0.142857142857143,0.171428571428571,0.2,0.228571428571429,0.257142857142857,
0.285714285714286,0.314285714285714,0.342857142857143,0.371428571428571,
0.4,0.428571428571429,0.457142857142857,0.485714285714286,0.514285714285714,
0.542857142857143,0.571428571428572,0.6,0.628571428571429,0.657142857142857,
0.667078900656917),.UNSPECIFIED.)
CURVE()
GEOMETRIC_REPRESENTATION_ITEM()
RATIONAL_B_SPLINE_CURVE((1.,1.,1.,1.,1.,1.,1.,1.,1.,1.,1.,1.,1.,1.,1.,1.,
1.,1.,1.,1.,1.,1.,1.,1.,1.,1.,1.,1.,1.))
REPRESENTATION_ITEM('')
);
#625=(
BOUNDED_CURVE()
B_SPLINE_CURVE(5,(#43716,#43717,#43718,#43719,#43720,#43721,#43722,#43723,
#43724,#43725,#43726,#43727,#43728,#43729,#43730,#43731,#43732,#43733,#43734,
#43735,#43736,#43737,#43738,#43739,#43740),.UNSPECIFIED.,.F.,.F.)
B_SPLINE_CURVE_WITH_KNOTS((6,1,1,1,1,1,1,1,1,1,1,1,1,1,1,1,1,1,1,1,6),(0.436331539942223,
0.457142857142857,0.485714285714286,0.514285714285714,0.542857142857143,
0.571428571428572,0.6,0.628571428571429,0.657142857142857,0.685714285714286,
0.714285714285714,0.742857142857143,0.771428571428572,0.8,0.828571428571429,
0.857142857142857,0.885714285714286,0.914285714285714,0.942857142857143,
0.971428571428572,1.),.UNSPECIFIED.)
CURVE()
GEOMETRIC_REPRESENTATION_ITEM()
RATIONAL_B_SPLINE_CURVE((1.,1.,1.,1.,1.,1.,1.,1.,1.,1.,1.,1.,1.,1.,1.,1.,
1.,1.,1.,1.,1.,1.,1.,1.,1.))
REPRESENTATION_ITEM('')
);
#626=(
BOUNDED_CURVE()
B_SPLINE_CURVE(5,(#43829,#43830,#43831,#43832,#43833,#43834,#43835,#43836,
#43837,#43838,#43839,#43840,#43841,#43842,#43843,#43844,#43845,#43846,#43847,
#43848,#43849,#43850,#43851,#43852,#43853),.UNSPECIFIED.,.F.,.F.)
B_SPLINE_CURVE_WITH_KNOTS((6,1,1,1,1,1,1,1,1,1,1,1,1,1,1,1,1,1,1,1,6),(-1.,
-0.971428571428572,-0.942857142857143,-0.914285714285714,-0.885714285714286,
-0.857142857142857,-0.828571428571429,-0.8,-0.771428571428572,-0.742857142857143,
-0.714285714285714,-0.685714285714286,-0.657142857142857,-0.628571428571429,
-0.6,-0.571428571428572,-0.542857142857143,-0.514285714285714,-0.485714285714286,
-0.457142857142857,-0.436331539942219),.UNSPECIFIED.)
CURVE()
GEOMETRIC_REPRESENTATION_ITEM()
RATIONAL_B_SPLINE_CURVE((1.,1.,1.,1.,1.,1.,1.,1.,1.,1.,1.,1.,1.,1.,1.,1.,
1.,1.,1.,1.,1.,1.,1.,1.,1.))
REPRESENTATION_ITEM('')
);
#627=(
BOUNDED_CURVE()
B_SPLINE_CURVE(5,(#43962,#43963,#43964,#43965,#43966,#43967,#43968,#43969,
#43970,#43971,#43972,#43973,#43974,#43975,#43976,#43977,#43978,#43979,#43980,
#43981,#43982,#43983,#43984,#43985,#43986,#43987,#43988,#43989,#43990),
 .UNSPECIFIED.,.F.,.F.)
B_SPLINE_CURVE_WITH_KNOTS((6,1,1,1,1,1,1,1,1,1,1,1,1,1,1,1,1,1,1,1,1,1,
1,1,6),(-0.667078900656922,-0.657142857142857,-0.628571428571429,-0.6,-0.571428571428572,
-0.542857142857143,-0.514285714285714,-0.485714285714286,-0.457142857142857,
-0.428571428571429,-0.4,-0.371428571428571,-0.342857142857143,-0.314285714285714,
-0.285714285714286,-0.257142857142857,-0.228571428571429,-0.2,-0.171428571428571,
-0.142857142857143,-0.114285714285714,-0.0857142857142857,-0.0571428571428571,
-0.0285714285714286,0.),.UNSPECIFIED.)
CURVE()
GEOMETRIC_REPRESENTATION_ITEM()
RATIONAL_B_SPLINE_CURVE((1.,1.,1.,1.,1.,1.,1.,1.,1.,1.,1.,1.,1.,1.,1.,1.,
1.,1.,1.,1.,1.,1.,1.,1.,1.,1.,1.,1.,1.))
REPRESENTATION_ITEM('')
);
#628=(
BOUNDED_CURVE()
B_SPLINE_CURVE(5,(#44020,#44021,#44022,#44023,#44024,#44025,#44026,#44027,
#44028,#44029,#44030,#44031,#44032,#44033,#44034,#44035,#44036,#44037,#44038,
#44039,#44040,#44041,#44042,#44043,#44044,#44045,#44046,#44047,#44048),
 .UNSPECIFIED.,.F.,.F.)
B_SPLINE_CURVE_WITH_KNOTS((6,1,1,1,1,1,1,1,1,1,1,1,1,1,1,1,1,1,1,1,1,1,
1,1,6),(0.,0.0285714285714286,0.0571428571428571,0.0857142857142857,0.114285714285714,
0.142857142857143,0.171428571428571,0.2,0.228571428571429,0.257142857142857,
0.285714285714286,0.314285714285714,0.342857142857143,0.371428571428571,
0.4,0.428571428571429,0.457142857142857,0.485714285714286,0.514285714285714,
0.542857142857143,0.571428571428572,0.6,0.628571428571429,0.657142857142857,
0.667078900656916),.UNSPECIFIED.)
CURVE()
GEOMETRIC_REPRESENTATION_ITEM()
RATIONAL_B_SPLINE_CURVE((1.,1.,1.,1.,1.,1.,1.,1.,1.,1.,1.,1.,1.,1.,1.,1.,
1.,1.,1.,1.,1.,1.,1.,1.,1.,1.,1.,1.,1.))
REPRESENTATION_ITEM('')
);
#629=(
BOUNDED_CURVE()
B_SPLINE_CURVE(5,(#44051,#44052,#44053,#44054,#44055,#44056,#44057,#44058,
#44059,#44060,#44061,#44062,#44063,#44064,#44065,#44066,#44067,#44068,#44069,
#44070,#44071,#44072,#44073,#44074,#44075),.UNSPECIFIED.,.F.,.F.)
B_SPLINE_CURVE_WITH_KNOTS((6,1,1,1,1,1,1,1,1,1,1,1,1,1,1,1,1,1,1,1,6),(0.436331539942223,
0.457142857142857,0.485714285714286,0.514285714285714,0.542857142857143,
0.571428571428572,0.6,0.628571428571429,0.657142857142857,0.685714285714286,
0.714285714285714,0.742857142857143,0.771428571428572,0.8,0.828571428571429,
0.857142857142857,0.885714285714286,0.914285714285714,0.942857142857143,
0.971428571428572,1.),.UNSPECIFIED.)
CURVE()
GEOMETRIC_REPRESENTATION_ITEM()
RATIONAL_B_SPLINE_CURVE((1.,1.,1.,1.,1.,1.,1.,1.,1.,1.,1.,1.,1.,1.,1.,1.,
1.,1.,1.,1.,1.,1.,1.,1.,1.))
REPRESENTATION_ITEM('')
);
#630=(
BOUNDED_CURVE()
B_SPLINE_CURVE(5,(#44164,#44165,#44166,#44167,#44168,#44169,#44170,#44171,
#44172,#44173,#44174,#44175,#44176,#44177,#44178,#44179,#44180,#44181,#44182,
#44183,#44184,#44185,#44186,#44187,#44188),.UNSPECIFIED.,.F.,.F.)
B_SPLINE_CURVE_WITH_KNOTS((6,1,1,1,1,1,1,1,1,1,1,1,1,1,1,1,1,1,1,1,6),(-1.,
-0.971428571428572,-0.942857142857143,-0.914285714285714,-0.885714285714286,
-0.857142857142857,-0.828571428571429,-0.8,-0.771428571428572,-0.742857142857143,
-0.714285714285714,-0.685714285714286,-0.657142857142857,-0.628571428571429,
-0.6,-0.571428571428572,-0.542857142857143,-0.514285714285714,-0.485714285714286,
-0.457142857142857,-0.436331539942219),.UNSPECIFIED.)
CURVE()
GEOMETRIC_REPRESENTATION_ITEM()
RATIONAL_B_SPLINE_CURVE((1.,1.,1.,1.,1.,1.,1.,1.,1.,1.,1.,1.,1.,1.,1.,1.,
1.,1.,1.,1.,1.,1.,1.,1.,1.))
REPRESENTATION_ITEM('')
);
#631=(
BOUNDED_CURVE()
B_SPLINE_CURVE(5,(#44284,#44285,#44286,#44287,#44288,#44289,#44290,#44291,
#44292,#44293,#44294,#44295,#44296,#44297,#44298,#44299,#44300,#44301,#44302,
#44303,#44304,#44305,#44306,#44307,#44308,#44309,#44310,#44311,#44312),
 .UNSPECIFIED.,.F.,.F.)
B_SPLINE_CURVE_WITH_KNOTS((6,1,1,1,1,1,1,1,1,1,1,1,1,1,1,1,1,1,1,1,1,1,
1,1,6),(-0.667078900656921,-0.657142857142857,-0.628571428571429,-0.6,-0.571428571428572,
-0.542857142857143,-0.514285714285714,-0.485714285714286,-0.457142857142857,
-0.428571428571429,-0.4,-0.371428571428571,-0.342857142857143,-0.314285714285714,
-0.285714285714286,-0.257142857142857,-0.228571428571429,-0.2,-0.171428571428571,
-0.142857142857143,-0.114285714285714,-0.0857142857142857,-0.0571428571428571,
-0.0285714285714286,0.),.UNSPECIFIED.)
CURVE()
GEOMETRIC_REPRESENTATION_ITEM()
RATIONAL_B_SPLINE_CURVE((1.,1.,1.,1.,1.,1.,1.,1.,1.,1.,1.,1.,1.,1.,1.,1.,
1.,1.,1.,1.,1.,1.,1.,1.,1.,1.,1.,1.,1.))
REPRESENTATION_ITEM('')
);
#632=(
BOUNDED_CURVE()
B_SPLINE_CURVE(5,(#44342,#44343,#44344,#44345,#44346,#44347,#44348,#44349,
#44350,#44351,#44352,#44353,#44354,#44355,#44356,#44357,#44358,#44359,#44360,
#44361,#44362,#44363,#44364,#44365,#44366,#44367,#44368,#44369,#44370),
 .UNSPECIFIED.,.F.,.F.)
B_SPLINE_CURVE_WITH_KNOTS((6,1,1,1,1,1,1,1,1,1,1,1,1,1,1,1,1,1,1,1,1,1,
1,1,6),(0.,0.0285714285714286,0.0571428571428571,0.0857142857142857,0.114285714285714,
0.142857142857143,0.171428571428571,0.2,0.228571428571429,0.257142857142857,
0.285714285714286,0.314285714285714,0.342857142857143,0.371428571428571,
0.4,0.428571428571429,0.457142857142857,0.485714285714286,0.514285714285714,
0.542857142857143,0.571428571428572,0.6,0.628571428571429,0.657142857142857,
0.667078900656917),.UNSPECIFIED.)
CURVE()
GEOMETRIC_REPRESENTATION_ITEM()
RATIONAL_B_SPLINE_CURVE((1.,1.,1.,1.,1.,1.,1.,1.,1.,1.,1.,1.,1.,1.,1.,1.,
1.,1.,1.,1.,1.,1.,1.,1.,1.,1.,1.,1.,1.))
REPRESENTATION_ITEM('')
);
#633=(
BOUNDED_CURVE()
B_SPLINE_CURVE(5,(#44373,#44374,#44375,#44376,#44377,#44378,#44379,#44380,
#44381,#44382,#44383,#44384,#44385,#44386,#44387,#44388,#44389,#44390,#44391,
#44392,#44393,#44394,#44395,#44396,#44397),.UNSPECIFIED.,.F.,.F.)
B_SPLINE_CURVE_WITH_KNOTS((6,1,1,1,1,1,1,1,1,1,1,1,1,1,1,1,1,1,1,1,6),(0.436331539942223,
0.457142857142857,0.485714285714286,0.514285714285714,0.542857142857143,
0.571428571428572,0.6,0.628571428571429,0.657142857142857,0.685714285714286,
0.714285714285714,0.742857142857143,0.771428571428572,0.8,0.828571428571429,
0.857142857142857,0.885714285714286,0.914285714285714,0.942857142857143,
0.971428571428572,1.),.UNSPECIFIED.)
CURVE()
GEOMETRIC_REPRESENTATION_ITEM()
RATIONAL_B_SPLINE_CURVE((1.,1.,1.,1.,1.,1.,1.,1.,1.,1.,1.,1.,1.,1.,1.,1.,
1.,1.,1.,1.,1.,1.,1.,1.,1.))
REPRESENTATION_ITEM('')
);
#634=(
BOUNDED_CURVE()
B_SPLINE_CURVE(5,(#44486,#44487,#44488,#44489,#44490,#44491,#44492,#44493,
#44494,#44495,#44496,#44497,#44498,#44499,#44500,#44501,#44502,#44503,#44504,
#44505,#44506,#44507,#44508,#44509,#44510),.UNSPECIFIED.,.F.,.F.)
B_SPLINE_CURVE_WITH_KNOTS((6,1,1,1,1,1,1,1,1,1,1,1,1,1,1,1,1,1,1,1,6),(-1.,
-0.971428571428572,-0.942857142857143,-0.914285714285714,-0.885714285714286,
-0.857142857142857,-0.828571428571429,-0.8,-0.771428571428572,-0.742857142857143,
-0.714285714285714,-0.685714285714286,-0.657142857142857,-0.628571428571429,
-0.6,-0.571428571428572,-0.542857142857143,-0.514285714285714,-0.485714285714286,
-0.457142857142857,-0.436331539942219),.UNSPECIFIED.)
CURVE()
GEOMETRIC_REPRESENTATION_ITEM()
RATIONAL_B_SPLINE_CURVE((1.,1.,1.,1.,1.,1.,1.,1.,1.,1.,1.,1.,1.,1.,1.,1.,
1.,1.,1.,1.,1.,1.,1.,1.,1.))
REPRESENTATION_ITEM('')
);
#635=(
BOUNDED_CURVE()
B_SPLINE_CURVE(5,(#44606,#44607,#44608,#44609,#44610,#44611,#44612,#44613,
#44614,#44615,#44616,#44617,#44618,#44619,#44620,#44621,#44622,#44623,#44624,
#44625,#44626,#44627,#44628,#44629,#44630,#44631,#44632,#44633,#44634),
 .UNSPECIFIED.,.F.,.F.)
B_SPLINE_CURVE_WITH_KNOTS((6,1,1,1,1,1,1,1,1,1,1,1,1,1,1,1,1,1,1,1,1,1,
1,1,6),(-0.667078900656922,-0.657142857142857,-0.628571428571429,-0.6,-0.571428571428572,
-0.542857142857143,-0.514285714285714,-0.485714285714286,-0.457142857142857,
-0.428571428571429,-0.4,-0.371428571428571,-0.342857142857143,-0.314285714285714,
-0.285714285714286,-0.257142857142857,-0.228571428571429,-0.2,-0.171428571428571,
-0.142857142857143,-0.114285714285714,-0.0857142857142857,-0.0571428571428571,
-0.0285714285714286,0.),.UNSPECIFIED.)
CURVE()
GEOMETRIC_REPRESENTATION_ITEM()
RATIONAL_B_SPLINE_CURVE((1.,1.,1.,1.,1.,1.,1.,1.,1.,1.,1.,1.,1.,1.,1.,1.,
1.,1.,1.,1.,1.,1.,1.,1.,1.,1.,1.,1.,1.))
REPRESENTATION_ITEM('')
);
#636=(
BOUNDED_CURVE()
B_SPLINE_CURVE(5,(#44666,#44667,#44668,#44669,#44670,#44671,#44672,#44673,
#44674,#44675,#44676,#44677,#44678,#44679,#44680,#44681,#44682,#44683,#44684,
#44685,#44686,#44687,#44688,#44689,#44690,#44691,#44692,#44693,#44694),
 .UNSPECIFIED.,.F.,.F.)
B_SPLINE_CURVE_WITH_KNOTS((6,1,1,1,1,1,1,1,1,1,1,1,1,1,1,1,1,1,1,1,1,1,
1,1,6),(0.,0.0285714285714286,0.0571428571428571,0.0857142857142857,0.114285714285714,
0.142857142857143,0.171428571428571,0.2,0.228571428571429,0.257142857142857,
0.285714285714286,0.314285714285714,0.342857142857143,0.371428571428571,
0.4,0.428571428571429,0.457142857142857,0.485714285714286,0.514285714285714,
0.542857142857143,0.571428571428572,0.6,0.628571428571429,0.657142857142857,
0.667078900656917),.UNSPECIFIED.)
CURVE()
GEOMETRIC_REPRESENTATION_ITEM()
RATIONAL_B_SPLINE_CURVE((1.,1.,1.,1.,1.,1.,1.,1.,1.,1.,1.,1.,1.,1.,1.,1.,
1.,1.,1.,1.,1.,1.,1.,1.,1.,1.,1.,1.,1.))
REPRESENTATION_ITEM('')
);
#637=(
BOUNDED_CURVE()
B_SPLINE_CURVE(5,(#44697,#44698,#44699,#44700,#44701,#44702,#44703,#44704,
#44705,#44706,#44707,#44708,#44709,#44710,#44711,#44712,#44713,#44714,#44715,
#44716,#44717,#44718,#44719,#44720,#44721),.UNSPECIFIED.,.F.,.F.)
B_SPLINE_CURVE_WITH_KNOTS((6,1,1,1,1,1,1,1,1,1,1,1,1,1,1,1,1,1,1,1,6),(0.436331539942224,
0.457142857142857,0.485714285714286,0.514285714285714,0.542857142857143,
0.571428571428572,0.6,0.628571428571429,0.657142857142857,0.685714285714286,
0.714285714285714,0.742857142857143,0.771428571428572,0.8,0.828571428571429,
0.857142857142857,0.885714285714286,0.914285714285714,0.942857142857143,
0.971428571428572,1.),.UNSPECIFIED.)
CURVE()
GEOMETRIC_REPRESENTATION_ITEM()
RATIONAL_B_SPLINE_CURVE((1.,1.,1.,1.,1.,1.,1.,1.,1.,1.,1.,1.,1.,1.,1.,1.,
1.,1.,1.,1.,1.,1.,1.,1.,1.))
REPRESENTATION_ITEM('')
);
#638=(
BOUNDED_CURVE()
B_SPLINE_CURVE(5,(#44812,#44813,#44814,#44815,#44816,#44817,#44818,#44819,
#44820,#44821,#44822,#44823,#44824,#44825,#44826,#44827,#44828,#44829,#44830,
#44831,#44832,#44833,#44834,#44835,#44836),.UNSPECIFIED.,.F.,.F.)
B_SPLINE_CURVE_WITH_KNOTS((6,1,1,1,1,1,1,1,1,1,1,1,1,1,1,1,1,1,1,1,6),(-1.,
-0.971428571428572,-0.942857142857143,-0.914285714285714,-0.885714285714286,
-0.857142857142857,-0.828571428571429,-0.8,-0.771428571428572,-0.742857142857143,
-0.714285714285714,-0.685714285714286,-0.657142857142857,-0.628571428571429,
-0.6,-0.571428571428572,-0.542857142857143,-0.514285714285714,-0.485714285714286,
-0.457142857142857,-0.43633153994222),.UNSPECIFIED.)
CURVE()
GEOMETRIC_REPRESENTATION_ITEM()
RATIONAL_B_SPLINE_CURVE((1.,1.,1.,1.,1.,1.,1.,1.,1.,1.,1.,1.,1.,1.,1.,1.,
1.,1.,1.,1.,1.,1.,1.,1.,1.))
REPRESENTATION_ITEM('')
);
#639=(
BOUNDED_CURVE()
B_SPLINE_CURVE(5,(#44932,#44933,#44934,#44935,#44936,#44937,#44938,#44939,
#44940,#44941,#44942,#44943,#44944,#44945,#44946,#44947,#44948,#44949,#44950,
#44951,#44952,#44953,#44954,#44955,#44956,#44957,#44958,#44959,#44960),
 .UNSPECIFIED.,.F.,.F.)
B_SPLINE_CURVE_WITH_KNOTS((6,1,1,1,1,1,1,1,1,1,1,1,1,1,1,1,1,1,1,1,1,1,
1,1,6),(-0.667078900656922,-0.657142857142857,-0.628571428571429,-0.6,-0.571428571428572,
-0.542857142857143,-0.514285714285714,-0.485714285714286,-0.457142857142857,
-0.428571428571429,-0.4,-0.371428571428571,-0.342857142857143,-0.314285714285714,
-0.285714285714286,-0.257142857142857,-0.228571428571429,-0.2,-0.171428571428571,
-0.142857142857143,-0.114285714285714,-0.0857142857142857,-0.0571428571428571,
-0.0285714285714286,0.),.UNSPECIFIED.)
CURVE()
GEOMETRIC_REPRESENTATION_ITEM()
RATIONAL_B_SPLINE_CURVE((1.,1.,1.,1.,1.,1.,1.,1.,1.,1.,1.,1.,1.,1.,1.,1.,
1.,1.,1.,1.,1.,1.,1.,1.,1.,1.,1.,1.,1.))
REPRESENTATION_ITEM('')
);
#640=(
BOUNDED_CURVE()
B_SPLINE_CURVE(5,(#44992,#44993,#44994,#44995,#44996,#44997,#44998,#44999,
#45000,#45001,#45002,#45003,#45004,#45005,#45006,#45007,#45008,#45009,#45010,
#45011,#45012,#45013,#45014,#45015,#45016,#45017,#45018,#45019,#45020),
 .UNSPECIFIED.,.F.,.F.)
B_SPLINE_CURVE_WITH_KNOTS((6,1,1,1,1,1,1,1,1,1,1,1,1,1,1,1,1,1,1,1,1,1,
1,1,6),(0.,0.0285714285714286,0.0571428571428571,0.0857142857142857,0.114285714285714,
0.142857142857143,0.171428571428571,0.2,0.228571428571429,0.257142857142857,
0.285714285714286,0.314285714285714,0.342857142857143,0.371428571428571,
0.4,0.428571428571429,0.457142857142857,0.485714285714286,0.514285714285714,
0.542857142857143,0.571428571428572,0.6,0.628571428571429,0.657142857142857,
0.667078900656917),.UNSPECIFIED.)
CURVE()
GEOMETRIC_REPRESENTATION_ITEM()
RATIONAL_B_SPLINE_CURVE((1.,1.,1.,1.,1.,1.,1.,1.,1.,1.,1.,1.,1.,1.,1.,1.,
1.,1.,1.,1.,1.,1.,1.,1.,1.,1.,1.,1.,1.))
REPRESENTATION_ITEM('')
);
#641=(
BOUNDED_CURVE()
B_SPLINE_CURVE(5,(#45023,#45024,#45025,#45026,#45027,#45028,#45029,#45030,
#45031,#45032,#45033,#45034,#45035,#45036,#45037,#45038,#45039,#45040,#45041,
#45042,#45043,#45044,#45045,#45046,#45047),.UNSPECIFIED.,.F.,.F.)
B_SPLINE_CURVE_WITH_KNOTS((6,1,1,1,1,1,1,1,1,1,1,1,1,1,1,1,1,1,1,1,6),(0.436331539942223,
0.457142857142857,0.485714285714286,0.514285714285714,0.542857142857143,
0.571428571428572,0.6,0.628571428571429,0.657142857142857,0.685714285714286,
0.714285714285714,0.742857142857143,0.771428571428572,0.8,0.828571428571429,
0.857142857142857,0.885714285714286,0.914285714285714,0.942857142857143,
0.971428571428572,1.),.UNSPECIFIED.)
CURVE()
GEOMETRIC_REPRESENTATION_ITEM()
RATIONAL_B_SPLINE_CURVE((1.,1.,1.,1.,1.,1.,1.,1.,1.,1.,1.,1.,1.,1.,1.,1.,
1.,1.,1.,1.,1.,1.,1.,1.,1.))
REPRESENTATION_ITEM('')
);
#642=(
BOUNDED_CURVE()
B_SPLINE_CURVE(5,(#45136,#45137,#45138,#45139,#45140,#45141,#45142,#45143,
#45144,#45145,#45146,#45147,#45148,#45149,#45150,#45151,#45152,#45153,#45154,
#45155,#45156,#45157,#45158,#45159,#45160),.UNSPECIFIED.,.F.,.F.)
B_SPLINE_CURVE_WITH_KNOTS((6,1,1,1,1,1,1,1,1,1,1,1,1,1,1,1,1,1,1,1,6),(-1.,
-0.971428571428572,-0.942857142857143,-0.914285714285714,-0.885714285714286,
-0.857142857142857,-0.828571428571429,-0.8,-0.771428571428572,-0.742857142857143,
-0.714285714285714,-0.685714285714286,-0.657142857142857,-0.628571428571429,
-0.6,-0.571428571428572,-0.542857142857143,-0.514285714285714,-0.485714285714286,
-0.457142857142857,-0.436331539942219),.UNSPECIFIED.)
CURVE()
GEOMETRIC_REPRESENTATION_ITEM()
RATIONAL_B_SPLINE_CURVE((1.,1.,1.,1.,1.,1.,1.,1.,1.,1.,1.,1.,1.,1.,1.,1.,
1.,1.,1.,1.,1.,1.,1.,1.,1.))
REPRESENTATION_ITEM('')
);
#643=(
BOUNDED_CURVE()
B_SPLINE_CURVE(5,(#45256,#45257,#45258,#45259,#45260,#45261,#45262,#45263,
#45264,#45265,#45266,#45267,#45268,#45269,#45270,#45271,#45272,#45273,#45274,
#45275,#45276,#45277,#45278,#45279,#45280,#45281,#45282,#45283,#45284),
 .UNSPECIFIED.,.F.,.F.)
B_SPLINE_CURVE_WITH_KNOTS((6,1,1,1,1,1,1,1,1,1,1,1,1,1,1,1,1,1,1,1,1,1,
1,1,6),(-0.667078900656922,-0.657142857142857,-0.628571428571429,-0.6,-0.571428571428572,
-0.542857142857143,-0.514285714285714,-0.485714285714286,-0.457142857142857,
-0.428571428571429,-0.4,-0.371428571428571,-0.342857142857143,-0.314285714285714,
-0.285714285714286,-0.257142857142857,-0.228571428571429,-0.2,-0.171428571428571,
-0.142857142857143,-0.114285714285714,-0.0857142857142857,-0.0571428571428571,
-0.0285714285714286,0.),.UNSPECIFIED.)
CURVE()
GEOMETRIC_REPRESENTATION_ITEM()
RATIONAL_B_SPLINE_CURVE((1.,1.,1.,1.,1.,1.,1.,1.,1.,1.,1.,1.,1.,1.,1.,1.,
1.,1.,1.,1.,1.,1.,1.,1.,1.,1.,1.,1.,1.))
REPRESENTATION_ITEM('')
);
#644=(
BOUNDED_CURVE()
B_SPLINE_CURVE(5,(#45314,#45315,#45316,#45317,#45318,#45319,#45320,#45321,
#45322,#45323,#45324,#45325,#45326,#45327,#45328,#45329,#45330,#45331,#45332,
#45333,#45334,#45335,#45336,#45337,#45338,#45339,#45340,#45341,#45342),
 .UNSPECIFIED.,.F.,.F.)
B_SPLINE_CURVE_WITH_KNOTS((6,1,1,1,1,1,1,1,1,1,1,1,1,1,1,1,1,1,1,1,1,1,
1,1,6),(0.,0.0285714285714286,0.0571428571428571,0.0857142857142857,0.114285714285714,
0.142857142857143,0.171428571428571,0.2,0.228571428571429,0.257142857142857,
0.285714285714286,0.314285714285714,0.342857142857143,0.371428571428571,
0.4,0.428571428571429,0.457142857142857,0.485714285714286,0.514285714285714,
0.542857142857143,0.571428571428572,0.6,0.628571428571429,0.657142857142857,
0.667078900656917),.UNSPECIFIED.)
CURVE()
GEOMETRIC_REPRESENTATION_ITEM()
RATIONAL_B_SPLINE_CURVE((1.,1.,1.,1.,1.,1.,1.,1.,1.,1.,1.,1.,1.,1.,1.,1.,
1.,1.,1.,1.,1.,1.,1.,1.,1.,1.,1.,1.,1.))
REPRESENTATION_ITEM('')
);
#645=(
BOUNDED_CURVE()
B_SPLINE_CURVE(5,(#45345,#45346,#45347,#45348,#45349,#45350,#45351,#45352,
#45353,#45354,#45355,#45356,#45357,#45358,#45359,#45360,#45361,#45362,#45363,
#45364,#45365,#45366,#45367,#45368,#45369),.UNSPECIFIED.,.F.,.F.)
B_SPLINE_CURVE_WITH_KNOTS((6,1,1,1,1,1,1,1,1,1,1,1,1,1,1,1,1,1,1,1,6),(0.436331539942223,
0.457142857142857,0.485714285714286,0.514285714285714,0.542857142857143,
0.571428571428572,0.6,0.628571428571429,0.657142857142857,0.685714285714286,
0.714285714285714,0.742857142857143,0.771428571428572,0.8,0.828571428571429,
0.857142857142857,0.885714285714286,0.914285714285714,0.942857142857143,
0.971428571428572,1.),.UNSPECIFIED.)
CURVE()
GEOMETRIC_REPRESENTATION_ITEM()
RATIONAL_B_SPLINE_CURVE((1.,1.,1.,1.,1.,1.,1.,1.,1.,1.,1.,1.,1.,1.,1.,1.,
1.,1.,1.,1.,1.,1.,1.,1.,1.))
REPRESENTATION_ITEM('')
);
#646=(
BOUNDED_CURVE()
B_SPLINE_CURVE(5,(#45458,#45459,#45460,#45461,#45462,#45463,#45464,#45465,
#45466,#45467,#45468,#45469,#45470,#45471,#45472,#45473,#45474,#45475,#45476,
#45477,#45478,#45479,#45480,#45481,#45482),.UNSPECIFIED.,.F.,.F.)
B_SPLINE_CURVE_WITH_KNOTS((6,1,1,1,1,1,1,1,1,1,1,1,1,1,1,1,1,1,1,1,6),(-1.,
-0.971428571428572,-0.942857142857143,-0.914285714285714,-0.885714285714286,
-0.857142857142857,-0.828571428571429,-0.8,-0.771428571428572,-0.742857142857143,
-0.714285714285714,-0.685714285714286,-0.657142857142857,-0.628571428571429,
-0.6,-0.571428571428572,-0.542857142857143,-0.514285714285714,-0.485714285714286,
-0.457142857142857,-0.436331539942219),.UNSPECIFIED.)
CURVE()
GEOMETRIC_REPRESENTATION_ITEM()
RATIONAL_B_SPLINE_CURVE((1.,1.,1.,1.,1.,1.,1.,1.,1.,1.,1.,1.,1.,1.,1.,1.,
1.,1.,1.,1.,1.,1.,1.,1.,1.))
REPRESENTATION_ITEM('')
);
#647=(
BOUNDED_CURVE()
B_SPLINE_CURVE(5,(#45578,#45579,#45580,#45581,#45582,#45583,#45584,#45585,
#45586,#45587,#45588,#45589,#45590,#45591,#45592,#45593,#45594,#45595,#45596,
#45597,#45598,#45599,#45600,#45601,#45602,#45603,#45604,#45605,#45606),
 .UNSPECIFIED.,.F.,.F.)
B_SPLINE_CURVE_WITH_KNOTS((6,1,1,1,1,1,1,1,1,1,1,1,1,1,1,1,1,1,1,1,1,1,
1,1,6),(-0.667078900656922,-0.657142857142857,-0.628571428571429,-0.6,-0.571428571428572,
-0.542857142857143,-0.514285714285714,-0.485714285714286,-0.457142857142857,
-0.428571428571429,-0.4,-0.371428571428571,-0.342857142857143,-0.314285714285714,
-0.285714285714286,-0.257142857142857,-0.228571428571429,-0.2,-0.171428571428571,
-0.142857142857143,-0.114285714285714,-0.0857142857142857,-0.0571428571428571,
-0.0285714285714286,0.),.UNSPECIFIED.)
CURVE()
GEOMETRIC_REPRESENTATION_ITEM()
RATIONAL_B_SPLINE_CURVE((1.,1.,1.,1.,1.,1.,1.,1.,1.,1.,1.,1.,1.,1.,1.,1.,
1.,1.,1.,1.,1.,1.,1.,1.,1.,1.,1.,1.,1.))
REPRESENTATION_ITEM('')
);
#648=(
BOUNDED_CURVE()
B_SPLINE_CURVE(5,(#45636,#45637,#45638,#45639,#45640,#45641,#45642,#45643,
#45644,#45645,#45646,#45647,#45648,#45649,#45650,#45651,#45652,#45653,#45654,
#45655,#45656,#45657,#45658,#45659,#45660,#45661,#45662,#45663,#45664),
 .UNSPECIFIED.,.F.,.F.)
B_SPLINE_CURVE_WITH_KNOTS((6,1,1,1,1,1,1,1,1,1,1,1,1,1,1,1,1,1,1,1,1,1,
1,1,6),(0.,0.0285714285714286,0.0571428571428571,0.0857142857142857,0.114285714285714,
0.142857142857143,0.171428571428571,0.2,0.228571428571429,0.257142857142857,
0.285714285714286,0.314285714285714,0.342857142857143,0.371428571428571,
0.4,0.428571428571429,0.457142857142857,0.485714285714286,0.514285714285714,
0.542857142857143,0.571428571428572,0.6,0.628571428571429,0.657142857142857,
0.667078900656917),.UNSPECIFIED.)
CURVE()
GEOMETRIC_REPRESENTATION_ITEM()
RATIONAL_B_SPLINE_CURVE((1.,1.,1.,1.,1.,1.,1.,1.,1.,1.,1.,1.,1.,1.,1.,1.,
1.,1.,1.,1.,1.,1.,1.,1.,1.,1.,1.,1.,1.))
REPRESENTATION_ITEM('')
);
#649=(
BOUNDED_CURVE()
B_SPLINE_CURVE(5,(#45667,#45668,#45669,#45670,#45671,#45672,#45673,#45674,
#45675,#45676,#45677,#45678,#45679,#45680,#45681,#45682,#45683,#45684,#45685,
#45686,#45687,#45688,#45689,#45690,#45691),.UNSPECIFIED.,.F.,.F.)
B_SPLINE_CURVE_WITH_KNOTS((6,1,1,1,1,1,1,1,1,1,1,1,1,1,1,1,1,1,1,1,6),(0.436331539942223,
0.457142857142857,0.485714285714286,0.514285714285714,0.542857142857143,
0.571428571428572,0.6,0.628571428571429,0.657142857142857,0.685714285714286,
0.714285714285714,0.742857142857143,0.771428571428572,0.8,0.828571428571429,
0.857142857142857,0.885714285714286,0.914285714285714,0.942857142857143,
0.971428571428572,1.),.UNSPECIFIED.)
CURVE()
GEOMETRIC_REPRESENTATION_ITEM()
RATIONAL_B_SPLINE_CURVE((1.,1.,1.,1.,1.,1.,1.,1.,1.,1.,1.,1.,1.,1.,1.,1.,
1.,1.,1.,1.,1.,1.,1.,1.,1.))
REPRESENTATION_ITEM('')
);
#650=(
BOUNDED_CURVE()
B_SPLINE_CURVE(5,(#45780,#45781,#45782,#45783,#45784,#45785,#45786,#45787,
#45788,#45789,#45790,#45791,#45792,#45793,#45794,#45795,#45796,#45797,#45798,
#45799,#45800,#45801,#45802,#45803,#45804),.UNSPECIFIED.,.F.,.F.)
B_SPLINE_CURVE_WITH_KNOTS((6,1,1,1,1,1,1,1,1,1,1,1,1,1,1,1,1,1,1,1,6),(-1.,
-0.971428571428572,-0.942857142857143,-0.914285714285714,-0.885714285714286,
-0.857142857142857,-0.828571428571429,-0.8,-0.771428571428572,-0.742857142857143,
-0.714285714285714,-0.685714285714286,-0.657142857142857,-0.628571428571429,
-0.6,-0.571428571428572,-0.542857142857143,-0.514285714285714,-0.485714285714286,
-0.457142857142857,-0.436331539942219),.UNSPECIFIED.)
CURVE()
GEOMETRIC_REPRESENTATION_ITEM()
RATIONAL_B_SPLINE_CURVE((1.,1.,1.,1.,1.,1.,1.,1.,1.,1.,1.,1.,1.,1.,1.,1.,
1.,1.,1.,1.,1.,1.,1.,1.,1.))
REPRESENTATION_ITEM('')
);
#651=(
BOUNDED_CURVE()
B_SPLINE_CURVE(5,(#45900,#45901,#45902,#45903,#45904,#45905,#45906,#45907,
#45908,#45909,#45910,#45911,#45912,#45913,#45914,#45915,#45916,#45917,#45918,
#45919,#45920,#45921,#45922,#45923,#45924,#45925,#45926,#45927,#45928),
 .UNSPECIFIED.,.F.,.F.)
B_SPLINE_CURVE_WITH_KNOTS((6,1,1,1,1,1,1,1,1,1,1,1,1,1,1,1,1,1,1,1,1,1,
1,1,6),(-0.667078900656922,-0.657142857142857,-0.628571428571429,-0.6,-0.571428571428572,
-0.542857142857143,-0.514285714285714,-0.485714285714286,-0.457142857142857,
-0.428571428571429,-0.4,-0.371428571428571,-0.342857142857143,-0.314285714285714,
-0.285714285714286,-0.257142857142857,-0.228571428571429,-0.2,-0.171428571428571,
-0.142857142857143,-0.114285714285714,-0.0857142857142857,-0.0571428571428571,
-0.0285714285714286,0.),.UNSPECIFIED.)
CURVE()
GEOMETRIC_REPRESENTATION_ITEM()
RATIONAL_B_SPLINE_CURVE((1.,1.,1.,1.,1.,1.,1.,1.,1.,1.,1.,1.,1.,1.,1.,1.,
1.,1.,1.,1.,1.,1.,1.,1.,1.,1.,1.,1.,1.))
REPRESENTATION_ITEM('')
);
#652=(
BOUNDED_CURVE()
B_SPLINE_CURVE(5,(#45964,#45965,#45966,#45967,#45968,#45969,#45970,#45971,
#45972,#45973,#45974,#45975,#45976,#45977,#45978,#45979,#45980,#45981,#45982,
#45983,#45984,#45985,#45986,#45987,#45988,#45989,#45990,#45991,#45992),
 .UNSPECIFIED.,.F.,.F.)
B_SPLINE_CURVE_WITH_KNOTS((6,1,1,1,1,1,1,1,1,1,1,1,1,1,1,1,1,1,1,1,1,1,
1,1,6),(0.,0.0285714285714286,0.0571428571428571,0.0857142857142857,0.114285714285714,
0.142857142857143,0.171428571428571,0.2,0.228571428571429,0.257142857142857,
0.285714285714286,0.314285714285714,0.342857142857143,0.371428571428571,
0.4,0.428571428571429,0.457142857142857,0.485714285714286,0.514285714285714,
0.542857142857143,0.571428571428572,0.6,0.628571428571429,0.657142857142857,
0.667078900656916),.UNSPECIFIED.)
CURVE()
GEOMETRIC_REPRESENTATION_ITEM()
RATIONAL_B_SPLINE_CURVE((1.,1.,1.,1.,1.,1.,1.,1.,1.,1.,1.,1.,1.,1.,1.,1.,
1.,1.,1.,1.,1.,1.,1.,1.,1.,1.,1.,1.,1.))
REPRESENTATION_ITEM('')
);
#653=(
BOUNDED_CURVE()
B_SPLINE_CURVE(5,(#45995,#45996,#45997,#45998,#45999,#46000,#46001,#46002,
#46003,#46004,#46005,#46006,#46007,#46008,#46009,#46010,#46011,#46012,#46013,
#46014,#46015,#46016,#46017,#46018,#46019),.UNSPECIFIED.,.F.,.F.)
B_SPLINE_CURVE_WITH_KNOTS((6,1,1,1,1,1,1,1,1,1,1,1,1,1,1,1,1,1,1,1,6),(0.436331539942224,
0.457142857142857,0.485714285714286,0.514285714285714,0.542857142857143,
0.571428571428572,0.6,0.628571428571429,0.657142857142857,0.685714285714286,
0.714285714285714,0.742857142857143,0.771428571428572,0.8,0.828571428571429,
0.857142857142857,0.885714285714286,0.914285714285714,0.942857142857143,
0.971428571428572,1.),.UNSPECIFIED.)
CURVE()
GEOMETRIC_REPRESENTATION_ITEM()
RATIONAL_B_SPLINE_CURVE((1.,1.,1.,1.,1.,1.,1.,1.,1.,1.,1.,1.,1.,1.,1.,1.,
1.,1.,1.,1.,1.,1.,1.,1.,1.))
REPRESENTATION_ITEM('')
);
#654=(
BOUNDED_CURVE()
B_SPLINE_CURVE(5,(#46108,#46109,#46110,#46111,#46112,#46113,#46114,#46115,
#46116,#46117,#46118,#46119,#46120,#46121,#46122,#46123,#46124,#46125,#46126,
#46127,#46128,#46129,#46130,#46131,#46132),.UNSPECIFIED.,.F.,.F.)
B_SPLINE_CURVE_WITH_KNOTS((6,1,1,1,1,1,1,1,1,1,1,1,1,1,1,1,1,1,1,1,6),(-1.,
-0.971428571428572,-0.942857142857143,-0.914285714285714,-0.885714285714286,
-0.857142857142857,-0.828571428571429,-0.8,-0.771428571428572,-0.742857142857143,
-0.714285714285714,-0.685714285714286,-0.657142857142857,-0.628571428571429,
-0.6,-0.571428571428572,-0.542857142857143,-0.514285714285714,-0.485714285714286,
-0.457142857142857,-0.43633153994222),.UNSPECIFIED.)
CURVE()
GEOMETRIC_REPRESENTATION_ITEM()
RATIONAL_B_SPLINE_CURVE((1.,1.,1.,1.,1.,1.,1.,1.,1.,1.,1.,1.,1.,1.,1.,1.,
1.,1.,1.,1.,1.,1.,1.,1.,1.))
REPRESENTATION_ITEM('')
);
#655=(
BOUNDED_CURVE()
B_SPLINE_CURVE(5,(#46228,#46229,#46230,#46231,#46232,#46233,#46234,#46235,
#46236,#46237,#46238,#46239,#46240,#46241,#46242,#46243,#46244,#46245,#46246,
#46247,#46248,#46249,#46250,#46251,#46252,#46253,#46254,#46255,#46256),
 .UNSPECIFIED.,.F.,.F.)
B_SPLINE_CURVE_WITH_KNOTS((6,1,1,1,1,1,1,1,1,1,1,1,1,1,1,1,1,1,1,1,1,1,
1,1,6),(-0.667078900656921,-0.657142857142857,-0.628571428571429,-0.6,-0.571428571428572,
-0.542857142857143,-0.514285714285714,-0.485714285714286,-0.457142857142857,
-0.428571428571429,-0.4,-0.371428571428571,-0.342857142857143,-0.314285714285714,
-0.285714285714286,-0.257142857142857,-0.228571428571429,-0.2,-0.171428571428571,
-0.142857142857143,-0.114285714285714,-0.0857142857142857,-0.0571428571428571,
-0.0285714285714286,0.),.UNSPECIFIED.)
CURVE()
GEOMETRIC_REPRESENTATION_ITEM()
RATIONAL_B_SPLINE_CURVE((1.,1.,1.,1.,1.,1.,1.,1.,1.,1.,1.,1.,1.,1.,1.,1.,
1.,1.,1.,1.,1.,1.,1.,1.,1.,1.,1.,1.,1.))
REPRESENTATION_ITEM('')
);
#656=(
BOUNDED_CURVE()
B_SPLINE_CURVE(5,(#46286,#46287,#46288,#46289,#46290,#46291,#46292,#46293,
#46294,#46295,#46296,#46297,#46298,#46299,#46300,#46301,#46302,#46303,#46304,
#46305,#46306,#46307,#46308,#46309,#46310,#46311,#46312,#46313,#46314),
 .UNSPECIFIED.,.F.,.F.)
B_SPLINE_CURVE_WITH_KNOTS((6,1,1,1,1,1,1,1,1,1,1,1,1,1,1,1,1,1,1,1,1,1,
1,1,6),(0.,0.0285714285714286,0.0571428571428571,0.0857142857142857,0.114285714285714,
0.142857142857143,0.171428571428571,0.2,0.228571428571429,0.257142857142857,
0.285714285714286,0.314285714285714,0.342857142857143,0.371428571428571,
0.4,0.428571428571429,0.457142857142857,0.485714285714286,0.514285714285714,
0.542857142857143,0.571428571428572,0.6,0.628571428571429,0.657142857142857,
0.667078900656917),.UNSPECIFIED.)
CURVE()
GEOMETRIC_REPRESENTATION_ITEM()
RATIONAL_B_SPLINE_CURVE((1.,1.,1.,1.,1.,1.,1.,1.,1.,1.,1.,1.,1.,1.,1.,1.,
1.,1.,1.,1.,1.,1.,1.,1.,1.,1.,1.,1.,1.))
REPRESENTATION_ITEM('')
);
#657=(
BOUNDED_CURVE()
B_SPLINE_CURVE(5,(#46317,#46318,#46319,#46320,#46321,#46322,#46323,#46324,
#46325,#46326,#46327,#46328,#46329,#46330,#46331,#46332,#46333,#46334,#46335,
#46336,#46337,#46338,#46339,#46340,#46341),.UNSPECIFIED.,.F.,.F.)
B_SPLINE_CURVE_WITH_KNOTS((6,1,1,1,1,1,1,1,1,1,1,1,1,1,1,1,1,1,1,1,6),(0.436331539942224,
0.457142857142857,0.485714285714286,0.514285714285714,0.542857142857143,
0.571428571428572,0.6,0.628571428571429,0.657142857142857,0.685714285714286,
0.714285714285714,0.742857142857143,0.771428571428572,0.8,0.828571428571429,
0.857142857142857,0.885714285714286,0.914285714285714,0.942857142857143,
0.971428571428572,1.),.UNSPECIFIED.)
CURVE()
GEOMETRIC_REPRESENTATION_ITEM()
RATIONAL_B_SPLINE_CURVE((1.,1.,1.,1.,1.,1.,1.,1.,1.,1.,1.,1.,1.,1.,1.,1.,
1.,1.,1.,1.,1.,1.,1.,1.,1.))
REPRESENTATION_ITEM('')
);
#658=(
BOUNDED_CURVE()
B_SPLINE_CURVE(5,(#46430,#46431,#46432,#46433,#46434,#46435,#46436,#46437,
#46438,#46439,#46440,#46441,#46442,#46443,#46444,#46445,#46446,#46447,#46448,
#46449,#46450,#46451,#46452,#46453,#46454),.UNSPECIFIED.,.F.,.F.)
B_SPLINE_CURVE_WITH_KNOTS((6,1,1,1,1,1,1,1,1,1,1,1,1,1,1,1,1,1,1,1,6),(-1.,
-0.971428571428572,-0.942857142857143,-0.914285714285714,-0.885714285714286,
-0.857142857142857,-0.828571428571429,-0.8,-0.771428571428572,-0.742857142857143,
-0.714285714285714,-0.685714285714286,-0.657142857142857,-0.628571428571429,
-0.6,-0.571428571428572,-0.542857142857143,-0.514285714285714,-0.485714285714286,
-0.457142857142857,-0.43633153994222),.UNSPECIFIED.)
CURVE()
GEOMETRIC_REPRESENTATION_ITEM()
RATIONAL_B_SPLINE_CURVE((1.,1.,1.,1.,1.,1.,1.,1.,1.,1.,1.,1.,1.,1.,1.,1.,
1.,1.,1.,1.,1.,1.,1.,1.,1.))
REPRESENTATION_ITEM('')
);
#659=(
BOUNDED_CURVE()
B_SPLINE_CURVE(5,(#46550,#46551,#46552,#46553,#46554,#46555,#46556,#46557,
#46558,#46559,#46560,#46561,#46562,#46563,#46564,#46565,#46566,#46567,#46568,
#46569,#46570,#46571,#46572,#46573,#46574,#46575,#46576,#46577,#46578),
 .UNSPECIFIED.,.F.,.F.)
B_SPLINE_CURVE_WITH_KNOTS((6,1,1,1,1,1,1,1,1,1,1,1,1,1,1,1,1,1,1,1,1,1,
1,1,6),(-0.667078900656921,-0.657142857142857,-0.628571428571429,-0.6,-0.571428571428572,
-0.542857142857143,-0.514285714285714,-0.485714285714286,-0.457142857142857,
-0.428571428571429,-0.4,-0.371428571428571,-0.342857142857143,-0.314285714285714,
-0.285714285714286,-0.257142857142857,-0.228571428571429,-0.2,-0.171428571428571,
-0.142857142857143,-0.114285714285714,-0.0857142857142857,-0.0571428571428571,
-0.0285714285714286,0.),.UNSPECIFIED.)
CURVE()
GEOMETRIC_REPRESENTATION_ITEM()
RATIONAL_B_SPLINE_CURVE((1.,1.,1.,1.,1.,1.,1.,1.,1.,1.,1.,1.,1.,1.,1.,1.,
1.,1.,1.,1.,1.,1.,1.,1.,1.,1.,1.,1.,1.))
REPRESENTATION_ITEM('')
);
#660=(
BOUNDED_CURVE()
B_SPLINE_CURVE(5,(#46608,#46609,#46610,#46611,#46612,#46613,#46614,#46615,
#46616,#46617,#46618,#46619,#46620,#46621,#46622,#46623,#46624,#46625,#46626,
#46627,#46628,#46629,#46630,#46631,#46632,#46633,#46634,#46635,#46636),
 .UNSPECIFIED.,.F.,.F.)
B_SPLINE_CURVE_WITH_KNOTS((6,1,1,1,1,1,1,1,1,1,1,1,1,1,1,1,1,1,1,1,1,1,
1,1,6),(0.,0.0285714285714286,0.0571428571428571,0.0857142857142857,0.114285714285714,
0.142857142857143,0.171428571428571,0.2,0.228571428571429,0.257142857142857,
0.285714285714286,0.314285714285714,0.342857142857143,0.371428571428571,
0.4,0.428571428571429,0.457142857142857,0.485714285714286,0.514285714285714,
0.542857142857143,0.571428571428572,0.6,0.628571428571429,0.657142857142857,
0.667078900656917),.UNSPECIFIED.)
CURVE()
GEOMETRIC_REPRESENTATION_ITEM()
RATIONAL_B_SPLINE_CURVE((1.,1.,1.,1.,1.,1.,1.,1.,1.,1.,1.,1.,1.,1.,1.,1.,
1.,1.,1.,1.,1.,1.,1.,1.,1.,1.,1.,1.,1.))
REPRESENTATION_ITEM('')
);
#661=(
BOUNDED_CURVE()
B_SPLINE_CURVE(5,(#46639,#46640,#46641,#46642,#46643,#46644,#46645,#46646,
#46647,#46648,#46649,#46650,#46651,#46652,#46653,#46654,#46655,#46656,#46657,
#46658,#46659,#46660,#46661,#46662,#46663),.UNSPECIFIED.,.F.,.F.)
B_SPLINE_CURVE_WITH_KNOTS((6,1,1,1,1,1,1,1,1,1,1,1,1,1,1,1,1,1,1,1,6),(0.436331539942223,
0.457142857142857,0.485714285714286,0.514285714285714,0.542857142857143,
0.571428571428572,0.6,0.628571428571429,0.657142857142857,0.685714285714286,
0.714285714285714,0.742857142857143,0.771428571428572,0.8,0.828571428571429,
0.857142857142857,0.885714285714286,0.914285714285714,0.942857142857143,
0.971428571428572,1.),.UNSPECIFIED.)
CURVE()
GEOMETRIC_REPRESENTATION_ITEM()
RATIONAL_B_SPLINE_CURVE((1.,1.,1.,1.,1.,1.,1.,1.,1.,1.,1.,1.,1.,1.,1.,1.,
1.,1.,1.,1.,1.,1.,1.,1.,1.))
REPRESENTATION_ITEM('')
);
#662=(
BOUNDED_CURVE()
B_SPLINE_CURVE(5,(#46752,#46753,#46754,#46755,#46756,#46757,#46758,#46759,
#46760,#46761,#46762,#46763,#46764,#46765,#46766,#46767,#46768,#46769,#46770,
#46771,#46772,#46773,#46774,#46775,#46776),.UNSPECIFIED.,.F.,.F.)
B_SPLINE_CURVE_WITH_KNOTS((6,1,1,1,1,1,1,1,1,1,1,1,1,1,1,1,1,1,1,1,6),(-1.,
-0.971428571428572,-0.942857142857143,-0.914285714285714,-0.885714285714286,
-0.857142857142857,-0.828571428571429,-0.8,-0.771428571428572,-0.742857142857143,
-0.714285714285714,-0.685714285714286,-0.657142857142857,-0.628571428571429,
-0.6,-0.571428571428572,-0.542857142857143,-0.514285714285714,-0.485714285714286,
-0.457142857142857,-0.436331539942219),.UNSPECIFIED.)
CURVE()
GEOMETRIC_REPRESENTATION_ITEM()
RATIONAL_B_SPLINE_CURVE((1.,1.,1.,1.,1.,1.,1.,1.,1.,1.,1.,1.,1.,1.,1.,1.,
1.,1.,1.,1.,1.,1.,1.,1.,1.))
REPRESENTATION_ITEM('')
);
#663=(
BOUNDED_CURVE()
B_SPLINE_CURVE(5,(#46872,#46873,#46874,#46875,#46876,#46877,#46878,#46879,
#46880,#46881,#46882,#46883,#46884,#46885,#46886,#46887,#46888,#46889,#46890,
#46891,#46892,#46893,#46894,#46895,#46896,#46897,#46898,#46899,#46900),
 .UNSPECIFIED.,.F.,.F.)
B_SPLINE_CURVE_WITH_KNOTS((6,1,1,1,1,1,1,1,1,1,1,1,1,1,1,1,1,1,1,1,1,1,
1,1,6),(-0.667078900656922,-0.657142857142857,-0.628571428571429,-0.6,-0.571428571428572,
-0.542857142857143,-0.514285714285714,-0.485714285714286,-0.457142857142857,
-0.428571428571429,-0.4,-0.371428571428571,-0.342857142857143,-0.314285714285714,
-0.285714285714286,-0.257142857142857,-0.228571428571429,-0.2,-0.171428571428571,
-0.142857142857143,-0.114285714285714,-0.0857142857142857,-0.0571428571428571,
-0.0285714285714286,0.),.UNSPECIFIED.)
CURVE()
GEOMETRIC_REPRESENTATION_ITEM()
RATIONAL_B_SPLINE_CURVE((1.,1.,1.,1.,1.,1.,1.,1.,1.,1.,1.,1.,1.,1.,1.,1.,
1.,1.,1.,1.,1.,1.,1.,1.,1.,1.,1.,1.,1.))
REPRESENTATION_ITEM('')
);
#664=(
BOUNDED_CURVE()
B_SPLINE_CURVE(5,(#47007,#47008,#47009,#47010,#47011,#47012,#47013,#47014,
#47015,#47016,#47017,#47018,#47019,#47020,#47021,#47022,#47023,#47024,#47025,
#47026,#47027,#47028,#47029,#47030,#47031,#47032,#47033,#47034,#47035),
 .UNSPECIFIED.,.F.,.F.)
B_SPLINE_CURVE_WITH_KNOTS((6,1,1,1,1,1,1,1,1,1,1,1,1,1,1,1,1,1,1,1,1,1,
1,1,6),(-0.667078900656922,-0.657142857142857,-0.628571428571429,-0.6,-0.571428571428572,
-0.542857142857143,-0.514285714285714,-0.485714285714286,-0.457142857142857,
-0.428571428571429,-0.4,-0.371428571428571,-0.342857142857143,-0.314285714285714,
-0.285714285714286,-0.257142857142857,-0.228571428571429,-0.2,-0.171428571428571,
-0.142857142857143,-0.114285714285714,-0.0857142857142857,-0.0571428571428571,
-0.0285714285714286,0.),.UNSPECIFIED.)
CURVE()
GEOMETRIC_REPRESENTATION_ITEM()
RATIONAL_B_SPLINE_CURVE((1.,1.,1.,1.,1.,1.,1.,1.,1.,1.,1.,1.,1.,1.,1.,1.,
1.,1.,1.,1.,1.,1.,1.,1.,1.,1.,1.,1.,1.))
REPRESENTATION_ITEM('')
);
#665=(
BOUNDED_CURVE()
B_SPLINE_CURVE(5,(#47038,#47039,#47040,#47041,#47042,#47043,#47044,#47045,
#47046,#47047,#47048,#47049,#47050,#47051,#47052,#47053,#47054,#47055,#47056,
#47057,#47058,#47059,#47060,#47061,#47062,#47063,#47064,#47065,#47066),
 .UNSPECIFIED.,.F.,.F.)
B_SPLINE_CURVE_WITH_KNOTS((6,1,1,1,1,1,1,1,1,1,1,1,1,1,1,1,1,1,1,1,1,1,
1,1,6),(0.,0.0285714285714286,0.0571428571428571,0.0857142857142857,0.114285714285714,
0.142857142857143,0.171428571428571,0.2,0.228571428571429,0.257142857142857,
0.285714285714286,0.314285714285714,0.342857142857143,0.371428571428571,
0.4,0.428571428571429,0.457142857142857,0.485714285714286,0.514285714285714,
0.542857142857143,0.571428571428572,0.6,0.628571428571429,0.657142857142857,
0.667078900656918),.UNSPECIFIED.)
CURVE()
GEOMETRIC_REPRESENTATION_ITEM()
RATIONAL_B_SPLINE_CURVE((1.,1.,1.,1.,1.,1.,1.,1.,1.,1.,1.,1.,1.,1.,1.,1.,
1.,1.,1.,1.,1.,1.,1.,1.,1.,1.,1.,1.,1.))
REPRESENTATION_ITEM('')
);
#666=(
BOUNDED_CURVE()
B_SPLINE_CURVE(5,(#47071,#47072,#47073,#47074,#47075,#47076,#47077,#47078,
#47079,#47080,#47081,#47082,#47083,#47084,#47085,#47086,#47087,#47088,#47089,
#47090,#47091,#47092,#47093,#47094,#47095),.UNSPECIFIED.,.F.,.F.)
B_SPLINE_CURVE_WITH_KNOTS((6,1,1,1,1,1,1,1,1,1,1,1,1,1,1,1,1,1,1,1,6),(0.436331539942222,
0.457142857142857,0.485714285714286,0.514285714285714,0.542857142857143,
0.571428571428572,0.6,0.628571428571429,0.657142857142857,0.685714285714286,
0.714285714285714,0.742857142857143,0.771428571428572,0.8,0.828571428571429,
0.857142857142857,0.885714285714286,0.914285714285714,0.942857142857143,
0.971428571428572,1.),.UNSPECIFIED.)
CURVE()
GEOMETRIC_REPRESENTATION_ITEM()
RATIONAL_B_SPLINE_CURVE((1.,1.,1.,1.,1.,1.,1.,1.,1.,1.,1.,1.,1.,1.,1.,1.,
1.,1.,1.,1.,1.,1.,1.,1.,1.))
REPRESENTATION_ITEM('')
);
#667=(
BOUNDED_CURVE()
B_SPLINE_CURVE(5,(#47192,#47193,#47194,#47195,#47196,#47197,#47198,#47199,
#47200,#47201,#47202,#47203,#47204,#47205,#47206,#47207,#47208,#47209,#47210,
#47211,#47212,#47213,#47214,#47215,#47216),.UNSPECIFIED.,.F.,.F.)
B_SPLINE_CURVE_WITH_KNOTS((6,1,1,1,1,1,1,1,1,1,1,1,1,1,1,1,1,1,1,1,6),(-1.,
-0.971428571428572,-0.942857142857143,-0.914285714285714,-0.885714285714286,
-0.857142857142857,-0.828571428571429,-0.8,-0.771428571428572,-0.742857142857143,
-0.714285714285714,-0.685714285714286,-0.657142857142857,-0.628571428571429,
-0.6,-0.571428571428572,-0.542857142857143,-0.514285714285714,-0.485714285714286,
-0.457142857142857,-0.436331539942219),.UNSPECIFIED.)
CURVE()
GEOMETRIC_REPRESENTATION_ITEM()
RATIONAL_B_SPLINE_CURVE((1.,1.,1.,1.,1.,1.,1.,1.,1.,1.,1.,1.,1.,1.,1.,1.,
1.,1.,1.,1.,1.,1.,1.,1.,1.))
REPRESENTATION_ITEM('')
);
#668=(
BOUNDED_CURVE()
B_SPLINE_CURVE(2,(#48216,#48217,#48218),.UNSPECIFIED.,.F.,.F.)
B_SPLINE_CURVE_WITH_KNOTS((3,3),(0.026389951333147,0.0542823820564139),
 .UNSPECIFIED.)
CURVE()
GEOMETRIC_REPRESENTATION_ITEM()
RATIONAL_B_SPLINE_CURVE((1.00002935554076,1.00004146705942,1.00004638738564))
REPRESENTATION_ITEM('')
);
#669=(
BOUNDED_CURVE()
B_SPLINE_CURVE(2,(#48349,#48350,#48351),.UNSPECIFIED.,.F.,.F.)
B_SPLINE_CURVE_WITH_KNOTS((3,3),(0.0263899513331846,0.0542823820564278),
 .UNSPECIFIED.)
CURVE()
GEOMETRIC_REPRESENTATION_ITEM()
RATIONAL_B_SPLINE_CURVE((1.00002935553973,1.00004146705796,1.00004638738401))
REPRESENTATION_ITEM('')
);
#670=(
BOUNDED_CURVE()
B_SPLINE_CURVE(2,(#49013,#49014,#49015),.UNSPECIFIED.,.F.,.F.)
B_SPLINE_CURVE_WITH_KNOTS((3,3),(0.355039941373883,0.455385686797418),
 .UNSPECIFIED.)
CURVE()
GEOMETRIC_REPRESENTATION_ITEM()
RATIONAL_B_SPLINE_CURVE((1.00817025780825,1.00909081812274,1.00987909016891))
REPRESENTATION_ITEM('')
);
#671=(
BOUNDED_CURVE()
B_SPLINE_CURVE(2,(#49128,#49129,#49130),.UNSPECIFIED.,.F.,.F.)
B_SPLINE_CURVE_WITH_KNOTS((3,3),(1.65125508748907,1.7516008329126),
 .UNSPECIFIED.)
CURVE()
GEOMETRIC_REPRESENTATION_ITEM()
RATIONAL_B_SPLINE_CURVE((1.00987909016891,1.00909081812274,1.00817025780825))
REPRESENTATION_ITEM('')
);
#672=(
BOUNDED_CURVE()
B_SPLINE_CURVE(5,(#49245,#49246,#49247,#49248,#49249,#49250,#49251,#49252,
#49253,#49254,#49255,#49256,#49257,#49258,#49259,#49260,#49261,#49262,#49263,
#49264,#49265,#49266,#49267,#49268,#49269),.UNSPECIFIED.,.F.,.F.)
B_SPLINE_CURVE_WITH_KNOTS((6,1,1,1,1,1,1,1,1,1,1,1,1,1,1,1,1,1,1,1,6),(0.437678095034471,
0.457142857142857,0.485714285714286,0.514285714285714,0.542857142857143,
0.571428571428572,0.6,0.628571428571429,0.657142857142857,0.685714285714286,
0.714285714285714,0.742857142857143,0.771428571428572,0.8,0.828571428571429,
0.857142857142857,0.885714285714286,0.914285714285714,0.942857142857143,
0.971428571428572,1.),.UNSPECIFIED.)
CURVE()
GEOMETRIC_REPRESENTATION_ITEM()
RATIONAL_B_SPLINE_CURVE((1.,1.,1.,1.,1.,1.,1.,1.,1.,1.,1.,1.,1.,1.,1.,1.,
1.,1.,1.,1.,1.,1.,1.,1.,1.))
REPRESENTATION_ITEM('')
);
#673=(
BOUNDED_CURVE()
B_SPLINE_CURVE(5,(#49273,#49274,#49275,#49276,#49277,#49278,#49279,#49280,
#49281,#49282,#49283,#49284,#49285,#49286,#49287,#49288,#49289,#49290,#49291,
#49292,#49293,#49294,#49295,#49296,#49297,#49298,#49299,#49300,#49301),
 .UNSPECIFIED.,.F.,.F.)
B_SPLINE_CURVE_WITH_KNOTS((6,1,1,1,1,1,1,1,1,1,1,1,1,1,1,1,1,1,1,1,1,1,
1,1,6),(0.,0.0285714285714286,0.0571428571428571,0.0857142857142857,0.114285714285714,
0.142857142857143,0.171428571428571,0.2,0.228571428571429,0.257142857142857,
0.285714285714286,0.314285714285714,0.342857142857143,0.371428571428571,
0.4,0.428571428571429,0.457142857142857,0.485714285714286,0.514285714285714,
0.542857142857143,0.571428571428572,0.6,0.628571428571429,0.657142857142857,
0.666463158655954),.UNSPECIFIED.)
CURVE()
GEOMETRIC_REPRESENTATION_ITEM()
RATIONAL_B_SPLINE_CURVE((1.,1.,1.,1.,1.,1.,1.,1.,1.,1.,1.,1.,1.,1.,1.,1.,
1.,1.,1.,1.,1.,1.,1.,1.,1.,1.,1.,1.,1.))
REPRESENTATION_ITEM('')
);
#674=(
BOUNDED_CURVE()
B_SPLINE_CURVE(5,(#49305,#49306,#49307,#49308,#49309,#49310,#49311,#49312,
#49313,#49314,#49315,#49316,#49317,#49318,#49319,#49320,#49321,#49322,#49323,
#49324,#49325,#49326,#49327,#49328,#49329),.UNSPECIFIED.,.F.,.F.)
B_SPLINE_CURVE_WITH_KNOTS((6,1,1,1,1,1,1,1,1,1,1,1,1,1,1,1,1,1,1,1,6),(0.437678095034471,
0.457142857142857,0.485714285714286,0.514285714285714,0.542857142857143,
0.571428571428572,0.6,0.628571428571429,0.657142857142857,0.685714285714286,
0.714285714285714,0.742857142857143,0.771428571428572,0.8,0.828571428571429,
0.857142857142857,0.885714285714286,0.914285714285714,0.942857142857143,
0.971428571428572,1.),.UNSPECIFIED.)
CURVE()
GEOMETRIC_REPRESENTATION_ITEM()
RATIONAL_B_SPLINE_CURVE((1.,1.,1.,1.,1.,1.,1.,1.,1.,1.,1.,1.,1.,1.,1.,1.,
1.,1.,1.,1.,1.,1.,1.,1.,1.))
REPRESENTATION_ITEM('')
);
#675=(
BOUNDED_CURVE()
B_SPLINE_CURVE(5,(#49333,#49334,#49335,#49336,#49337,#49338,#49339,#49340,
#49341,#49342,#49343,#49344,#49345,#49346,#49347,#49348,#49349,#49350,#49351,
#49352,#49353,#49354,#49355,#49356,#49357,#49358,#49359,#49360,#49361),
 .UNSPECIFIED.,.F.,.F.)
B_SPLINE_CURVE_WITH_KNOTS((6,1,1,1,1,1,1,1,1,1,1,1,1,1,1,1,1,1,1,1,1,1,
1,1,6),(0.,0.0285714285714286,0.0571428571428571,0.0857142857142857,0.114285714285714,
0.142857142857143,0.171428571428571,0.2,0.228571428571429,0.257142857142857,
0.285714285714286,0.314285714285714,0.342857142857143,0.371428571428571,
0.4,0.428571428571429,0.457142857142857,0.485714285714286,0.514285714285714,
0.542857142857143,0.571428571428572,0.6,0.628571428571429,0.657142857142857,
0.666463158655954),.UNSPECIFIED.)
CURVE()
GEOMETRIC_REPRESENTATION_ITEM()
RATIONAL_B_SPLINE_CURVE((1.,1.,1.,1.,1.,1.,1.,1.,1.,1.,1.,1.,1.,1.,1.,1.,
1.,1.,1.,1.,1.,1.,1.,1.,1.,1.,1.,1.,1.))
REPRESENTATION_ITEM('')
);
#676=(
BOUNDED_CURVE()
B_SPLINE_CURVE(5,(#49365,#49366,#49367,#49368,#49369,#49370,#49371,#49372,
#49373,#49374,#49375,#49376,#49377,#49378,#49379,#49380,#49381,#49382,#49383,
#49384,#49385,#49386,#49387,#49388,#49389),.UNSPECIFIED.,.F.,.F.)
B_SPLINE_CURVE_WITH_KNOTS((6,1,1,1,1,1,1,1,1,1,1,1,1,1,1,1,1,1,1,1,6),(0.437678095034471,
0.457142857142857,0.485714285714286,0.514285714285714,0.542857142857143,
0.571428571428572,0.6,0.628571428571429,0.657142857142857,0.685714285714286,
0.714285714285714,0.742857142857143,0.771428571428572,0.8,0.828571428571429,
0.857142857142857,0.885714285714286,0.914285714285714,0.942857142857143,
0.971428571428572,1.),.UNSPECIFIED.)
CURVE()
GEOMETRIC_REPRESENTATION_ITEM()
RATIONAL_B_SPLINE_CURVE((1.,1.,1.,1.,1.,1.,1.,1.,1.,1.,1.,1.,1.,1.,1.,1.,
1.,1.,1.,1.,1.,1.,1.,1.,1.))
REPRESENTATION_ITEM('')
);
#677=(
BOUNDED_CURVE()
B_SPLINE_CURVE(5,(#49393,#49394,#49395,#49396,#49397,#49398,#49399,#49400,
#49401,#49402,#49403,#49404,#49405,#49406,#49407,#49408,#49409,#49410,#49411,
#49412,#49413,#49414,#49415,#49416,#49417,#49418,#49419,#49420,#49421),
 .UNSPECIFIED.,.F.,.F.)
B_SPLINE_CURVE_WITH_KNOTS((6,1,1,1,1,1,1,1,1,1,1,1,1,1,1,1,1,1,1,1,1,1,
1,1,6),(0.,0.0285714285714286,0.0571428571428571,0.0857142857142857,0.114285714285714,
0.142857142857143,0.171428571428571,0.2,0.228571428571429,0.257142857142857,
0.285714285714286,0.314285714285714,0.342857142857143,0.371428571428571,
0.4,0.428571428571429,0.457142857142857,0.485714285714286,0.514285714285714,
0.542857142857143,0.571428571428572,0.6,0.628571428571429,0.657142857142857,
0.666463158655955),.UNSPECIFIED.)
CURVE()
GEOMETRIC_REPRESENTATION_ITEM()
RATIONAL_B_SPLINE_CURVE((1.,1.,1.,1.,1.,1.,1.,1.,1.,1.,1.,1.,1.,1.,1.,1.,
1.,1.,1.,1.,1.,1.,1.,1.,1.,1.,1.,1.,1.))
REPRESENTATION_ITEM('')
);
#678=(
BOUNDED_CURVE()
B_SPLINE_CURVE(5,(#49425,#49426,#49427,#49428,#49429,#49430,#49431,#49432,
#49433,#49434,#49435,#49436,#49437,#49438,#49439,#49440,#49441,#49442,#49443,
#49444,#49445,#49446,#49447,#49448,#49449),.UNSPECIFIED.,.F.,.F.)
B_SPLINE_CURVE_WITH_KNOTS((6,1,1,1,1,1,1,1,1,1,1,1,1,1,1,1,1,1,1,1,6),(0.437678095034471,
0.457142857142857,0.485714285714286,0.514285714285714,0.542857142857143,
0.571428571428572,0.6,0.628571428571429,0.657142857142857,0.685714285714286,
0.714285714285714,0.742857142857143,0.771428571428572,0.8,0.828571428571429,
0.857142857142857,0.885714285714286,0.914285714285714,0.942857142857143,
0.971428571428572,1.),.UNSPECIFIED.)
CURVE()
GEOMETRIC_REPRESENTATION_ITEM()
RATIONAL_B_SPLINE_CURVE((1.,1.,1.,1.,1.,1.,1.,1.,1.,1.,1.,1.,1.,1.,1.,1.,
1.,1.,1.,1.,1.,1.,1.,1.,1.))
REPRESENTATION_ITEM('')
);
#679=(
BOUNDED_CURVE()
B_SPLINE_CURVE(5,(#49453,#49454,#49455,#49456,#49457,#49458,#49459,#49460,
#49461,#49462,#49463,#49464,#49465,#49466,#49467,#49468,#49469,#49470,#49471,
#49472,#49473,#49474,#49475,#49476,#49477,#49478,#49479,#49480,#49481),
 .UNSPECIFIED.,.F.,.F.)
B_SPLINE_CURVE_WITH_KNOTS((6,1,1,1,1,1,1,1,1,1,1,1,1,1,1,1,1,1,1,1,1,1,
1,1,6),(0.,0.0285714285714286,0.0571428571428571,0.0857142857142857,0.114285714285714,
0.142857142857143,0.171428571428571,0.2,0.228571428571429,0.257142857142857,
0.285714285714286,0.314285714285714,0.342857142857143,0.371428571428571,
0.4,0.428571428571429,0.457142857142857,0.485714285714286,0.514285714285714,
0.542857142857143,0.571428571428572,0.6,0.628571428571429,0.657142857142857,
0.666463158655954),.UNSPECIFIED.)
CURVE()
GEOMETRIC_REPRESENTATION_ITEM()
RATIONAL_B_SPLINE_CURVE((1.,1.,1.,1.,1.,1.,1.,1.,1.,1.,1.,1.,1.,1.,1.,1.,
1.,1.,1.,1.,1.,1.,1.,1.,1.,1.,1.,1.,1.))
REPRESENTATION_ITEM('')
);
#680=(
BOUNDED_CURVE()
B_SPLINE_CURVE(5,(#49485,#49486,#49487,#49488,#49489,#49490,#49491,#49492,
#49493,#49494,#49495,#49496,#49497,#49498,#49499,#49500,#49501,#49502,#49503,
#49504,#49505,#49506,#49507,#49508,#49509),.UNSPECIFIED.,.F.,.F.)
B_SPLINE_CURVE_WITH_KNOTS((6,1,1,1,1,1,1,1,1,1,1,1,1,1,1,1,1,1,1,1,6),(0.437678095034471,
0.457142857142857,0.485714285714286,0.514285714285714,0.542857142857143,
0.571428571428572,0.6,0.628571428571429,0.657142857142857,0.685714285714286,
0.714285714285714,0.742857142857143,0.771428571428572,0.8,0.828571428571429,
0.857142857142857,0.885714285714286,0.914285714285714,0.942857142857143,
0.971428571428572,1.),.UNSPECIFIED.)
CURVE()
GEOMETRIC_REPRESENTATION_ITEM()
RATIONAL_B_SPLINE_CURVE((1.,1.,1.,1.,1.,1.,1.,1.,1.,1.,1.,1.,1.,1.,1.,1.,
1.,1.,1.,1.,1.,1.,1.,1.,1.))
REPRESENTATION_ITEM('')
);
#681=(
BOUNDED_CURVE()
B_SPLINE_CURVE(5,(#49513,#49514,#49515,#49516,#49517,#49518,#49519,#49520,
#49521,#49522,#49523,#49524,#49525,#49526,#49527,#49528,#49529,#49530,#49531,
#49532,#49533,#49534,#49535,#49536,#49537,#49538,#49539,#49540,#49541),
 .UNSPECIFIED.,.F.,.F.)
B_SPLINE_CURVE_WITH_KNOTS((6,1,1,1,1,1,1,1,1,1,1,1,1,1,1,1,1,1,1,1,1,1,
1,1,6),(0.,0.0285714285714286,0.0571428571428571,0.0857142857142857,0.114285714285714,
0.142857142857143,0.171428571428571,0.2,0.228571428571429,0.257142857142857,
0.285714285714286,0.314285714285714,0.342857142857143,0.371428571428571,
0.4,0.428571428571429,0.457142857142857,0.485714285714286,0.514285714285714,
0.542857142857143,0.571428571428572,0.6,0.628571428571429,0.657142857142857,
0.666463158655954),.UNSPECIFIED.)
CURVE()
GEOMETRIC_REPRESENTATION_ITEM()
RATIONAL_B_SPLINE_CURVE((1.,1.,1.,1.,1.,1.,1.,1.,1.,1.,1.,1.,1.,1.,1.,1.,
1.,1.,1.,1.,1.,1.,1.,1.,1.,1.,1.,1.,1.))
REPRESENTATION_ITEM('')
);
#682=(
BOUNDED_CURVE()
B_SPLINE_CURVE(5,(#49545,#49546,#49547,#49548,#49549,#49550,#49551,#49552,
#49553,#49554,#49555,#49556,#49557,#49558,#49559,#49560,#49561,#49562,#49563,
#49564,#49565,#49566,#49567,#49568,#49569),.UNSPECIFIED.,.F.,.F.)
B_SPLINE_CURVE_WITH_KNOTS((6,1,1,1,1,1,1,1,1,1,1,1,1,1,1,1,1,1,1,1,6),(0.437678095034471,
0.457142857142857,0.485714285714286,0.514285714285714,0.542857142857143,
0.571428571428572,0.6,0.628571428571429,0.657142857142857,0.685714285714286,
0.714285714285714,0.742857142857143,0.771428571428572,0.8,0.828571428571429,
0.857142857142857,0.885714285714286,0.914285714285714,0.942857142857143,
0.971428571428572,1.),.UNSPECIFIED.)
CURVE()
GEOMETRIC_REPRESENTATION_ITEM()
RATIONAL_B_SPLINE_CURVE((1.,1.,1.,1.,1.,1.,1.,1.,1.,1.,1.,1.,1.,1.,1.,1.,
1.,1.,1.,1.,1.,1.,1.,1.,1.))
REPRESENTATION_ITEM('')
);
#683=(
BOUNDED_CURVE()
B_SPLINE_CURVE(5,(#49573,#49574,#49575,#49576,#49577,#49578,#49579,#49580,
#49581,#49582,#49583,#49584,#49585,#49586,#49587,#49588,#49589,#49590,#49591,
#49592,#49593,#49594,#49595,#49596,#49597,#49598,#49599,#49600,#49601),
 .UNSPECIFIED.,.F.,.F.)
B_SPLINE_CURVE_WITH_KNOTS((6,1,1,1,1,1,1,1,1,1,1,1,1,1,1,1,1,1,1,1,1,1,
1,1,6),(0.,0.0285714285714286,0.0571428571428571,0.0857142857142857,0.114285714285714,
0.142857142857143,0.171428571428571,0.2,0.228571428571429,0.257142857142857,
0.285714285714286,0.314285714285714,0.342857142857143,0.371428571428571,
0.4,0.428571428571429,0.457142857142857,0.485714285714286,0.514285714285714,
0.542857142857143,0.571428571428572,0.6,0.628571428571429,0.657142857142857,
0.666463158655954),.UNSPECIFIED.)
CURVE()
GEOMETRIC_REPRESENTATION_ITEM()
RATIONAL_B_SPLINE_CURVE((1.,1.,1.,1.,1.,1.,1.,1.,1.,1.,1.,1.,1.,1.,1.,1.,
1.,1.,1.,1.,1.,1.,1.,1.,1.,1.,1.,1.,1.))
REPRESENTATION_ITEM('')
);
#684=(
BOUNDED_CURVE()
B_SPLINE_CURVE(5,(#49605,#49606,#49607,#49608,#49609,#49610,#49611,#49612,
#49613,#49614,#49615,#49616,#49617,#49618,#49619,#49620,#49621,#49622,#49623,
#49624,#49625,#49626,#49627,#49628,#49629),.UNSPECIFIED.,.F.,.F.)
B_SPLINE_CURVE_WITH_KNOTS((6,1,1,1,1,1,1,1,1,1,1,1,1,1,1,1,1,1,1,1,6),(0.437678095034471,
0.457142857142857,0.485714285714286,0.514285714285714,0.542857142857143,
0.571428571428572,0.6,0.628571428571429,0.657142857142857,0.685714285714286,
0.714285714285714,0.742857142857143,0.771428571428572,0.8,0.828571428571429,
0.857142857142857,0.885714285714286,0.914285714285714,0.942857142857143,
0.971428571428572,1.),.UNSPECIFIED.)
CURVE()
GEOMETRIC_REPRESENTATION_ITEM()
RATIONAL_B_SPLINE_CURVE((1.,1.,1.,1.,1.,1.,1.,1.,1.,1.,1.,1.,1.,1.,1.,1.,
1.,1.,1.,1.,1.,1.,1.,1.,1.))
REPRESENTATION_ITEM('')
);
#685=(
BOUNDED_CURVE()
B_SPLINE_CURVE(5,(#49633,#49634,#49635,#49636,#49637,#49638,#49639,#49640,
#49641,#49642,#49643,#49644,#49645,#49646,#49647,#49648,#49649,#49650,#49651,
#49652,#49653,#49654,#49655,#49656,#49657,#49658,#49659,#49660,#49661),
 .UNSPECIFIED.,.F.,.F.)
B_SPLINE_CURVE_WITH_KNOTS((6,1,1,1,1,1,1,1,1,1,1,1,1,1,1,1,1,1,1,1,1,1,
1,1,6),(0.,0.0285714285714286,0.0571428571428571,0.0857142857142857,0.114285714285714,
0.142857142857143,0.171428571428571,0.2,0.228571428571429,0.257142857142857,
0.285714285714286,0.314285714285714,0.342857142857143,0.371428571428571,
0.4,0.428571428571429,0.457142857142857,0.485714285714286,0.514285714285714,
0.542857142857143,0.571428571428572,0.6,0.628571428571429,0.657142857142857,
0.666463158655955),.UNSPECIFIED.)
CURVE()
GEOMETRIC_REPRESENTATION_ITEM()
RATIONAL_B_SPLINE_CURVE((1.,1.,1.,1.,1.,1.,1.,1.,1.,1.,1.,1.,1.,1.,1.,1.,
1.,1.,1.,1.,1.,1.,1.,1.,1.,1.,1.,1.,1.))
REPRESENTATION_ITEM('')
);
#686=(
BOUNDED_CURVE()
B_SPLINE_CURVE(5,(#49665,#49666,#49667,#49668,#49669,#49670,#49671,#49672,
#49673,#49674,#49675,#49676,#49677,#49678,#49679,#49680,#49681,#49682,#49683,
#49684,#49685,#49686,#49687,#49688,#49689),.UNSPECIFIED.,.F.,.F.)
B_SPLINE_CURVE_WITH_KNOTS((6,1,1,1,1,1,1,1,1,1,1,1,1,1,1,1,1,1,1,1,6),(0.437678095034471,
0.457142857142857,0.485714285714286,0.514285714285714,0.542857142857143,
0.571428571428572,0.6,0.628571428571429,0.657142857142857,0.685714285714286,
0.714285714285714,0.742857142857143,0.771428571428572,0.8,0.828571428571429,
0.857142857142857,0.885714285714286,0.914285714285714,0.942857142857143,
0.971428571428572,1.),.UNSPECIFIED.)
CURVE()
GEOMETRIC_REPRESENTATION_ITEM()
RATIONAL_B_SPLINE_CURVE((1.,1.,1.,1.,1.,1.,1.,1.,1.,1.,1.,1.,1.,1.,1.,1.,
1.,1.,1.,1.,1.,1.,1.,1.,1.))
REPRESENTATION_ITEM('')
);
#687=(
BOUNDED_CURVE()
B_SPLINE_CURVE(5,(#49693,#49694,#49695,#49696,#49697,#49698,#49699,#49700,
#49701,#49702,#49703,#49704,#49705,#49706,#49707,#49708,#49709,#49710,#49711,
#49712,#49713,#49714,#49715,#49716,#49717,#49718,#49719,#49720,#49721),
 .UNSPECIFIED.,.F.,.F.)
B_SPLINE_CURVE_WITH_KNOTS((6,1,1,1,1,1,1,1,1,1,1,1,1,1,1,1,1,1,1,1,1,1,
1,1,6),(0.,0.0285714285714286,0.0571428571428571,0.0857142857142857,0.114285714285714,
0.142857142857143,0.171428571428571,0.2,0.228571428571429,0.257142857142857,
0.285714285714286,0.314285714285714,0.342857142857143,0.371428571428571,
0.4,0.428571428571429,0.457142857142857,0.485714285714286,0.514285714285714,
0.542857142857143,0.571428571428572,0.6,0.628571428571429,0.657142857142857,
0.666463158655954),.UNSPECIFIED.)
CURVE()
GEOMETRIC_REPRESENTATION_ITEM()
RATIONAL_B_SPLINE_CURVE((1.,1.,1.,1.,1.,1.,1.,1.,1.,1.,1.,1.,1.,1.,1.,1.,
1.,1.,1.,1.,1.,1.,1.,1.,1.,1.,1.,1.,1.))
REPRESENTATION_ITEM('')
);
#688=(
BOUNDED_CURVE()
B_SPLINE_CURVE(5,(#49725,#49726,#49727,#49728,#49729,#49730,#49731,#49732,
#49733,#49734,#49735,#49736,#49737,#49738,#49739,#49740,#49741,#49742,#49743,
#49744,#49745,#49746,#49747,#49748,#49749),.UNSPECIFIED.,.F.,.F.)
B_SPLINE_CURVE_WITH_KNOTS((6,1,1,1,1,1,1,1,1,1,1,1,1,1,1,1,1,1,1,1,6),(0.437678095034471,
0.457142857142857,0.485714285714286,0.514285714285714,0.542857142857143,
0.571428571428572,0.6,0.628571428571429,0.657142857142857,0.685714285714286,
0.714285714285714,0.742857142857143,0.771428571428572,0.8,0.828571428571429,
0.857142857142857,0.885714285714286,0.914285714285714,0.942857142857143,
0.971428571428572,1.),.UNSPECIFIED.)
CURVE()
GEOMETRIC_REPRESENTATION_ITEM()
RATIONAL_B_SPLINE_CURVE((1.,1.,1.,1.,1.,1.,1.,1.,1.,1.,1.,1.,1.,1.,1.,1.,
1.,1.,1.,1.,1.,1.,1.,1.,1.))
REPRESENTATION_ITEM('')
);
#689=(
BOUNDED_CURVE()
B_SPLINE_CURVE(5,(#49753,#49754,#49755,#49756,#49757,#49758,#49759,#49760,
#49761,#49762,#49763,#49764,#49765,#49766,#49767,#49768,#49769,#49770,#49771,
#49772,#49773,#49774,#49775,#49776,#49777,#49778,#49779,#49780,#49781),
 .UNSPECIFIED.,.F.,.F.)
B_SPLINE_CURVE_WITH_KNOTS((6,1,1,1,1,1,1,1,1,1,1,1,1,1,1,1,1,1,1,1,1,1,
1,1,6),(0.,0.0285714285714286,0.0571428571428571,0.0857142857142857,0.114285714285714,
0.142857142857143,0.171428571428571,0.2,0.228571428571429,0.257142857142857,
0.285714285714286,0.314285714285714,0.342857142857143,0.371428571428571,
0.4,0.428571428571429,0.457142857142857,0.485714285714286,0.514285714285714,
0.542857142857143,0.571428571428572,0.6,0.628571428571429,0.657142857142857,
0.666463158655955),.UNSPECIFIED.)
CURVE()
GEOMETRIC_REPRESENTATION_ITEM()
RATIONAL_B_SPLINE_CURVE((1.,1.,1.,1.,1.,1.,1.,1.,1.,1.,1.,1.,1.,1.,1.,1.,
1.,1.,1.,1.,1.,1.,1.,1.,1.,1.,1.,1.,1.))
REPRESENTATION_ITEM('')
);
#690=(
BOUNDED_CURVE()
B_SPLINE_CURVE(5,(#49785,#49786,#49787,#49788,#49789,#49790,#49791,#49792,
#49793,#49794,#49795,#49796,#49797,#49798,#49799,#49800,#49801,#49802,#49803,
#49804,#49805,#49806,#49807,#49808,#49809),.UNSPECIFIED.,.F.,.F.)
B_SPLINE_CURVE_WITH_KNOTS((6,1,1,1,1,1,1,1,1,1,1,1,1,1,1,1,1,1,1,1,6),(0.437678095034471,
0.457142857142857,0.485714285714286,0.514285714285714,0.542857142857143,
0.571428571428572,0.6,0.628571428571429,0.657142857142857,0.685714285714286,
0.714285714285714,0.742857142857143,0.771428571428572,0.8,0.828571428571429,
0.857142857142857,0.885714285714286,0.914285714285714,0.942857142857143,
0.971428571428572,1.),.UNSPECIFIED.)
CURVE()
GEOMETRIC_REPRESENTATION_ITEM()
RATIONAL_B_SPLINE_CURVE((1.,1.,1.,1.,1.,1.,1.,1.,1.,1.,1.,1.,1.,1.,1.,1.,
1.,1.,1.,1.,1.,1.,1.,1.,1.))
REPRESENTATION_ITEM('')
);
#691=(
BOUNDED_CURVE()
B_SPLINE_CURVE(5,(#49813,#49814,#49815,#49816,#49817,#49818,#49819,#49820,
#49821,#49822,#49823,#49824,#49825,#49826,#49827,#49828,#49829,#49830,#49831,
#49832,#49833,#49834,#49835,#49836,#49837,#49838,#49839,#49840,#49841),
 .UNSPECIFIED.,.F.,.F.)
B_SPLINE_CURVE_WITH_KNOTS((6,1,1,1,1,1,1,1,1,1,1,1,1,1,1,1,1,1,1,1,1,1,
1,1,6),(0.,0.0285714285714286,0.0571428571428571,0.0857142857142857,0.114285714285714,
0.142857142857143,0.171428571428571,0.2,0.228571428571429,0.257142857142857,
0.285714285714286,0.314285714285714,0.342857142857143,0.371428571428571,
0.4,0.428571428571429,0.457142857142857,0.485714285714286,0.514285714285714,
0.542857142857143,0.571428571428572,0.6,0.628571428571429,0.657142857142857,
0.666463158655954),.UNSPECIFIED.)
CURVE()
GEOMETRIC_REPRESENTATION_ITEM()
RATIONAL_B_SPLINE_CURVE((1.,1.,1.,1.,1.,1.,1.,1.,1.,1.,1.,1.,1.,1.,1.,1.,
1.,1.,1.,1.,1.,1.,1.,1.,1.,1.,1.,1.,1.))
REPRESENTATION_ITEM('')
);
#692=(
BOUNDED_CURVE()
B_SPLINE_CURVE(5,(#49845,#49846,#49847,#49848,#49849,#49850,#49851,#49852,
#49853,#49854,#49855,#49856,#49857,#49858,#49859,#49860,#49861,#49862,#49863,
#49864,#49865,#49866,#49867,#49868,#49869),.UNSPECIFIED.,.F.,.F.)
B_SPLINE_CURVE_WITH_KNOTS((6,1,1,1,1,1,1,1,1,1,1,1,1,1,1,1,1,1,1,1,6),(0.437678095034471,
0.457142857142857,0.485714285714286,0.514285714285714,0.542857142857143,
0.571428571428572,0.6,0.628571428571429,0.657142857142857,0.685714285714286,
0.714285714285714,0.742857142857143,0.771428571428572,0.8,0.828571428571429,
0.857142857142857,0.885714285714286,0.914285714285714,0.942857142857143,
0.971428571428572,1.),.UNSPECIFIED.)
CURVE()
GEOMETRIC_REPRESENTATION_ITEM()
RATIONAL_B_SPLINE_CURVE((1.,1.,1.,1.,1.,1.,1.,1.,1.,1.,1.,1.,1.,1.,1.,1.,
1.,1.,1.,1.,1.,1.,1.,1.,1.))
REPRESENTATION_ITEM('')
);
#693=(
BOUNDED_CURVE()
B_SPLINE_CURVE(5,(#49873,#49874,#49875,#49876,#49877,#49878,#49879,#49880,
#49881,#49882,#49883,#49884,#49885,#49886,#49887,#49888,#49889,#49890,#49891,
#49892,#49893,#49894,#49895,#49896,#49897,#49898,#49899,#49900,#49901),
 .UNSPECIFIED.,.F.,.F.)
B_SPLINE_CURVE_WITH_KNOTS((6,1,1,1,1,1,1,1,1,1,1,1,1,1,1,1,1,1,1,1,1,1,
1,1,6),(0.,0.0285714285714286,0.0571428571428571,0.0857142857142857,0.114285714285714,
0.142857142857143,0.171428571428571,0.2,0.228571428571429,0.257142857142857,
0.285714285714286,0.314285714285714,0.342857142857143,0.371428571428571,
0.4,0.428571428571429,0.457142857142857,0.485714285714286,0.514285714285714,
0.542857142857143,0.571428571428572,0.6,0.628571428571429,0.657142857142857,
0.666463158655955),.UNSPECIFIED.)
CURVE()
GEOMETRIC_REPRESENTATION_ITEM()
RATIONAL_B_SPLINE_CURVE((1.,1.,1.,1.,1.,1.,1.,1.,1.,1.,1.,1.,1.,1.,1.,1.,
1.,1.,1.,1.,1.,1.,1.,1.,1.,1.,1.,1.,1.))
REPRESENTATION_ITEM('')
);
#694=(
BOUNDED_CURVE()
B_SPLINE_CURVE(5,(#49905,#49906,#49907,#49908,#49909,#49910,#49911,#49912,
#49913,#49914,#49915,#49916,#49917,#49918,#49919,#49920,#49921,#49922,#49923,
#49924,#49925,#49926,#49927,#49928,#49929),.UNSPECIFIED.,.F.,.F.)
B_SPLINE_CURVE_WITH_KNOTS((6,1,1,1,1,1,1,1,1,1,1,1,1,1,1,1,1,1,1,1,6),(0.437678095034471,
0.457142857142857,0.485714285714286,0.514285714285714,0.542857142857143,
0.571428571428572,0.6,0.628571428571429,0.657142857142857,0.685714285714286,
0.714285714285714,0.742857142857143,0.771428571428572,0.8,0.828571428571429,
0.857142857142857,0.885714285714286,0.914285714285714,0.942857142857143,
0.971428571428572,1.),.UNSPECIFIED.)
CURVE()
GEOMETRIC_REPRESENTATION_ITEM()
RATIONAL_B_SPLINE_CURVE((1.,1.,1.,1.,1.,1.,1.,1.,1.,1.,1.,1.,1.,1.,1.,1.,
1.,1.,1.,1.,1.,1.,1.,1.,1.))
REPRESENTATION_ITEM('')
);
#695=(
BOUNDED_CURVE()
B_SPLINE_CURVE(5,(#49933,#49934,#49935,#49936,#49937,#49938,#49939,#49940,
#49941,#49942,#49943,#49944,#49945,#49946,#49947,#49948,#49949,#49950,#49951,
#49952,#49953,#49954,#49955,#49956,#49957,#49958,#49959,#49960,#49961),
 .UNSPECIFIED.,.F.,.F.)
B_SPLINE_CURVE_WITH_KNOTS((6,1,1,1,1,1,1,1,1,1,1,1,1,1,1,1,1,1,1,1,1,1,
1,1,6),(0.,0.0285714285714286,0.0571428571428571,0.0857142857142857,0.114285714285714,
0.142857142857143,0.171428571428571,0.2,0.228571428571429,0.257142857142857,
0.285714285714286,0.314285714285714,0.342857142857143,0.371428571428571,
0.4,0.428571428571429,0.457142857142857,0.485714285714286,0.514285714285714,
0.542857142857143,0.571428571428572,0.6,0.628571428571429,0.657142857142857,
0.666463158655955),.UNSPECIFIED.)
CURVE()
GEOMETRIC_REPRESENTATION_ITEM()
RATIONAL_B_SPLINE_CURVE((1.,1.,1.,1.,1.,1.,1.,1.,1.,1.,1.,1.,1.,1.,1.,1.,
1.,1.,1.,1.,1.,1.,1.,1.,1.,1.,1.,1.,1.))
REPRESENTATION_ITEM('')
);
#696=(
BOUNDED_CURVE()
B_SPLINE_CURVE(5,(#49965,#49966,#49967,#49968,#49969,#49970,#49971,#49972,
#49973,#49974,#49975,#49976,#49977,#49978,#49979,#49980,#49981,#49982,#49983,
#49984,#49985,#49986,#49987,#49988,#49989),.UNSPECIFIED.,.F.,.F.)
B_SPLINE_CURVE_WITH_KNOTS((6,1,1,1,1,1,1,1,1,1,1,1,1,1,1,1,1,1,1,1,6),(0.437678095034471,
0.457142857142857,0.485714285714286,0.514285714285714,0.542857142857143,
0.571428571428572,0.6,0.628571428571429,0.657142857142857,0.685714285714286,
0.714285714285714,0.742857142857143,0.771428571428572,0.8,0.828571428571429,
0.857142857142857,0.885714285714286,0.914285714285714,0.942857142857143,
0.971428571428572,1.),.UNSPECIFIED.)
CURVE()
GEOMETRIC_REPRESENTATION_ITEM()
RATIONAL_B_SPLINE_CURVE((1.,1.,1.,1.,1.,1.,1.,1.,1.,1.,1.,1.,1.,1.,1.,1.,
1.,1.,1.,1.,1.,1.,1.,1.,1.))
REPRESENTATION_ITEM('')
);
#697=(
BOUNDED_CURVE()
B_SPLINE_CURVE(5,(#49993,#49994,#49995,#49996,#49997,#49998,#49999,#50000,
#50001,#50002,#50003,#50004,#50005,#50006,#50007,#50008,#50009,#50010,#50011,
#50012,#50013,#50014,#50015,#50016,#50017,#50018,#50019,#50020,#50021),
 .UNSPECIFIED.,.F.,.F.)
B_SPLINE_CURVE_WITH_KNOTS((6,1,1,1,1,1,1,1,1,1,1,1,1,1,1,1,1,1,1,1,1,1,
1,1,6),(0.,0.0285714285714286,0.0571428571428571,0.0857142857142857,0.114285714285714,
0.142857142857143,0.171428571428571,0.2,0.228571428571429,0.257142857142857,
0.285714285714286,0.314285714285714,0.342857142857143,0.371428571428571,
0.4,0.428571428571429,0.457142857142857,0.485714285714286,0.514285714285714,
0.542857142857143,0.571428571428572,0.6,0.628571428571429,0.657142857142857,
0.666463158655954),.UNSPECIFIED.)
CURVE()
GEOMETRIC_REPRESENTATION_ITEM()
RATIONAL_B_SPLINE_CURVE((1.,1.,1.,1.,1.,1.,1.,1.,1.,1.,1.,1.,1.,1.,1.,1.,
1.,1.,1.,1.,1.,1.,1.,1.,1.,1.,1.,1.,1.))
REPRESENTATION_ITEM('')
);
#698=(
BOUNDED_CURVE()
B_SPLINE_CURVE(5,(#50025,#50026,#50027,#50028,#50029,#50030,#50031,#50032,
#50033,#50034,#50035,#50036,#50037,#50038,#50039,#50040,#50041,#50042,#50043,
#50044,#50045,#50046,#50047,#50048,#50049),.UNSPECIFIED.,.F.,.F.)
B_SPLINE_CURVE_WITH_KNOTS((6,1,1,1,1,1,1,1,1,1,1,1,1,1,1,1,1,1,1,1,6),(0.437678095034471,
0.457142857142857,0.485714285714286,0.514285714285714,0.542857142857143,
0.571428571428572,0.6,0.628571428571429,0.657142857142857,0.685714285714286,
0.714285714285714,0.742857142857143,0.771428571428572,0.8,0.828571428571429,
0.857142857142857,0.885714285714286,0.914285714285714,0.942857142857143,
0.971428571428572,1.),.UNSPECIFIED.)
CURVE()
GEOMETRIC_REPRESENTATION_ITEM()
RATIONAL_B_SPLINE_CURVE((1.,1.,1.,1.,1.,1.,1.,1.,1.,1.,1.,1.,1.,1.,1.,1.,
1.,1.,1.,1.,1.,1.,1.,1.,1.))
REPRESENTATION_ITEM('')
);
#699=(
BOUNDED_CURVE()
B_SPLINE_CURVE(5,(#50053,#50054,#50055,#50056,#50057,#50058,#50059,#50060,
#50061,#50062,#50063,#50064,#50065,#50066,#50067,#50068,#50069,#50070,#50071,
#50072,#50073,#50074,#50075,#50076,#50077,#50078,#50079,#50080,#50081),
 .UNSPECIFIED.,.F.,.F.)
B_SPLINE_CURVE_WITH_KNOTS((6,1,1,1,1,1,1,1,1,1,1,1,1,1,1,1,1,1,1,1,1,1,
1,1,6),(0.,0.0285714285714286,0.0571428571428571,0.0857142857142857,0.114285714285714,
0.142857142857143,0.171428571428571,0.2,0.228571428571429,0.257142857142857,
0.285714285714286,0.314285714285714,0.342857142857143,0.371428571428571,
0.4,0.428571428571429,0.457142857142857,0.485714285714286,0.514285714285714,
0.542857142857143,0.571428571428572,0.6,0.628571428571429,0.657142857142857,
0.666463158655955),.UNSPECIFIED.)
CURVE()
GEOMETRIC_REPRESENTATION_ITEM()
RATIONAL_B_SPLINE_CURVE((1.,1.,1.,1.,1.,1.,1.,1.,1.,1.,1.,1.,1.,1.,1.,1.,
1.,1.,1.,1.,1.,1.,1.,1.,1.,1.,1.,1.,1.))
REPRESENTATION_ITEM('')
);
#700=(
BOUNDED_CURVE()
B_SPLINE_CURVE(5,(#50090,#50091,#50092,#50093,#50094,#50095,#50096,#50097,
#50098,#50099,#50100,#50101,#50102,#50103,#50104,#50105,#50106,#50107,#50108,
#50109,#50110,#50111,#50112,#50113,#50114,#50115,#50116,#50117,#50118),
 .UNSPECIFIED.,.F.,.F.)
B_SPLINE_CURVE_WITH_KNOTS((6,1,1,1,1,1,1,1,1,1,1,1,1,1,1,1,1,1,1,1,1,1,
1,1,6),(-0.670627588953113,-0.657142857142857,-0.628571428571429,-0.6,-0.571428571428572,
-0.542857142857143,-0.514285714285714,-0.485714285714286,-0.457142857142857,
-0.428571428571429,-0.4,-0.371428571428571,-0.342857142857143,-0.314285714285714,
-0.285714285714286,-0.257142857142857,-0.228571428571429,-0.2,-0.171428571428571,
-0.142857142857143,-0.114285714285714,-0.0857142857142857,-0.0571428571428571,
-0.0285714285714286,0.),.UNSPECIFIED.)
CURVE()
GEOMETRIC_REPRESENTATION_ITEM()
RATIONAL_B_SPLINE_CURVE((1.,1.,1.,1.,1.,1.,1.,1.,1.,1.,1.,1.,1.,1.,1.,1.,
1.,1.,1.,1.,1.,1.,1.,1.,1.,1.,1.,1.,1.))
REPRESENTATION_ITEM('')
);
#701=(
BOUNDED_CURVE()
B_SPLINE_CURVE(5,(#50122,#50123,#50124,#50125,#50126,#50127,#50128,#50129,
#50130,#50131,#50132,#50133,#50134,#50135,#50136,#50137,#50138,#50139,#50140,
#50141,#50142,#50143,#50144,#50145,#50146,#50147),.UNSPECIFIED.,.F.,.F.)
B_SPLINE_CURVE_WITH_KNOTS((6,1,1,1,1,1,1,1,1,1,1,1,1,1,1,1,1,1,1,1,1,6),
(-1.,-0.971428571428572,-0.942857142857143,-0.914285714285714,-0.885714285714286,
-0.857142857142857,-0.828571428571429,-0.8,-0.771428571428572,-0.742857142857143,
-0.714285714285714,-0.685714285714286,-0.657142857142857,-0.628571428571429,
-0.6,-0.571428571428572,-0.542857142857143,-0.514285714285714,-0.485714285714286,
-0.457142857142857,-0.428571428571429,-0.428061295609926),.UNSPECIFIED.)
CURVE()
GEOMETRIC_REPRESENTATION_ITEM()
RATIONAL_B_SPLINE_CURVE((1.,1.,1.,1.,1.,1.,1.,1.,1.,1.,1.,1.,1.,1.,1.,1.,
1.,1.,1.,1.,1.,1.,1.,1.,1.,1.))
REPRESENTATION_ITEM('')
);
#702=(
BOUNDED_CURVE()
B_SPLINE_CURVE(5,(#50151,#50152,#50153,#50154,#50155,#50156,#50157,#50158,
#50159,#50160,#50161,#50162,#50163,#50164,#50165,#50166,#50167,#50168,#50169,
#50170,#50171,#50172,#50173,#50174,#50175,#50176,#50177,#50178,#50179),
 .UNSPECIFIED.,.F.,.F.)
B_SPLINE_CURVE_WITH_KNOTS((6,1,1,1,1,1,1,1,1,1,1,1,1,1,1,1,1,1,1,1,1,1,
1,1,6),(-0.670627588953112,-0.657142857142857,-0.628571428571429,-0.6,-0.571428571428572,
-0.542857142857143,-0.514285714285714,-0.485714285714286,-0.457142857142857,
-0.428571428571429,-0.4,-0.371428571428571,-0.342857142857143,-0.314285714285714,
-0.285714285714286,-0.257142857142857,-0.228571428571429,-0.2,-0.171428571428571,
-0.142857142857143,-0.114285714285714,-0.0857142857142857,-0.0571428571428571,
-0.0285714285714286,0.),.UNSPECIFIED.)
CURVE()
GEOMETRIC_REPRESENTATION_ITEM()
RATIONAL_B_SPLINE_CURVE((1.,1.,1.,1.,1.,1.,1.,1.,1.,1.,1.,1.,1.,1.,1.,1.,
1.,1.,1.,1.,1.,1.,1.,1.,1.,1.,1.,1.,1.))
REPRESENTATION_ITEM('')
);
#703=(
BOUNDED_CURVE()
B_SPLINE_CURVE(5,(#50183,#50184,#50185,#50186,#50187,#50188,#50189,#50190,
#50191,#50192,#50193,#50194,#50195,#50196,#50197,#50198,#50199,#50200,#50201,
#50202,#50203,#50204,#50205,#50206,#50207,#50208),.UNSPECIFIED.,.F.,.F.)
B_SPLINE_CURVE_WITH_KNOTS((6,1,1,1,1,1,1,1,1,1,1,1,1,1,1,1,1,1,1,1,1,6),
(-1.,-0.971428571428572,-0.942857142857143,-0.914285714285714,-0.885714285714286,
-0.857142857142857,-0.828571428571429,-0.8,-0.771428571428572,-0.742857142857143,
-0.714285714285714,-0.685714285714286,-0.657142857142857,-0.628571428571429,
-0.6,-0.571428571428572,-0.542857142857143,-0.514285714285714,-0.485714285714286,
-0.457142857142857,-0.428571428571429,-0.428061295609925),.UNSPECIFIED.)
CURVE()
GEOMETRIC_REPRESENTATION_ITEM()
RATIONAL_B_SPLINE_CURVE((1.,1.,1.,1.,1.,1.,1.,1.,1.,1.,1.,1.,1.,1.,1.,1.,
1.,1.,1.,1.,1.,1.,1.,1.,1.,1.))
REPRESENTATION_ITEM('')
);
#704=(
BOUNDED_CURVE()
B_SPLINE_CURVE(5,(#50212,#50213,#50214,#50215,#50216,#50217,#50218,#50219,
#50220,#50221,#50222,#50223,#50224,#50225,#50226,#50227,#50228,#50229,#50230,
#50231,#50232,#50233,#50234,#50235,#50236,#50237,#50238,#50239,#50240),
 .UNSPECIFIED.,.F.,.F.)
B_SPLINE_CURVE_WITH_KNOTS((6,1,1,1,1,1,1,1,1,1,1,1,1,1,1,1,1,1,1,1,1,1,
1,1,6),(-0.670627588953112,-0.657142857142857,-0.628571428571429,-0.6,-0.571428571428572,
-0.542857142857143,-0.514285714285714,-0.485714285714286,-0.457142857142857,
-0.428571428571429,-0.4,-0.371428571428571,-0.342857142857143,-0.314285714285714,
-0.285714285714286,-0.257142857142857,-0.228571428571429,-0.2,-0.171428571428571,
-0.142857142857143,-0.114285714285714,-0.0857142857142857,-0.0571428571428571,
-0.0285714285714286,0.),.UNSPECIFIED.)
CURVE()
GEOMETRIC_REPRESENTATION_ITEM()
RATIONAL_B_SPLINE_CURVE((1.,1.,1.,1.,1.,1.,1.,1.,1.,1.,1.,1.,1.,1.,1.,1.,
1.,1.,1.,1.,1.,1.,1.,1.,1.,1.,1.,1.,1.))
REPRESENTATION_ITEM('')
);
#705=(
BOUNDED_CURVE()
B_SPLINE_CURVE(5,(#50244,#50245,#50246,#50247,#50248,#50249,#50250,#50251,
#50252,#50253,#50254,#50255,#50256,#50257,#50258,#50259,#50260,#50261,#50262,
#50263,#50264,#50265,#50266,#50267,#50268,#50269),.UNSPECIFIED.,.F.,.F.)
B_SPLINE_CURVE_WITH_KNOTS((6,1,1,1,1,1,1,1,1,1,1,1,1,1,1,1,1,1,1,1,1,6),
(-1.,-0.971428571428572,-0.942857142857143,-0.914285714285714,-0.885714285714286,
-0.857142857142857,-0.828571428571429,-0.8,-0.771428571428572,-0.742857142857143,
-0.714285714285714,-0.685714285714286,-0.657142857142857,-0.628571428571429,
-0.6,-0.571428571428572,-0.542857142857143,-0.514285714285714,-0.485714285714286,
-0.457142857142857,-0.428571428571429,-0.428061295609925),.UNSPECIFIED.)
CURVE()
GEOMETRIC_REPRESENTATION_ITEM()
RATIONAL_B_SPLINE_CURVE((1.,1.,1.,1.,1.,1.,1.,1.,1.,1.,1.,1.,1.,1.,1.,1.,
1.,1.,1.,1.,1.,1.,1.,1.,1.,1.))
REPRESENTATION_ITEM('')
);
#706=(
BOUNDED_CURVE()
B_SPLINE_CURVE(5,(#50273,#50274,#50275,#50276,#50277,#50278,#50279,#50280,
#50281,#50282,#50283,#50284,#50285,#50286,#50287,#50288,#50289,#50290,#50291,
#50292,#50293,#50294,#50295,#50296,#50297,#50298,#50299,#50300,#50301),
 .UNSPECIFIED.,.F.,.F.)
B_SPLINE_CURVE_WITH_KNOTS((6,1,1,1,1,1,1,1,1,1,1,1,1,1,1,1,1,1,1,1,1,1,
1,1,6),(-0.670627588953113,-0.657142857142857,-0.628571428571429,-0.6,-0.571428571428572,
-0.542857142857143,-0.514285714285714,-0.485714285714286,-0.457142857142857,
-0.428571428571429,-0.4,-0.371428571428571,-0.342857142857143,-0.314285714285714,
-0.285714285714286,-0.257142857142857,-0.228571428571429,-0.2,-0.171428571428571,
-0.142857142857143,-0.114285714285714,-0.0857142857142857,-0.0571428571428571,
-0.0285714285714286,0.),.UNSPECIFIED.)
CURVE()
GEOMETRIC_REPRESENTATION_ITEM()
RATIONAL_B_SPLINE_CURVE((1.,1.,1.,1.,1.,1.,1.,1.,1.,1.,1.,1.,1.,1.,1.,1.,
1.,1.,1.,1.,1.,1.,1.,1.,1.,1.,1.,1.,1.))
REPRESENTATION_ITEM('')
);
#707=(
BOUNDED_CURVE()
B_SPLINE_CURVE(5,(#50305,#50306,#50307,#50308,#50309,#50310,#50311,#50312,
#50313,#50314,#50315,#50316,#50317,#50318,#50319,#50320,#50321,#50322,#50323,
#50324,#50325,#50326,#50327,#50328,#50329,#50330),.UNSPECIFIED.,.F.,.F.)
B_SPLINE_CURVE_WITH_KNOTS((6,1,1,1,1,1,1,1,1,1,1,1,1,1,1,1,1,1,1,1,1,6),
(-1.,-0.971428571428572,-0.942857142857143,-0.914285714285714,-0.885714285714286,
-0.857142857142857,-0.828571428571429,-0.8,-0.771428571428572,-0.742857142857143,
-0.714285714285714,-0.685714285714286,-0.657142857142857,-0.628571428571429,
-0.6,-0.571428571428572,-0.542857142857143,-0.514285714285714,-0.485714285714286,
-0.457142857142857,-0.428571428571429,-0.428061295609926),.UNSPECIFIED.)
CURVE()
GEOMETRIC_REPRESENTATION_ITEM()
RATIONAL_B_SPLINE_CURVE((1.,1.,1.,1.,1.,1.,1.,1.,1.,1.,1.,1.,1.,1.,1.,1.,
1.,1.,1.,1.,1.,1.,1.,1.,1.,1.))
REPRESENTATION_ITEM('')
);
#708=(
BOUNDED_CURVE()
B_SPLINE_CURVE(5,(#50334,#50335,#50336,#50337,#50338,#50339,#50340,#50341,
#50342,#50343,#50344,#50345,#50346,#50347,#50348,#50349,#50350,#50351,#50352,
#50353,#50354,#50355,#50356,#50357,#50358,#50359,#50360,#50361,#50362),
 .UNSPECIFIED.,.F.,.F.)
B_SPLINE_CURVE_WITH_KNOTS((6,1,1,1,1,1,1,1,1,1,1,1,1,1,1,1,1,1,1,1,1,1,
1,1,6),(-0.670627588953112,-0.657142857142857,-0.628571428571429,-0.6,-0.571428571428572,
-0.542857142857143,-0.514285714285714,-0.485714285714286,-0.457142857142857,
-0.428571428571429,-0.4,-0.371428571428571,-0.342857142857143,-0.314285714285714,
-0.285714285714286,-0.257142857142857,-0.228571428571429,-0.2,-0.171428571428571,
-0.142857142857143,-0.114285714285714,-0.0857142857142857,-0.0571428571428571,
-0.0285714285714286,0.),.UNSPECIFIED.)
CURVE()
GEOMETRIC_REPRESENTATION_ITEM()
RATIONAL_B_SPLINE_CURVE((1.,1.,1.,1.,1.,1.,1.,1.,1.,1.,1.,1.,1.,1.,1.,1.,
1.,1.,1.,1.,1.,1.,1.,1.,1.,1.,1.,1.,1.))
REPRESENTATION_ITEM('')
);
#709=(
BOUNDED_CURVE()
B_SPLINE_CURVE(5,(#50366,#50367,#50368,#50369,#50370,#50371,#50372,#50373,
#50374,#50375,#50376,#50377,#50378,#50379,#50380,#50381,#50382,#50383,#50384,
#50385,#50386,#50387,#50388,#50389,#50390,#50391),.UNSPECIFIED.,.F.,.F.)
B_SPLINE_CURVE_WITH_KNOTS((6,1,1,1,1,1,1,1,1,1,1,1,1,1,1,1,1,1,1,1,1,6),
(-1.,-0.971428571428572,-0.942857142857143,-0.914285714285714,-0.885714285714286,
-0.857142857142857,-0.828571428571429,-0.8,-0.771428571428572,-0.742857142857143,
-0.714285714285714,-0.685714285714286,-0.657142857142857,-0.628571428571429,
-0.6,-0.571428571428572,-0.542857142857143,-0.514285714285714,-0.485714285714286,
-0.457142857142857,-0.428571428571429,-0.428061295609926),.UNSPECIFIED.)
CURVE()
GEOMETRIC_REPRESENTATION_ITEM()
RATIONAL_B_SPLINE_CURVE((1.,1.,1.,1.,1.,1.,1.,1.,1.,1.,1.,1.,1.,1.,1.,1.,
1.,1.,1.,1.,1.,1.,1.,1.,1.,1.))
REPRESENTATION_ITEM('')
);
#710=(
BOUNDED_CURVE()
B_SPLINE_CURVE(5,(#50395,#50396,#50397,#50398,#50399,#50400,#50401,#50402,
#50403,#50404,#50405,#50406,#50407,#50408,#50409,#50410,#50411,#50412,#50413,
#50414,#50415,#50416,#50417,#50418,#50419,#50420,#50421,#50422,#50423),
 .UNSPECIFIED.,.F.,.F.)
B_SPLINE_CURVE_WITH_KNOTS((6,1,1,1,1,1,1,1,1,1,1,1,1,1,1,1,1,1,1,1,1,1,
1,1,6),(-0.670627588953113,-0.657142857142857,-0.628571428571429,-0.6,-0.571428571428572,
-0.542857142857143,-0.514285714285714,-0.485714285714286,-0.457142857142857,
-0.428571428571429,-0.4,-0.371428571428571,-0.342857142857143,-0.314285714285714,
-0.285714285714286,-0.257142857142857,-0.228571428571429,-0.2,-0.171428571428571,
-0.142857142857143,-0.114285714285714,-0.0857142857142857,-0.0571428571428571,
-0.0285714285714286,0.),.UNSPECIFIED.)
CURVE()
GEOMETRIC_REPRESENTATION_ITEM()
RATIONAL_B_SPLINE_CURVE((1.,1.,1.,1.,1.,1.,1.,1.,1.,1.,1.,1.,1.,1.,1.,1.,
1.,1.,1.,1.,1.,1.,1.,1.,1.,1.,1.,1.,1.))
REPRESENTATION_ITEM('')
);
#711=(
BOUNDED_CURVE()
B_SPLINE_CURVE(5,(#50427,#50428,#50429,#50430,#50431,#50432,#50433,#50434,
#50435,#50436,#50437,#50438,#50439,#50440,#50441,#50442,#50443,#50444,#50445,
#50446,#50447,#50448,#50449,#50450,#50451,#50452),.UNSPECIFIED.,.F.,.F.)
B_SPLINE_CURVE_WITH_KNOTS((6,1,1,1,1,1,1,1,1,1,1,1,1,1,1,1,1,1,1,1,1,6),
(-1.,-0.971428571428572,-0.942857142857143,-0.914285714285714,-0.885714285714286,
-0.857142857142857,-0.828571428571429,-0.8,-0.771428571428572,-0.742857142857143,
-0.714285714285714,-0.685714285714286,-0.657142857142857,-0.628571428571429,
-0.6,-0.571428571428572,-0.542857142857143,-0.514285714285714,-0.485714285714286,
-0.457142857142857,-0.428571428571429,-0.428061295609926),.UNSPECIFIED.)
CURVE()
GEOMETRIC_REPRESENTATION_ITEM()
RATIONAL_B_SPLINE_CURVE((1.,1.,1.,1.,1.,1.,1.,1.,1.,1.,1.,1.,1.,1.,1.,1.,
1.,1.,1.,1.,1.,1.,1.,1.,1.,1.))
REPRESENTATION_ITEM('')
);
#712=(
BOUNDED_CURVE()
B_SPLINE_CURVE(5,(#50456,#50457,#50458,#50459,#50460,#50461,#50462,#50463,
#50464,#50465,#50466,#50467,#50468,#50469,#50470,#50471,#50472,#50473,#50474,
#50475,#50476,#50477,#50478,#50479,#50480,#50481,#50482,#50483,#50484),
 .UNSPECIFIED.,.F.,.F.)
B_SPLINE_CURVE_WITH_KNOTS((6,1,1,1,1,1,1,1,1,1,1,1,1,1,1,1,1,1,1,1,1,1,
1,1,6),(-0.670627588953112,-0.657142857142857,-0.628571428571429,-0.6,-0.571428571428572,
-0.542857142857143,-0.514285714285714,-0.485714285714286,-0.457142857142857,
-0.428571428571429,-0.4,-0.371428571428571,-0.342857142857143,-0.314285714285714,
-0.285714285714286,-0.257142857142857,-0.228571428571429,-0.2,-0.171428571428571,
-0.142857142857143,-0.114285714285714,-0.0857142857142857,-0.0571428571428571,
-0.0285714285714286,0.),.UNSPECIFIED.)
CURVE()
GEOMETRIC_REPRESENTATION_ITEM()
RATIONAL_B_SPLINE_CURVE((1.,1.,1.,1.,1.,1.,1.,1.,1.,1.,1.,1.,1.,1.,1.,1.,
1.,1.,1.,1.,1.,1.,1.,1.,1.,1.,1.,1.,1.))
REPRESENTATION_ITEM('')
);
#713=(
BOUNDED_CURVE()
B_SPLINE_CURVE(5,(#50488,#50489,#50490,#50491,#50492,#50493,#50494,#50495,
#50496,#50497,#50498,#50499,#50500,#50501,#50502,#50503,#50504,#50505,#50506,
#50507,#50508,#50509,#50510,#50511,#50512,#50513),.UNSPECIFIED.,.F.,.F.)
B_SPLINE_CURVE_WITH_KNOTS((6,1,1,1,1,1,1,1,1,1,1,1,1,1,1,1,1,1,1,1,1,6),
(-1.,-0.971428571428572,-0.942857142857143,-0.914285714285714,-0.885714285714286,
-0.857142857142857,-0.828571428571429,-0.8,-0.771428571428572,-0.742857142857143,
-0.714285714285714,-0.685714285714286,-0.657142857142857,-0.628571428571429,
-0.6,-0.571428571428572,-0.542857142857143,-0.514285714285714,-0.485714285714286,
-0.457142857142857,-0.428571428571429,-0.428061295609925),.UNSPECIFIED.)
CURVE()
GEOMETRIC_REPRESENTATION_ITEM()
RATIONAL_B_SPLINE_CURVE((1.,1.,1.,1.,1.,1.,1.,1.,1.,1.,1.,1.,1.,1.,1.,1.,
1.,1.,1.,1.,1.,1.,1.,1.,1.,1.))
REPRESENTATION_ITEM('')
);
#714=(
BOUNDED_CURVE()
B_SPLINE_CURVE(5,(#50517,#50518,#50519,#50520,#50521,#50522,#50523,#50524,
#50525,#50526,#50527,#50528,#50529,#50530,#50531,#50532,#50533,#50534,#50535,
#50536,#50537,#50538,#50539,#50540,#50541,#50542,#50543,#50544,#50545),
 .UNSPECIFIED.,.F.,.F.)
B_SPLINE_CURVE_WITH_KNOTS((6,1,1,1,1,1,1,1,1,1,1,1,1,1,1,1,1,1,1,1,1,1,
1,1,6),(-0.670627588953113,-0.657142857142857,-0.628571428571429,-0.6,-0.571428571428572,
-0.542857142857143,-0.514285714285714,-0.485714285714286,-0.457142857142857,
-0.428571428571429,-0.4,-0.371428571428571,-0.342857142857143,-0.314285714285714,
-0.285714285714286,-0.257142857142857,-0.228571428571429,-0.2,-0.171428571428571,
-0.142857142857143,-0.114285714285714,-0.0857142857142857,-0.0571428571428571,
-0.0285714285714286,0.),.UNSPECIFIED.)
CURVE()
GEOMETRIC_REPRESENTATION_ITEM()
RATIONAL_B_SPLINE_CURVE((1.,1.,1.,1.,1.,1.,1.,1.,1.,1.,1.,1.,1.,1.,1.,1.,
1.,1.,1.,1.,1.,1.,1.,1.,1.,1.,1.,1.,1.))
REPRESENTATION_ITEM('')
);
#715=(
BOUNDED_CURVE()
B_SPLINE_CURVE(5,(#50549,#50550,#50551,#50552,#50553,#50554,#50555,#50556,
#50557,#50558,#50559,#50560,#50561,#50562,#50563,#50564,#50565,#50566,#50567,
#50568,#50569,#50570,#50571,#50572,#50573,#50574),.UNSPECIFIED.,.F.,.F.)
B_SPLINE_CURVE_WITH_KNOTS((6,1,1,1,1,1,1,1,1,1,1,1,1,1,1,1,1,1,1,1,1,6),
(-1.,-0.971428571428572,-0.942857142857143,-0.914285714285714,-0.885714285714286,
-0.857142857142857,-0.828571428571429,-0.8,-0.771428571428572,-0.742857142857143,
-0.714285714285714,-0.685714285714286,-0.657142857142857,-0.628571428571429,
-0.6,-0.571428571428572,-0.542857142857143,-0.514285714285714,-0.485714285714286,
-0.457142857142857,-0.428571428571429,-0.428061295609925),.UNSPECIFIED.)
CURVE()
GEOMETRIC_REPRESENTATION_ITEM()
RATIONAL_B_SPLINE_CURVE((1.,1.,1.,1.,1.,1.,1.,1.,1.,1.,1.,1.,1.,1.,1.,1.,
1.,1.,1.,1.,1.,1.,1.,1.,1.,1.))
REPRESENTATION_ITEM('')
);
#716=(
BOUNDED_CURVE()
B_SPLINE_CURVE(5,(#50578,#50579,#50580,#50581,#50582,#50583,#50584,#50585,
#50586,#50587,#50588,#50589,#50590,#50591,#50592,#50593,#50594,#50595,#50596,
#50597,#50598,#50599,#50600,#50601,#50602,#50603,#50604,#50605,#50606),
 .UNSPECIFIED.,.F.,.F.)
B_SPLINE_CURVE_WITH_KNOTS((6,1,1,1,1,1,1,1,1,1,1,1,1,1,1,1,1,1,1,1,1,1,
1,1,6),(-0.670627588953113,-0.657142857142857,-0.628571428571429,-0.6,-0.571428571428572,
-0.542857142857143,-0.514285714285714,-0.485714285714286,-0.457142857142857,
-0.428571428571429,-0.4,-0.371428571428571,-0.342857142857143,-0.314285714285714,
-0.285714285714286,-0.257142857142857,-0.228571428571429,-0.2,-0.171428571428571,
-0.142857142857143,-0.114285714285714,-0.0857142857142857,-0.0571428571428571,
-0.0285714285714286,0.),.UNSPECIFIED.)
CURVE()
GEOMETRIC_REPRESENTATION_ITEM()
RATIONAL_B_SPLINE_CURVE((1.,1.,1.,1.,1.,1.,1.,1.,1.,1.,1.,1.,1.,1.,1.,1.,
1.,1.,1.,1.,1.,1.,1.,1.,1.,1.,1.,1.,1.))
REPRESENTATION_ITEM('')
);
#717=(
BOUNDED_CURVE()
B_SPLINE_CURVE(5,(#50610,#50611,#50612,#50613,#50614,#50615,#50616,#50617,
#50618,#50619,#50620,#50621,#50622,#50623,#50624,#50625,#50626,#50627,#50628,
#50629,#50630,#50631,#50632,#50633,#50634,#50635),.UNSPECIFIED.,.F.,.F.)
B_SPLINE_CURVE_WITH_KNOTS((6,1,1,1,1,1,1,1,1,1,1,1,1,1,1,1,1,1,1,1,1,6),
(-1.,-0.971428571428572,-0.942857142857143,-0.914285714285714,-0.885714285714286,
-0.857142857142857,-0.828571428571429,-0.8,-0.771428571428572,-0.742857142857143,
-0.714285714285714,-0.685714285714286,-0.657142857142857,-0.628571428571429,
-0.6,-0.571428571428572,-0.542857142857143,-0.514285714285714,-0.485714285714286,
-0.457142857142857,-0.428571428571429,-0.428061295609926),.UNSPECIFIED.)
CURVE()
GEOMETRIC_REPRESENTATION_ITEM()
RATIONAL_B_SPLINE_CURVE((1.,1.,1.,1.,1.,1.,1.,1.,1.,1.,1.,1.,1.,1.,1.,1.,
1.,1.,1.,1.,1.,1.,1.,1.,1.,1.))
REPRESENTATION_ITEM('')
);
#718=(
BOUNDED_CURVE()
B_SPLINE_CURVE(5,(#50639,#50640,#50641,#50642,#50643,#50644,#50645,#50646,
#50647,#50648,#50649,#50650,#50651,#50652,#50653,#50654,#50655,#50656,#50657,
#50658,#50659,#50660,#50661,#50662,#50663,#50664,#50665,#50666,#50667),
 .UNSPECIFIED.,.F.,.F.)
B_SPLINE_CURVE_WITH_KNOTS((6,1,1,1,1,1,1,1,1,1,1,1,1,1,1,1,1,1,1,1,1,1,
1,1,6),(-0.670627588953112,-0.657142857142857,-0.628571428571429,-0.6,-0.571428571428572,
-0.542857142857143,-0.514285714285714,-0.485714285714286,-0.457142857142857,
-0.428571428571429,-0.4,-0.371428571428571,-0.342857142857143,-0.314285714285714,
-0.285714285714286,-0.257142857142857,-0.228571428571429,-0.2,-0.171428571428571,
-0.142857142857143,-0.114285714285714,-0.0857142857142857,-0.0571428571428571,
-0.0285714285714286,0.),.UNSPECIFIED.)
CURVE()
GEOMETRIC_REPRESENTATION_ITEM()
RATIONAL_B_SPLINE_CURVE((1.,1.,1.,1.,1.,1.,1.,1.,1.,1.,1.,1.,1.,1.,1.,1.,
1.,1.,1.,1.,1.,1.,1.,1.,1.,1.,1.,1.,1.))
REPRESENTATION_ITEM('')
);
#719=(
BOUNDED_CURVE()
B_SPLINE_CURVE(5,(#50671,#50672,#50673,#50674,#50675,#50676,#50677,#50678,
#50679,#50680,#50681,#50682,#50683,#50684,#50685,#50686,#50687,#50688,#50689,
#50690,#50691,#50692,#50693,#50694,#50695,#50696),.UNSPECIFIED.,.F.,.F.)
B_SPLINE_CURVE_WITH_KNOTS((6,1,1,1,1,1,1,1,1,1,1,1,1,1,1,1,1,1,1,1,1,6),
(-1.,-0.971428571428572,-0.942857142857143,-0.914285714285714,-0.885714285714286,
-0.857142857142857,-0.828571428571429,-0.8,-0.771428571428572,-0.742857142857143,
-0.714285714285714,-0.685714285714286,-0.657142857142857,-0.628571428571429,
-0.6,-0.571428571428572,-0.542857142857143,-0.514285714285714,-0.485714285714286,
-0.457142857142857,-0.428571428571429,-0.428061295609926),.UNSPECIFIED.)
CURVE()
GEOMETRIC_REPRESENTATION_ITEM()
RATIONAL_B_SPLINE_CURVE((1.,1.,1.,1.,1.,1.,1.,1.,1.,1.,1.,1.,1.,1.,1.,1.,
1.,1.,1.,1.,1.,1.,1.,1.,1.,1.))
REPRESENTATION_ITEM('')
);
#720=(
BOUNDED_CURVE()
B_SPLINE_CURVE(5,(#50700,#50701,#50702,#50703,#50704,#50705,#50706,#50707,
#50708,#50709,#50710,#50711,#50712,#50713,#50714,#50715,#50716,#50717,#50718,
#50719,#50720,#50721,#50722,#50723,#50724,#50725,#50726,#50727,#50728),
 .UNSPECIFIED.,.F.,.F.)
B_SPLINE_CURVE_WITH_KNOTS((6,1,1,1,1,1,1,1,1,1,1,1,1,1,1,1,1,1,1,1,1,1,
1,1,6),(-0.670627588953112,-0.657142857142857,-0.628571428571429,-0.6,-0.571428571428572,
-0.542857142857143,-0.514285714285714,-0.485714285714286,-0.457142857142857,
-0.428571428571429,-0.4,-0.371428571428571,-0.342857142857143,-0.314285714285714,
-0.285714285714286,-0.257142857142857,-0.228571428571429,-0.2,-0.171428571428571,
-0.142857142857143,-0.114285714285714,-0.0857142857142857,-0.0571428571428571,
-0.0285714285714286,0.),.UNSPECIFIED.)
CURVE()
GEOMETRIC_REPRESENTATION_ITEM()
RATIONAL_B_SPLINE_CURVE((1.,1.,1.,1.,1.,1.,1.,1.,1.,1.,1.,1.,1.,1.,1.,1.,
1.,1.,1.,1.,1.,1.,1.,1.,1.,1.,1.,1.,1.))
REPRESENTATION_ITEM('')
);
#721=(
BOUNDED_CURVE()
B_SPLINE_CURVE(5,(#50732,#50733,#50734,#50735,#50736,#50737,#50738,#50739,
#50740,#50741,#50742,#50743,#50744,#50745,#50746,#50747,#50748,#50749,#50750,
#50751,#50752,#50753,#50754,#50755,#50756,#50757),.UNSPECIFIED.,.F.,.F.)
B_SPLINE_CURVE_WITH_KNOTS((6,1,1,1,1,1,1,1,1,1,1,1,1,1,1,1,1,1,1,1,1,6),
(-1.,-0.971428571428572,-0.942857142857143,-0.914285714285714,-0.885714285714286,
-0.857142857142857,-0.828571428571429,-0.8,-0.771428571428572,-0.742857142857143,
-0.714285714285714,-0.685714285714286,-0.657142857142857,-0.628571428571429,
-0.6,-0.571428571428572,-0.542857142857143,-0.514285714285714,-0.485714285714286,
-0.457142857142857,-0.428571428571429,-0.428061295609926),.UNSPECIFIED.)
CURVE()
GEOMETRIC_REPRESENTATION_ITEM()
RATIONAL_B_SPLINE_CURVE((1.,1.,1.,1.,1.,1.,1.,1.,1.,1.,1.,1.,1.,1.,1.,1.,
1.,1.,1.,1.,1.,1.,1.,1.,1.,1.))
REPRESENTATION_ITEM('')
);
#722=(
BOUNDED_CURVE()
B_SPLINE_CURVE(5,(#50761,#50762,#50763,#50764,#50765,#50766,#50767,#50768,
#50769,#50770,#50771,#50772,#50773,#50774,#50775,#50776,#50777,#50778,#50779,
#50780,#50781,#50782,#50783,#50784,#50785,#50786,#50787,#50788,#50789),
 .UNSPECIFIED.,.F.,.F.)
B_SPLINE_CURVE_WITH_KNOTS((6,1,1,1,1,1,1,1,1,1,1,1,1,1,1,1,1,1,1,1,1,1,
1,1,6),(-0.670627588953112,-0.657142857142857,-0.628571428571429,-0.6,-0.571428571428572,
-0.542857142857143,-0.514285714285714,-0.485714285714286,-0.457142857142857,
-0.428571428571429,-0.4,-0.371428571428571,-0.342857142857143,-0.314285714285714,
-0.285714285714286,-0.257142857142857,-0.228571428571429,-0.2,-0.171428571428571,
-0.142857142857143,-0.114285714285714,-0.0857142857142857,-0.0571428571428571,
-0.0285714285714286,0.),.UNSPECIFIED.)
CURVE()
GEOMETRIC_REPRESENTATION_ITEM()
RATIONAL_B_SPLINE_CURVE((1.,1.,1.,1.,1.,1.,1.,1.,1.,1.,1.,1.,1.,1.,1.,1.,
1.,1.,1.,1.,1.,1.,1.,1.,1.,1.,1.,1.,1.))
REPRESENTATION_ITEM('')
);
#723=(
BOUNDED_CURVE()
B_SPLINE_CURVE(5,(#50793,#50794,#50795,#50796,#50797,#50798,#50799,#50800,
#50801,#50802,#50803,#50804,#50805,#50806,#50807,#50808,#50809,#50810,#50811,
#50812,#50813,#50814,#50815,#50816,#50817,#50818),.UNSPECIFIED.,.F.,.F.)
B_SPLINE_CURVE_WITH_KNOTS((6,1,1,1,1,1,1,1,1,1,1,1,1,1,1,1,1,1,1,1,1,6),
(-1.,-0.971428571428572,-0.942857142857143,-0.914285714285714,-0.885714285714286,
-0.857142857142857,-0.828571428571429,-0.8,-0.771428571428572,-0.742857142857143,
-0.714285714285714,-0.685714285714286,-0.657142857142857,-0.628571428571429,
-0.6,-0.571428571428572,-0.542857142857143,-0.514285714285714,-0.485714285714286,
-0.457142857142857,-0.428571428571429,-0.428061295609926),.UNSPECIFIED.)
CURVE()
GEOMETRIC_REPRESENTATION_ITEM()
RATIONAL_B_SPLINE_CURVE((1.,1.,1.,1.,1.,1.,1.,1.,1.,1.,1.,1.,1.,1.,1.,1.,
1.,1.,1.,1.,1.,1.,1.,1.,1.,1.))
REPRESENTATION_ITEM('')
);
#724=(
BOUNDED_CURVE()
B_SPLINE_CURVE(5,(#50822,#50823,#50824,#50825,#50826,#50827,#50828,#50829,
#50830,#50831,#50832,#50833,#50834,#50835,#50836,#50837,#50838,#50839,#50840,
#50841,#50842,#50843,#50844,#50845,#50846,#50847,#50848,#50849,#50850),
 .UNSPECIFIED.,.F.,.F.)
B_SPLINE_CURVE_WITH_KNOTS((6,1,1,1,1,1,1,1,1,1,1,1,1,1,1,1,1,1,1,1,1,1,
1,1,6),(-0.670627588953112,-0.657142857142857,-0.628571428571429,-0.6,-0.571428571428572,
-0.542857142857143,-0.514285714285714,-0.485714285714286,-0.457142857142857,
-0.428571428571429,-0.4,-0.371428571428571,-0.342857142857143,-0.314285714285714,
-0.285714285714286,-0.257142857142857,-0.228571428571429,-0.2,-0.171428571428571,
-0.142857142857143,-0.114285714285714,-0.0857142857142857,-0.0571428571428571,
-0.0285714285714286,0.),.UNSPECIFIED.)
CURVE()
GEOMETRIC_REPRESENTATION_ITEM()
RATIONAL_B_SPLINE_CURVE((1.,1.,1.,1.,1.,1.,1.,1.,1.,1.,1.,1.,1.,1.,1.,1.,
1.,1.,1.,1.,1.,1.,1.,1.,1.,1.,1.,1.,1.))
REPRESENTATION_ITEM('')
);
#725=(
BOUNDED_CURVE()
B_SPLINE_CURVE(5,(#50854,#50855,#50856,#50857,#50858,#50859,#50860,#50861,
#50862,#50863,#50864,#50865,#50866,#50867,#50868,#50869,#50870,#50871,#50872,
#50873,#50874,#50875,#50876,#50877,#50878,#50879),.UNSPECIFIED.,.F.,.F.)
B_SPLINE_CURVE_WITH_KNOTS((6,1,1,1,1,1,1,1,1,1,1,1,1,1,1,1,1,1,1,1,1,6),
(-1.,-0.971428571428572,-0.942857142857143,-0.914285714285714,-0.885714285714286,
-0.857142857142857,-0.828571428571429,-0.8,-0.771428571428572,-0.742857142857143,
-0.714285714285714,-0.685714285714286,-0.657142857142857,-0.628571428571429,
-0.6,-0.571428571428572,-0.542857142857143,-0.514285714285714,-0.485714285714286,
-0.457142857142857,-0.428571428571429,-0.428061295609926),.UNSPECIFIED.)
CURVE()
GEOMETRIC_REPRESENTATION_ITEM()
RATIONAL_B_SPLINE_CURVE((1.,1.,1.,1.,1.,1.,1.,1.,1.,1.,1.,1.,1.,1.,1.,1.,
1.,1.,1.,1.,1.,1.,1.,1.,1.,1.))
REPRESENTATION_ITEM('')
);
#726=(
BOUNDED_CURVE()
B_SPLINE_CURVE(5,(#50883,#50884,#50885,#50886,#50887,#50888,#50889,#50890,
#50891,#50892,#50893,#50894,#50895,#50896,#50897,#50898,#50899,#50900,#50901,
#50902,#50903,#50904,#50905,#50906,#50907,#50908,#50909,#50910,#50911),
 .UNSPECIFIED.,.F.,.F.)
B_SPLINE_CURVE_WITH_KNOTS((6,1,1,1,1,1,1,1,1,1,1,1,1,1,1,1,1,1,1,1,1,1,
1,1,6),(-0.670627588953112,-0.657142857142857,-0.628571428571429,-0.6,-0.571428571428572,
-0.542857142857143,-0.514285714285714,-0.485714285714286,-0.457142857142857,
-0.428571428571429,-0.4,-0.371428571428571,-0.342857142857143,-0.314285714285714,
-0.285714285714286,-0.257142857142857,-0.228571428571429,-0.2,-0.171428571428571,
-0.142857142857143,-0.114285714285714,-0.0857142857142857,-0.0571428571428571,
-0.0285714285714286,0.),.UNSPECIFIED.)
CURVE()
GEOMETRIC_REPRESENTATION_ITEM()
RATIONAL_B_SPLINE_CURVE((1.,1.,1.,1.,1.,1.,1.,1.,1.,1.,1.,1.,1.,1.,1.,1.,
1.,1.,1.,1.,1.,1.,1.,1.,1.,1.,1.,1.,1.))
REPRESENTATION_ITEM('')
);
#727=(
BOUNDED_CURVE()
B_SPLINE_CURVE(5,(#50915,#50916,#50917,#50918,#50919,#50920,#50921,#50922,
#50923,#50924,#50925,#50926,#50927,#50928,#50929,#50930,#50931,#50932,#50933,
#50934,#50935,#50936,#50937,#50938,#50939,#50940),.UNSPECIFIED.,.F.,.F.)
B_SPLINE_CURVE_WITH_KNOTS((6,1,1,1,1,1,1,1,1,1,1,1,1,1,1,1,1,1,1,1,1,6),
(-1.,-0.971428571428572,-0.942857142857143,-0.914285714285714,-0.885714285714286,
-0.857142857142857,-0.828571428571429,-0.8,-0.771428571428572,-0.742857142857143,
-0.714285714285714,-0.685714285714286,-0.657142857142857,-0.628571428571429,
-0.6,-0.571428571428572,-0.542857142857143,-0.514285714285714,-0.485714285714286,
-0.457142857142857,-0.428571428571429,-0.428061295609925),.UNSPECIFIED.)
CURVE()
GEOMETRIC_REPRESENTATION_ITEM()
RATIONAL_B_SPLINE_CURVE((1.,1.,1.,1.,1.,1.,1.,1.,1.,1.,1.,1.,1.,1.,1.,1.,
1.,1.,1.,1.,1.,1.,1.,1.,1.,1.))
REPRESENTATION_ITEM('')
);
#728=(
BOUNDED_CURVE()
B_SPLINE_CURVE(5,(#50944,#50945,#50946,#50947,#50948,#50949,#50950,#50951,
#50952,#50953,#50954,#50955,#50956,#50957,#50958,#50959,#50960,#50961,#50962,
#50963,#50964,#50965,#50966,#50967,#50968,#50969,#50970,#50971,#50972),
 .UNSPECIFIED.,.F.,.F.)
B_SPLINE_CURVE_WITH_KNOTS((6,1,1,1,1,1,1,1,1,1,1,1,1,1,1,1,1,1,1,1,1,1,
1,1,6),(-0.670627588953112,-0.657142857142857,-0.628571428571429,-0.6,-0.571428571428572,
-0.542857142857143,-0.514285714285714,-0.485714285714286,-0.457142857142857,
-0.428571428571429,-0.4,-0.371428571428571,-0.342857142857143,-0.314285714285714,
-0.285714285714286,-0.257142857142857,-0.228571428571429,-0.2,-0.171428571428571,
-0.142857142857143,-0.114285714285714,-0.0857142857142857,-0.0571428571428571,
-0.0285714285714286,0.),.UNSPECIFIED.)
CURVE()
GEOMETRIC_REPRESENTATION_ITEM()
RATIONAL_B_SPLINE_CURVE((1.,1.,1.,1.,1.,1.,1.,1.,1.,1.,1.,1.,1.,1.,1.,1.,
1.,1.,1.,1.,1.,1.,1.,1.,1.,1.,1.,1.,1.))
REPRESENTATION_ITEM('')
);
#729=(
BOUNDED_CURVE()
B_SPLINE_CURVE(5,(#50976,#50977,#50978,#50979,#50980,#50981,#50982,#50983,
#50984,#50985,#50986,#50987,#50988,#50989,#50990,#50991,#50992,#50993,#50994,
#50995,#50996,#50997,#50998,#50999,#51000,#51001),.UNSPECIFIED.,.F.,.F.)
B_SPLINE_CURVE_WITH_KNOTS((6,1,1,1,1,1,1,1,1,1,1,1,1,1,1,1,1,1,1,1,1,6),
(-1.,-0.971428571428572,-0.942857142857143,-0.914285714285714,-0.885714285714286,
-0.857142857142857,-0.828571428571429,-0.8,-0.771428571428572,-0.742857142857143,
-0.714285714285714,-0.685714285714286,-0.657142857142857,-0.628571428571429,
-0.6,-0.571428571428572,-0.542857142857143,-0.514285714285714,-0.485714285714286,
-0.457142857142857,-0.428571428571429,-0.428061295609926),.UNSPECIFIED.)
CURVE()
GEOMETRIC_REPRESENTATION_ITEM()
RATIONAL_B_SPLINE_CURVE((1.,1.,1.,1.,1.,1.,1.,1.,1.,1.,1.,1.,1.,1.,1.,1.,
1.,1.,1.,1.,1.,1.,1.,1.,1.,1.))
REPRESENTATION_ITEM('')
);
#730=(
BOUNDED_CURVE()
B_SPLINE_CURVE(5,(#51005,#51006,#51007,#51008,#51009,#51010,#51011,#51012,
#51013,#51014,#51015,#51016,#51017,#51018,#51019,#51020,#51021,#51022,#51023,
#51024,#51025,#51026,#51027,#51028,#51029,#51030,#51031,#51032,#51033),
 .UNSPECIFIED.,.F.,.F.)
B_SPLINE_CURVE_WITH_KNOTS((6,1,1,1,1,1,1,1,1,1,1,1,1,1,1,1,1,1,1,1,1,1,
1,1,6),(-0.670627588953112,-0.657142857142857,-0.628571428571429,-0.6,-0.571428571428572,
-0.542857142857143,-0.514285714285714,-0.485714285714286,-0.457142857142857,
-0.428571428571429,-0.4,-0.371428571428571,-0.342857142857143,-0.314285714285714,
-0.285714285714286,-0.257142857142857,-0.228571428571429,-0.2,-0.171428571428571,
-0.142857142857143,-0.114285714285714,-0.0857142857142857,-0.0571428571428571,
-0.0285714285714286,0.),.UNSPECIFIED.)
CURVE()
GEOMETRIC_REPRESENTATION_ITEM()
RATIONAL_B_SPLINE_CURVE((1.,1.,1.,1.,1.,1.,1.,1.,1.,1.,1.,1.,1.,1.,1.,1.,
1.,1.,1.,1.,1.,1.,1.,1.,1.,1.,1.,1.,1.))
REPRESENTATION_ITEM('')
);
#731=(
BOUNDED_CURVE()
B_SPLINE_CURVE(5,(#51037,#51038,#51039,#51040,#51041,#51042,#51043,#51044,
#51045,#51046,#51047,#51048,#51049,#51050,#51051,#51052,#51053,#51054,#51055,
#51056,#51057,#51058,#51059,#51060,#51061,#51062),.UNSPECIFIED.,.F.,.F.)
B_SPLINE_CURVE_WITH_KNOTS((6,1,1,1,1,1,1,1,1,1,1,1,1,1,1,1,1,1,1,1,1,6),
(-1.,-0.971428571428572,-0.942857142857143,-0.914285714285714,-0.885714285714286,
-0.857142857142857,-0.828571428571429,-0.8,-0.771428571428572,-0.742857142857143,
-0.714285714285714,-0.685714285714286,-0.657142857142857,-0.628571428571429,
-0.6,-0.571428571428572,-0.542857142857143,-0.514285714285714,-0.485714285714286,
-0.457142857142857,-0.428571428571429,-0.428061295609927),.UNSPECIFIED.)
CURVE()
GEOMETRIC_REPRESENTATION_ITEM()
RATIONAL_B_SPLINE_CURVE((1.,1.,1.,1.,1.,1.,1.,1.,1.,1.,1.,1.,1.,1.,1.,1.,
1.,1.,1.,1.,1.,1.,1.,1.,1.,1.))
REPRESENTATION_ITEM('')
);
#732=(
BOUNDED_CURVE()
B_SPLINE_CURVE(5,(#51066,#51067,#51068,#51069,#51070,#51071,#51072,#51073,
#51074,#51075,#51076,#51077,#51078,#51079,#51080,#51081,#51082,#51083,#51084,
#51085,#51086,#51087,#51088,#51089,#51090,#51091,#51092,#51093,#51094),
 .UNSPECIFIED.,.F.,.F.)
B_SPLINE_CURVE_WITH_KNOTS((6,1,1,1,1,1,1,1,1,1,1,1,1,1,1,1,1,1,1,1,1,1,
1,1,6),(-0.670627588953113,-0.657142857142857,-0.628571428571429,-0.6,-0.571428571428572,
-0.542857142857143,-0.514285714285714,-0.485714285714286,-0.457142857142857,
-0.428571428571429,-0.4,-0.371428571428571,-0.342857142857143,-0.314285714285714,
-0.285714285714286,-0.257142857142857,-0.228571428571429,-0.2,-0.171428571428571,
-0.142857142857143,-0.114285714285714,-0.0857142857142857,-0.0571428571428571,
-0.0285714285714286,0.),.UNSPECIFIED.)
CURVE()
GEOMETRIC_REPRESENTATION_ITEM()
RATIONAL_B_SPLINE_CURVE((1.,1.,1.,1.,1.,1.,1.,1.,1.,1.,1.,1.,1.,1.,1.,1.,
1.,1.,1.,1.,1.,1.,1.,1.,1.,1.,1.,1.,1.))
REPRESENTATION_ITEM('')
);
#733=(
BOUNDED_CURVE()
B_SPLINE_CURVE(5,(#51098,#51099,#51100,#51101,#51102,#51103,#51104,#51105,
#51106,#51107,#51108,#51109,#51110,#51111,#51112,#51113,#51114,#51115,#51116,
#51117,#51118,#51119,#51120,#51121,#51122,#51123),.UNSPECIFIED.,.F.,.F.)
B_SPLINE_CURVE_WITH_KNOTS((6,1,1,1,1,1,1,1,1,1,1,1,1,1,1,1,1,1,1,1,1,6),
(-1.,-0.971428571428572,-0.942857142857143,-0.914285714285714,-0.885714285714286,
-0.857142857142857,-0.828571428571429,-0.8,-0.771428571428572,-0.742857142857143,
-0.714285714285714,-0.685714285714286,-0.657142857142857,-0.628571428571429,
-0.6,-0.571428571428572,-0.542857142857143,-0.514285714285714,-0.485714285714286,
-0.457142857142857,-0.428571428571429,-0.428061295609925),.UNSPECIFIED.)
CURVE()
GEOMETRIC_REPRESENTATION_ITEM()
RATIONAL_B_SPLINE_CURVE((1.,1.,1.,1.,1.,1.,1.,1.,1.,1.,1.,1.,1.,1.,1.,1.,
1.,1.,1.,1.,1.,1.,1.,1.,1.,1.))
REPRESENTATION_ITEM('')
);
#734=(
BOUNDED_CURVE()
B_SPLINE_CURVE(5,(#51127,#51128,#51129,#51130,#51131,#51132,#51133,#51134,
#51135,#51136,#51137,#51138,#51139,#51140,#51141,#51142,#51143,#51144,#51145,
#51146,#51147,#51148,#51149,#51150,#51151,#51152,#51153,#51154,#51155),
 .UNSPECIFIED.,.F.,.F.)
B_SPLINE_CURVE_WITH_KNOTS((6,1,1,1,1,1,1,1,1,1,1,1,1,1,1,1,1,1,1,1,1,1,
1,1,6),(-0.670627588953113,-0.657142857142857,-0.628571428571429,-0.6,-0.571428571428572,
-0.542857142857143,-0.514285714285714,-0.485714285714286,-0.457142857142857,
-0.428571428571429,-0.4,-0.371428571428571,-0.342857142857143,-0.314285714285714,
-0.285714285714286,-0.257142857142857,-0.228571428571429,-0.2,-0.171428571428571,
-0.142857142857143,-0.114285714285714,-0.0857142857142857,-0.0571428571428571,
-0.0285714285714286,0.),.UNSPECIFIED.)
CURVE()
GEOMETRIC_REPRESENTATION_ITEM()
RATIONAL_B_SPLINE_CURVE((1.,1.,1.,1.,1.,1.,1.,1.,1.,1.,1.,1.,1.,1.,1.,1.,
1.,1.,1.,1.,1.,1.,1.,1.,1.,1.,1.,1.,1.))
REPRESENTATION_ITEM('')
);
#735=(
BOUNDED_CURVE()
B_SPLINE_CURVE(5,(#51159,#51160,#51161,#51162,#51163,#51164,#51165,#51166,
#51167,#51168,#51169,#51170,#51171,#51172,#51173,#51174,#51175,#51176,#51177,
#51178,#51179,#51180,#51181,#51182,#51183,#51184),.UNSPECIFIED.,.F.,.F.)
B_SPLINE_CURVE_WITH_KNOTS((6,1,1,1,1,1,1,1,1,1,1,1,1,1,1,1,1,1,1,1,1,6),
(-1.,-0.971428571428572,-0.942857142857143,-0.914285714285714,-0.885714285714286,
-0.857142857142857,-0.828571428571429,-0.8,-0.771428571428572,-0.742857142857143,
-0.714285714285714,-0.685714285714286,-0.657142857142857,-0.628571428571429,
-0.6,-0.571428571428572,-0.542857142857143,-0.514285714285714,-0.485714285714286,
-0.457142857142857,-0.428571428571429,-0.428061295609926),.UNSPECIFIED.)
CURVE()
GEOMETRIC_REPRESENTATION_ITEM()
RATIONAL_B_SPLINE_CURVE((1.,1.,1.,1.,1.,1.,1.,1.,1.,1.,1.,1.,1.,1.,1.,1.,
1.,1.,1.,1.,1.,1.,1.,1.,1.,1.))
REPRESENTATION_ITEM('')
);
#736=(
BOUNDED_CURVE()
B_SPLINE_CURVE(5,(#51188,#51189,#51190,#51191,#51192,#51193,#51194,#51195,
#51196,#51197,#51198,#51199,#51200,#51201,#51202,#51203,#51204,#51205,#51206,
#51207,#51208,#51209,#51210,#51211,#51212,#51213,#51214,#51215,#51216),
 .UNSPECIFIED.,.F.,.F.)
B_SPLINE_CURVE_WITH_KNOTS((6,1,1,1,1,1,1,1,1,1,1,1,1,1,1,1,1,1,1,1,1,1,
1,1,6),(-0.670627588953112,-0.657142857142857,-0.628571428571429,-0.6,-0.571428571428572,
-0.542857142857143,-0.514285714285714,-0.485714285714286,-0.457142857142857,
-0.428571428571429,-0.4,-0.371428571428571,-0.342857142857143,-0.314285714285714,
-0.285714285714286,-0.257142857142857,-0.228571428571429,-0.2,-0.171428571428571,
-0.142857142857143,-0.114285714285714,-0.0857142857142857,-0.0571428571428571,
-0.0285714285714286,0.),.UNSPECIFIED.)
CURVE()
GEOMETRIC_REPRESENTATION_ITEM()
RATIONAL_B_SPLINE_CURVE((1.,1.,1.,1.,1.,1.,1.,1.,1.,1.,1.,1.,1.,1.,1.,1.,
1.,1.,1.,1.,1.,1.,1.,1.,1.,1.,1.,1.,1.))
REPRESENTATION_ITEM('')
);
#737=(
BOUNDED_CURVE()
B_SPLINE_CURVE(5,(#51220,#51221,#51222,#51223,#51224,#51225,#51226,#51227,
#51228,#51229,#51230,#51231,#51232,#51233,#51234,#51235,#51236,#51237,#51238,
#51239,#51240,#51241,#51242,#51243,#51244,#51245),.UNSPECIFIED.,.F.,.F.)
B_SPLINE_CURVE_WITH_KNOTS((6,1,1,1,1,1,1,1,1,1,1,1,1,1,1,1,1,1,1,1,1,6),
(-1.,-0.971428571428572,-0.942857142857143,-0.914285714285714,-0.885714285714286,
-0.857142857142857,-0.828571428571429,-0.8,-0.771428571428572,-0.742857142857143,
-0.714285714285714,-0.685714285714286,-0.657142857142857,-0.628571428571429,
-0.6,-0.571428571428572,-0.542857142857143,-0.514285714285714,-0.485714285714286,
-0.457142857142857,-0.428571428571429,-0.428061295609926),.UNSPECIFIED.)
CURVE()
GEOMETRIC_REPRESENTATION_ITEM()
RATIONAL_B_SPLINE_CURVE((1.,1.,1.,1.,1.,1.,1.,1.,1.,1.,1.,1.,1.,1.,1.,1.,
1.,1.,1.,1.,1.,1.,1.,1.,1.,1.))
REPRESENTATION_ITEM('')
);
#738=(
BOUNDED_CURVE()
B_SPLINE_CURVE(5,(#51249,#51250,#51251,#51252,#51253,#51254,#51255,#51256,
#51257,#51258,#51259,#51260,#51261,#51262,#51263,#51264,#51265,#51266,#51267,
#51268,#51269,#51270,#51271,#51272,#51273,#51274,#51275,#51276,#51277),
 .UNSPECIFIED.,.F.,.F.)
B_SPLINE_CURVE_WITH_KNOTS((6,1,1,1,1,1,1,1,1,1,1,1,1,1,1,1,1,1,1,1,1,1,
1,1,6),(-0.670627588953113,-0.657142857142857,-0.628571428571429,-0.6,-0.571428571428572,
-0.542857142857143,-0.514285714285714,-0.485714285714286,-0.457142857142857,
-0.428571428571429,-0.4,-0.371428571428571,-0.342857142857143,-0.314285714285714,
-0.285714285714286,-0.257142857142857,-0.228571428571429,-0.2,-0.171428571428571,
-0.142857142857143,-0.114285714285714,-0.0857142857142857,-0.0571428571428571,
-0.0285714285714286,0.),.UNSPECIFIED.)
CURVE()
GEOMETRIC_REPRESENTATION_ITEM()
RATIONAL_B_SPLINE_CURVE((1.,1.,1.,1.,1.,1.,1.,1.,1.,1.,1.,1.,1.,1.,1.,1.,
1.,1.,1.,1.,1.,1.,1.,1.,1.,1.,1.,1.,1.))
REPRESENTATION_ITEM('')
);
#739=(
BOUNDED_CURVE()
B_SPLINE_CURVE(5,(#51281,#51282,#51283,#51284,#51285,#51286,#51287,#51288,
#51289,#51290,#51291,#51292,#51293,#51294,#51295,#51296,#51297,#51298,#51299,
#51300,#51301,#51302,#51303,#51304,#51305,#51306),.UNSPECIFIED.,.F.,.F.)
B_SPLINE_CURVE_WITH_KNOTS((6,1,1,1,1,1,1,1,1,1,1,1,1,1,1,1,1,1,1,1,1,6),
(-1.,-0.971428571428572,-0.942857142857143,-0.914285714285714,-0.885714285714286,
-0.857142857142857,-0.828571428571429,-0.8,-0.771428571428572,-0.742857142857143,
-0.714285714285714,-0.685714285714286,-0.657142857142857,-0.628571428571429,
-0.6,-0.571428571428572,-0.542857142857143,-0.514285714285714,-0.485714285714286,
-0.457142857142857,-0.428571428571429,-0.428061295609926),.UNSPECIFIED.)
CURVE()
GEOMETRIC_REPRESENTATION_ITEM()
RATIONAL_B_SPLINE_CURVE((1.,1.,1.,1.,1.,1.,1.,1.,1.,1.,1.,1.,1.,1.,1.,1.,
1.,1.,1.,1.,1.,1.,1.,1.,1.,1.))
REPRESENTATION_ITEM('')
);
#740=(
BOUNDED_CURVE()
B_SPLINE_CURVE(5,(#51310,#51311,#51312,#51313,#51314,#51315,#51316,#51317,
#51318,#51319,#51320,#51321,#51322,#51323,#51324,#51325,#51326,#51327,#51328,
#51329,#51330,#51331,#51332,#51333,#51334,#51335,#51336,#51337,#51338),
 .UNSPECIFIED.,.F.,.F.)
B_SPLINE_CURVE_WITH_KNOTS((6,1,1,1,1,1,1,1,1,1,1,1,1,1,1,1,1,1,1,1,1,1,
1,1,6),(-0.670627588953113,-0.657142857142857,-0.628571428571429,-0.6,-0.571428571428572,
-0.542857142857143,-0.514285714285714,-0.485714285714286,-0.457142857142857,
-0.428571428571429,-0.4,-0.371428571428571,-0.342857142857143,-0.314285714285714,
-0.285714285714286,-0.257142857142857,-0.228571428571429,-0.2,-0.171428571428571,
-0.142857142857143,-0.114285714285714,-0.0857142857142857,-0.0571428571428571,
-0.0285714285714286,0.),.UNSPECIFIED.)
CURVE()
GEOMETRIC_REPRESENTATION_ITEM()
RATIONAL_B_SPLINE_CURVE((1.,1.,1.,1.,1.,1.,1.,1.,1.,1.,1.,1.,1.,1.,1.,1.,
1.,1.,1.,1.,1.,1.,1.,1.,1.,1.,1.,1.,1.))
REPRESENTATION_ITEM('')
);
#741=(
BOUNDED_CURVE()
B_SPLINE_CURVE(5,(#51342,#51343,#51344,#51345,#51346,#51347,#51348,#51349,
#51350,#51351,#51352,#51353,#51354,#51355,#51356,#51357,#51358,#51359,#51360,
#51361,#51362,#51363,#51364,#51365,#51366,#51367),.UNSPECIFIED.,.F.,.F.)
B_SPLINE_CURVE_WITH_KNOTS((6,1,1,1,1,1,1,1,1,1,1,1,1,1,1,1,1,1,1,1,1,6),
(-1.,-0.971428571428572,-0.942857142857143,-0.914285714285714,-0.885714285714286,
-0.857142857142857,-0.828571428571429,-0.8,-0.771428571428572,-0.742857142857143,
-0.714285714285714,-0.685714285714286,-0.657142857142857,-0.628571428571429,
-0.6,-0.571428571428572,-0.542857142857143,-0.514285714285714,-0.485714285714286,
-0.457142857142857,-0.428571428571429,-0.428061295609926),.UNSPECIFIED.)
CURVE()
GEOMETRIC_REPRESENTATION_ITEM()
RATIONAL_B_SPLINE_CURVE((1.,1.,1.,1.,1.,1.,1.,1.,1.,1.,1.,1.,1.,1.,1.,1.,
1.,1.,1.,1.,1.,1.,1.,1.,1.,1.))
REPRESENTATION_ITEM('')
);
#742=(
BOUNDED_CURVE()
B_SPLINE_CURVE(5,(#51371,#51372,#51373,#51374,#51375,#51376,#51377,#51378,
#51379,#51380,#51381,#51382,#51383,#51384,#51385,#51386,#51387,#51388,#51389,
#51390,#51391,#51392,#51393,#51394,#51395,#51396,#51397,#51398,#51399),
 .UNSPECIFIED.,.F.,.F.)
B_SPLINE_CURVE_WITH_KNOTS((6,1,1,1,1,1,1,1,1,1,1,1,1,1,1,1,1,1,1,1,1,1,
1,1,6),(-0.670627588953112,-0.657142857142857,-0.628571428571429,-0.6,-0.571428571428572,
-0.542857142857143,-0.514285714285714,-0.485714285714286,-0.457142857142857,
-0.428571428571429,-0.4,-0.371428571428571,-0.342857142857143,-0.314285714285714,
-0.285714285714286,-0.257142857142857,-0.228571428571429,-0.2,-0.171428571428571,
-0.142857142857143,-0.114285714285714,-0.0857142857142857,-0.0571428571428571,
-0.0285714285714286,0.),.UNSPECIFIED.)
CURVE()
GEOMETRIC_REPRESENTATION_ITEM()
RATIONAL_B_SPLINE_CURVE((1.,1.,1.,1.,1.,1.,1.,1.,1.,1.,1.,1.,1.,1.,1.,1.,
1.,1.,1.,1.,1.,1.,1.,1.,1.,1.,1.,1.,1.))
REPRESENTATION_ITEM('')
);
#743=(
BOUNDED_CURVE()
B_SPLINE_CURVE(5,(#51403,#51404,#51405,#51406,#51407,#51408,#51409,#51410,
#51411,#51412,#51413,#51414,#51415,#51416,#51417,#51418,#51419,#51420,#51421,
#51422,#51423,#51424,#51425,#51426,#51427,#51428),.UNSPECIFIED.,.F.,.F.)
B_SPLINE_CURVE_WITH_KNOTS((6,1,1,1,1,1,1,1,1,1,1,1,1,1,1,1,1,1,1,1,1,6),
(-1.,-0.971428571428572,-0.942857142857143,-0.914285714285714,-0.885714285714286,
-0.857142857142857,-0.828571428571429,-0.8,-0.771428571428572,-0.742857142857143,
-0.714285714285714,-0.685714285714286,-0.657142857142857,-0.628571428571429,
-0.6,-0.571428571428572,-0.542857142857143,-0.514285714285714,-0.485714285714286,
-0.457142857142857,-0.428571428571429,-0.428061295609926),.UNSPECIFIED.)
CURVE()
GEOMETRIC_REPRESENTATION_ITEM()
RATIONAL_B_SPLINE_CURVE((1.,1.,1.,1.,1.,1.,1.,1.,1.,1.,1.,1.,1.,1.,1.,1.,
1.,1.,1.,1.,1.,1.,1.,1.,1.,1.))
REPRESENTATION_ITEM('')
);
#744=(
BOUNDED_CURVE()
B_SPLINE_CURVE(5,(#51432,#51433,#51434,#51435,#51436,#51437,#51438,#51439,
#51440,#51441,#51442,#51443,#51444,#51445,#51446,#51447,#51448,#51449,#51450,
#51451,#51452,#51453,#51454,#51455,#51456,#51457,#51458,#51459,#51460),
 .UNSPECIFIED.,.F.,.F.)
B_SPLINE_CURVE_WITH_KNOTS((6,1,1,1,1,1,1,1,1,1,1,1,1,1,1,1,1,1,1,1,1,1,
1,1,6),(-0.670627588953113,-0.657142857142857,-0.628571428571429,-0.6,-0.571428571428572,
-0.542857142857143,-0.514285714285714,-0.485714285714286,-0.457142857142857,
-0.428571428571429,-0.4,-0.371428571428571,-0.342857142857143,-0.314285714285714,
-0.285714285714286,-0.257142857142857,-0.228571428571429,-0.2,-0.171428571428571,
-0.142857142857143,-0.114285714285714,-0.0857142857142857,-0.0571428571428571,
-0.0285714285714286,0.),.UNSPECIFIED.)
CURVE()
GEOMETRIC_REPRESENTATION_ITEM()
RATIONAL_B_SPLINE_CURVE((1.,1.,1.,1.,1.,1.,1.,1.,1.,1.,1.,1.,1.,1.,1.,1.,
1.,1.,1.,1.,1.,1.,1.,1.,1.,1.,1.,1.,1.))
REPRESENTATION_ITEM('')
);
#745=(
BOUNDED_CURVE()
B_SPLINE_CURVE(5,(#51464,#51465,#51466,#51467,#51468,#51469,#51470,#51471,
#51472,#51473,#51474,#51475,#51476,#51477,#51478,#51479,#51480,#51481,#51482,
#51483,#51484,#51485,#51486,#51487,#51488,#51489),.UNSPECIFIED.,.F.,.F.)
B_SPLINE_CURVE_WITH_KNOTS((6,1,1,1,1,1,1,1,1,1,1,1,1,1,1,1,1,1,1,1,1,6),
(-1.,-0.971428571428572,-0.942857142857143,-0.914285714285714,-0.885714285714286,
-0.857142857142857,-0.828571428571429,-0.8,-0.771428571428572,-0.742857142857143,
-0.714285714285714,-0.685714285714286,-0.657142857142857,-0.628571428571429,
-0.6,-0.571428571428572,-0.542857142857143,-0.514285714285714,-0.485714285714286,
-0.457142857142857,-0.428571428571429,-0.428061295609926),.UNSPECIFIED.)
CURVE()
GEOMETRIC_REPRESENTATION_ITEM()
RATIONAL_B_SPLINE_CURVE((1.,1.,1.,1.,1.,1.,1.,1.,1.,1.,1.,1.,1.,1.,1.,1.,
1.,1.,1.,1.,1.,1.,1.,1.,1.,1.))
REPRESENTATION_ITEM('')
);
#746=(
BOUNDED_CURVE()
B_SPLINE_CURVE(5,(#51493,#51494,#51495,#51496,#51497,#51498,#51499,#51500,
#51501,#51502,#51503,#51504,#51505,#51506,#51507,#51508,#51509,#51510,#51511,
#51512,#51513,#51514,#51515,#51516,#51517,#51518,#51519,#51520,#51521),
 .UNSPECIFIED.,.F.,.F.)
B_SPLINE_CURVE_WITH_KNOTS((6,1,1,1,1,1,1,1,1,1,1,1,1,1,1,1,1,1,1,1,1,1,
1,1,6),(-0.670627588953113,-0.657142857142857,-0.628571428571429,-0.6,-0.571428571428572,
-0.542857142857143,-0.514285714285714,-0.485714285714286,-0.457142857142857,
-0.428571428571429,-0.4,-0.371428571428571,-0.342857142857143,-0.314285714285714,
-0.285714285714286,-0.257142857142857,-0.228571428571429,-0.2,-0.171428571428571,
-0.142857142857143,-0.114285714285714,-0.0857142857142857,-0.0571428571428571,
-0.0285714285714286,0.),.UNSPECIFIED.)
CURVE()
GEOMETRIC_REPRESENTATION_ITEM()
RATIONAL_B_SPLINE_CURVE((1.,1.,1.,1.,1.,1.,1.,1.,1.,1.,1.,1.,1.,1.,1.,1.,
1.,1.,1.,1.,1.,1.,1.,1.,1.,1.,1.,1.,1.))
REPRESENTATION_ITEM('')
);
#747=(
BOUNDED_CURVE()
B_SPLINE_CURVE(5,(#51525,#51526,#51527,#51528,#51529,#51530,#51531,#51532,
#51533,#51534,#51535,#51536,#51537,#51538,#51539,#51540,#51541,#51542,#51543,
#51544,#51545,#51546,#51547,#51548,#51549,#51550),.UNSPECIFIED.,.F.,.F.)
B_SPLINE_CURVE_WITH_KNOTS((6,1,1,1,1,1,1,1,1,1,1,1,1,1,1,1,1,1,1,1,1,6),
(-1.,-0.971428571428572,-0.942857142857143,-0.914285714285714,-0.885714285714286,
-0.857142857142857,-0.828571428571429,-0.8,-0.771428571428572,-0.742857142857143,
-0.714285714285714,-0.685714285714286,-0.657142857142857,-0.628571428571429,
-0.6,-0.571428571428572,-0.542857142857143,-0.514285714285714,-0.485714285714286,
-0.457142857142857,-0.428571428571429,-0.428061295609925),.UNSPECIFIED.)
CURVE()
GEOMETRIC_REPRESENTATION_ITEM()
RATIONAL_B_SPLINE_CURVE((1.,1.,1.,1.,1.,1.,1.,1.,1.,1.,1.,1.,1.,1.,1.,1.,
1.,1.,1.,1.,1.,1.,1.,1.,1.,1.))
REPRESENTATION_ITEM('')
);
#748=(
BOUNDED_CURVE()
B_SPLINE_CURVE(5,(#51554,#51555,#51556,#51557,#51558,#51559,#51560,#51561,
#51562,#51563,#51564,#51565,#51566,#51567,#51568,#51569,#51570,#51571,#51572,
#51573,#51574,#51575,#51576,#51577,#51578,#51579,#51580,#51581,#51582),
 .UNSPECIFIED.,.F.,.F.)
B_SPLINE_CURVE_WITH_KNOTS((6,1,1,1,1,1,1,1,1,1,1,1,1,1,1,1,1,1,1,1,1,1,
1,1,6),(-0.670627588953112,-0.657142857142857,-0.628571428571429,-0.6,-0.571428571428572,
-0.542857142857143,-0.514285714285714,-0.485714285714286,-0.457142857142857,
-0.428571428571429,-0.4,-0.371428571428571,-0.342857142857143,-0.314285714285714,
-0.285714285714286,-0.257142857142857,-0.228571428571429,-0.2,-0.171428571428571,
-0.142857142857143,-0.114285714285714,-0.0857142857142857,-0.0571428571428571,
-0.0285714285714286,0.),.UNSPECIFIED.)
CURVE()
GEOMETRIC_REPRESENTATION_ITEM()
RATIONAL_B_SPLINE_CURVE((1.,1.,1.,1.,1.,1.,1.,1.,1.,1.,1.,1.,1.,1.,1.,1.,
1.,1.,1.,1.,1.,1.,1.,1.,1.,1.,1.,1.,1.))
REPRESENTATION_ITEM('')
);
#749=(
BOUNDED_CURVE()
B_SPLINE_CURVE(5,(#51586,#51587,#51588,#51589,#51590,#51591,#51592,#51593,
#51594,#51595,#51596,#51597,#51598,#51599,#51600,#51601,#51602,#51603,#51604,
#51605,#51606,#51607,#51608,#51609,#51610,#51611),.UNSPECIFIED.,.F.,.F.)
B_SPLINE_CURVE_WITH_KNOTS((6,1,1,1,1,1,1,1,1,1,1,1,1,1,1,1,1,1,1,1,1,6),
(-1.,-0.971428571428572,-0.942857142857143,-0.914285714285714,-0.885714285714286,
-0.857142857142857,-0.828571428571429,-0.8,-0.771428571428572,-0.742857142857143,
-0.714285714285714,-0.685714285714286,-0.657142857142857,-0.628571428571429,
-0.6,-0.571428571428572,-0.542857142857143,-0.514285714285714,-0.485714285714286,
-0.457142857142857,-0.428571428571429,-0.428061295609926),.UNSPECIFIED.)
CURVE()
GEOMETRIC_REPRESENTATION_ITEM()
RATIONAL_B_SPLINE_CURVE((1.,1.,1.,1.,1.,1.,1.,1.,1.,1.,1.,1.,1.,1.,1.,1.,
1.,1.,1.,1.,1.,1.,1.,1.,1.,1.))
REPRESENTATION_ITEM('')
);
#750=(
BOUNDED_CURVE()
B_SPLINE_CURVE(5,(#51704,#51705,#51706,#51707,#51708,#51709,#51710,#51711,
#51712,#51713,#51714,#51715,#51716,#51717,#51718,#51719,#51720,#51721,#51722,
#51723,#51724,#51725,#51726,#51727,#51728,#51729,#51730,#51731,#51732,#51733,
#51734,#51735,#51736,#51737),.UNSPECIFIED.,.F.,.F.)
B_SPLINE_CURVE_WITH_KNOTS((6,1,1,1,1,1,1,1,1,1,1,1,1,1,1,1,1,1,1,1,1,1,
1,1,1,1,1,1,1,6),(0.,0.0285714285714286,0.0571428571428571,0.0857142857142857,
0.114285714285714,0.142857142857143,0.171428571428571,0.2,0.228571428571429,
0.257142857142857,0.285714285714286,0.314285714285714,0.342857142857143,
0.371428571428571,0.4,0.428571428571429,0.457142857142857,0.485714285714286,
0.514285714285714,0.542857142857143,0.571428571428572,0.6,0.628571428571429,
0.657142857142857,0.685714285714286,0.714285714285714,0.742857142857143,
0.771428571428572,0.8,0.816564825616131),.UNSPECIFIED.)
CURVE()
GEOMETRIC_REPRESENTATION_ITEM()
RATIONAL_B_SPLINE_CURVE((1.,1.,1.,1.,1.,1.,1.,1.,1.,1.,1.,1.,1.,1.,1.,1.,
1.,1.,1.,1.,1.,1.,1.,1.,1.,1.,1.,1.,1.,1.,1.,1.,1.,1.))
REPRESENTATION_ITEM('')
);
#751=(
BOUNDED_CURVE()
B_SPLINE_CURVE(5,(#51842,#51843,#51844,#51845,#51846,#51847,#51848,#51849,
#51850,#51851,#51852,#51853,#51854,#51855,#51856,#51857,#51858,#51859,#51860,
#51861,#51862,#51863,#51864,#51865,#51866,#51867,#51868,#51869,#51870),
 .UNSPECIFIED.,.F.,.F.)
B_SPLINE_CURVE_WITH_KNOTS((6,1,1,1,1,1,1,1,1,1,1,1,1,1,1,1,1,1,1,1,1,1,
1,1,6),(0.315728291775709,0.342857142857143,0.371428571428571,0.4,0.428571428571429,
0.457142857142857,0.485714285714286,0.514285714285714,0.542857142857143,
0.571428571428572,0.6,0.628571428571429,0.657142857142857,0.685714285714286,
0.714285714285714,0.742857142857143,0.771428571428572,0.8,0.828571428571429,
0.857142857142857,0.885714285714286,0.914285714285714,0.942857142857143,
0.971428571428572,1.),.UNSPECIFIED.)
CURVE()
GEOMETRIC_REPRESENTATION_ITEM()
RATIONAL_B_SPLINE_CURVE((1.,1.,1.,1.,1.,1.,1.,1.,1.,1.,1.,1.,1.,1.,1.,1.,
1.,1.,1.,1.,1.,1.,1.,1.,1.,1.,1.,1.,1.))
REPRESENTATION_ITEM('')
);
#752=(
BOUNDED_CURVE()
B_SPLINE_CURVE(5,(#51978,#51979,#51980,#51981,#51982,#51983,#51984,#51985,
#51986,#51987,#51988,#51989,#51990,#51991,#51992,#51993,#51994,#51995,#51996,
#51997,#51998,#51999,#52000,#52001,#52002,#52003,#52004,#52005,#52006),
 .UNSPECIFIED.,.F.,.F.)
B_SPLINE_CURVE_WITH_KNOTS((6,1,1,1,1,1,1,1,1,1,1,1,1,1,1,1,1,1,1,1,1,1,
1,1,6),(0.315728291775709,0.342857142857143,0.371428571428571,0.4,0.428571428571429,
0.457142857142857,0.485714285714286,0.514285714285714,0.542857142857143,
0.571428571428572,0.6,0.628571428571429,0.657142857142857,0.685714285714286,
0.714285714285714,0.742857142857143,0.771428571428572,0.8,0.828571428571429,
0.857142857142857,0.885714285714286,0.914285714285714,0.942857142857143,
0.971428571428572,1.),.UNSPECIFIED.)
CURVE()
GEOMETRIC_REPRESENTATION_ITEM()
RATIONAL_B_SPLINE_CURVE((1.,1.,1.,1.,1.,1.,1.,1.,1.,1.,1.,1.,1.,1.,1.,1.,
1.,1.,1.,1.,1.,1.,1.,1.,1.,1.,1.,1.,1.))
REPRESENTATION_ITEM('')
);
#753=(
BOUNDED_CURVE()
B_SPLINE_CURVE(5,(#52110,#52111,#52112,#52113,#52114,#52115,#52116,#52117,
#52118,#52119,#52120,#52121,#52122,#52123,#52124,#52125,#52126,#52127,#52128,
#52129,#52130,#52131,#52132,#52133,#52134,#52135,#52136,#52137,#52138,#52139,
#52140,#52141,#52142,#52143),.UNSPECIFIED.,.F.,.F.)
B_SPLINE_CURVE_WITH_KNOTS((6,1,1,1,1,1,1,1,1,1,1,1,1,1,1,1,1,1,1,1,1,1,
1,1,1,1,1,1,1,6),(0.,0.0285714285714286,0.0571428571428571,0.0857142857142857,
0.114285714285714,0.142857142857143,0.171428571428571,0.2,0.228571428571429,
0.257142857142857,0.285714285714286,0.314285714285714,0.342857142857143,
0.371428571428571,0.4,0.428571428571429,0.457142857142857,0.485714285714286,
0.514285714285714,0.542857142857143,0.571428571428572,0.6,0.628571428571429,
0.657142857142857,0.685714285714286,0.714285714285714,0.742857142857143,
0.771428571428572,0.8,0.816564825616034),.UNSPECIFIED.)
CURVE()
GEOMETRIC_REPRESENTATION_ITEM()
RATIONAL_B_SPLINE_CURVE((1.,1.,1.,1.,1.,1.,1.,1.,1.,1.,1.,1.,1.,1.,1.,1.,
1.,1.,1.,1.,1.,1.,1.,1.,1.,1.,1.,1.,1.,1.,1.,1.,1.,1.))
REPRESENTATION_ITEM('')
);
#754=(
BOUNDED_CURVE()
B_SPLINE_CURVE(5,(#52147,#52148,#52149,#52150,#52151,#52152,#52153,#52154,
#52155,#52156,#52157,#52158,#52159,#52160,#52161,#52162,#52163,#52164,#52165,
#52166,#52167,#52168,#52169,#52170,#52171,#52172,#52173,#52174,#52175),
 .UNSPECIFIED.,.F.,.F.)
B_SPLINE_CURVE_WITH_KNOTS((6,1,1,1,1,1,1,1,1,1,1,1,1,1,1,1,1,1,1,1,1,1,
1,1,6),(0.,0.0285714285714286,0.0571428571428571,0.0857142857142857,0.114285714285714,
0.142857142857143,0.171428571428571,0.2,0.228571428571429,0.257142857142857,
0.285714285714286,0.314285714285714,0.342857142857143,0.371428571428571,
0.4,0.428571428571429,0.457142857142857,0.485714285714286,0.514285714285714,
0.542857142857143,0.571428571428572,0.6,0.628571428571429,0.657142857142857,
0.670627588953113),.UNSPECIFIED.)
CURVE()
GEOMETRIC_REPRESENTATION_ITEM()
RATIONAL_B_SPLINE_CURVE((1.,1.,1.,1.,1.,1.,1.,1.,1.,1.,1.,1.,1.,1.,1.,1.,
1.,1.,1.,1.,1.,1.,1.,1.,1.,1.,1.,1.,1.))
REPRESENTATION_ITEM('')
);
#755=(
BOUNDED_CURVE()
B_SPLINE_CURVE(5,(#52179,#52180,#52181,#52182,#52183,#52184,#52185,#52186,
#52187,#52188,#52189,#52190,#52191,#52192,#52193,#52194,#52195,#52196,#52197,
#52198,#52199,#52200,#52201,#52202,#52203,#52204),.UNSPECIFIED.,.F.,.F.)
B_SPLINE_CURVE_WITH_KNOTS((6,1,1,1,1,1,1,1,1,1,1,1,1,1,1,1,1,1,1,1,1,6),
(0.428061295609926,0.428571428571429,0.457142857142857,0.485714285714286,
0.514285714285714,0.542857142857143,0.571428571428572,0.6,0.628571428571429,
0.657142857142857,0.685714285714286,0.714285714285714,0.742857142857143,
0.771428571428572,0.8,0.828571428571429,0.857142857142857,0.885714285714286,
0.914285714285714,0.942857142857143,0.971428571428572,1.),.UNSPECIFIED.)
CURVE()
GEOMETRIC_REPRESENTATION_ITEM()
RATIONAL_B_SPLINE_CURVE((1.,1.,1.,1.,1.,1.,1.,1.,1.,1.,1.,1.,1.,1.,1.,1.,
1.,1.,1.,1.,1.,1.,1.,1.,1.,1.))
REPRESENTATION_ITEM('')
);
#756=(
BOUNDED_CURVE()
B_SPLINE_CURVE(5,(#52208,#52209,#52210,#52211,#52212,#52213,#52214,#52215,
#52216,#52217,#52218,#52219,#52220,#52221,#52222,#52223,#52224,#52225,#52226,
#52227,#52228,#52229,#52230,#52231,#52232,#52233,#52234,#52235,#52236),
 .UNSPECIFIED.,.F.,.F.)
B_SPLINE_CURVE_WITH_KNOTS((6,1,1,1,1,1,1,1,1,1,1,1,1,1,1,1,1,1,1,1,1,1,
1,1,6),(0.,0.0285714285714286,0.0571428571428571,0.0857142857142857,0.114285714285714,
0.142857142857143,0.171428571428571,0.2,0.228571428571429,0.257142857142857,
0.285714285714286,0.314285714285714,0.342857142857143,0.371428571428571,
0.4,0.428571428571429,0.457142857142857,0.485714285714286,0.514285714285714,
0.542857142857143,0.571428571428572,0.6,0.628571428571429,0.657142857142857,
0.670627588953112),.UNSPECIFIED.)
CURVE()
GEOMETRIC_REPRESENTATION_ITEM()
RATIONAL_B_SPLINE_CURVE((1.,1.,1.,1.,1.,1.,1.,1.,1.,1.,1.,1.,1.,1.,1.,1.,
1.,1.,1.,1.,1.,1.,1.,1.,1.,1.,1.,1.,1.))
REPRESENTATION_ITEM('')
);
#757=(
BOUNDED_CURVE()
B_SPLINE_CURVE(5,(#52240,#52241,#52242,#52243,#52244,#52245,#52246,#52247,
#52248,#52249,#52250,#52251,#52252,#52253,#52254,#52255,#52256,#52257,#52258,
#52259,#52260,#52261,#52262,#52263,#52264,#52265),.UNSPECIFIED.,.F.,.F.)
B_SPLINE_CURVE_WITH_KNOTS((6,1,1,1,1,1,1,1,1,1,1,1,1,1,1,1,1,1,1,1,1,6),
(0.428061295609925,0.428571428571429,0.457142857142857,0.485714285714286,
0.514285714285714,0.542857142857143,0.571428571428572,0.6,0.628571428571429,
0.657142857142857,0.685714285714286,0.714285714285714,0.742857142857143,
0.771428571428572,0.8,0.828571428571429,0.857142857142857,0.885714285714286,
0.914285714285714,0.942857142857143,0.971428571428572,1.),.UNSPECIFIED.)
CURVE()
GEOMETRIC_REPRESENTATION_ITEM()
RATIONAL_B_SPLINE_CURVE((1.,1.,1.,1.,1.,1.,1.,1.,1.,1.,1.,1.,1.,1.,1.,1.,
1.,1.,1.,1.,1.,1.,1.,1.,1.,1.))
REPRESENTATION_ITEM('')
);
#758=(
BOUNDED_CURVE()
B_SPLINE_CURVE(5,(#52269,#52270,#52271,#52272,#52273,#52274,#52275,#52276,
#52277,#52278,#52279,#52280,#52281,#52282,#52283,#52284,#52285,#52286,#52287,
#52288,#52289,#52290,#52291,#52292,#52293,#52294,#52295,#52296,#52297),
 .UNSPECIFIED.,.F.,.F.)
B_SPLINE_CURVE_WITH_KNOTS((6,1,1,1,1,1,1,1,1,1,1,1,1,1,1,1,1,1,1,1,1,1,
1,1,6),(0.,0.0285714285714286,0.0571428571428571,0.0857142857142857,0.114285714285714,
0.142857142857143,0.171428571428571,0.2,0.228571428571429,0.257142857142857,
0.285714285714286,0.314285714285714,0.342857142857143,0.371428571428571,
0.4,0.428571428571429,0.457142857142857,0.485714285714286,0.514285714285714,
0.542857142857143,0.571428571428572,0.6,0.628571428571429,0.657142857142857,
0.670627588953113),.UNSPECIFIED.)
CURVE()
GEOMETRIC_REPRESENTATION_ITEM()
RATIONAL_B_SPLINE_CURVE((1.,1.,1.,1.,1.,1.,1.,1.,1.,1.,1.,1.,1.,1.,1.,1.,
1.,1.,1.,1.,1.,1.,1.,1.,1.,1.,1.,1.,1.))
REPRESENTATION_ITEM('')
);
#759=(
BOUNDED_CURVE()
B_SPLINE_CURVE(5,(#52301,#52302,#52303,#52304,#52305,#52306,#52307,#52308,
#52309,#52310,#52311,#52312,#52313,#52314,#52315,#52316,#52317,#52318,#52319,
#52320,#52321,#52322,#52323,#52324,#52325,#52326),.UNSPECIFIED.,.F.,.F.)
B_SPLINE_CURVE_WITH_KNOTS((6,1,1,1,1,1,1,1,1,1,1,1,1,1,1,1,1,1,1,1,1,6),
(0.428061295609926,0.428571428571429,0.457142857142857,0.485714285714286,
0.514285714285714,0.542857142857143,0.571428571428572,0.6,0.628571428571429,
0.657142857142857,0.685714285714286,0.714285714285714,0.742857142857143,
0.771428571428572,0.8,0.828571428571429,0.857142857142857,0.885714285714286,
0.914285714285714,0.942857142857143,0.971428571428572,1.),.UNSPECIFIED.)
CURVE()
GEOMETRIC_REPRESENTATION_ITEM()
RATIONAL_B_SPLINE_CURVE((1.,1.,1.,1.,1.,1.,1.,1.,1.,1.,1.,1.,1.,1.,1.,1.,
1.,1.,1.,1.,1.,1.,1.,1.,1.,1.))
REPRESENTATION_ITEM('')
);
#760=(
BOUNDED_CURVE()
B_SPLINE_CURVE(5,(#52330,#52331,#52332,#52333,#52334,#52335,#52336,#52337,
#52338,#52339,#52340,#52341,#52342,#52343,#52344,#52345,#52346,#52347,#52348,
#52349,#52350,#52351,#52352,#52353,#52354,#52355,#52356,#52357,#52358),
 .UNSPECIFIED.,.F.,.F.)
B_SPLINE_CURVE_WITH_KNOTS((6,1,1,1,1,1,1,1,1,1,1,1,1,1,1,1,1,1,1,1,1,1,
1,1,6),(0.,0.0285714285714286,0.0571428571428571,0.0857142857142857,0.114285714285714,
0.142857142857143,0.171428571428571,0.2,0.228571428571429,0.257142857142857,
0.285714285714286,0.314285714285714,0.342857142857143,0.371428571428571,
0.4,0.428571428571429,0.457142857142857,0.485714285714286,0.514285714285714,
0.542857142857143,0.571428571428572,0.6,0.628571428571429,0.657142857142857,
0.670627588953113),.UNSPECIFIED.)
CURVE()
GEOMETRIC_REPRESENTATION_ITEM()
RATIONAL_B_SPLINE_CURVE((1.,1.,1.,1.,1.,1.,1.,1.,1.,1.,1.,1.,1.,1.,1.,1.,
1.,1.,1.,1.,1.,1.,1.,1.,1.,1.,1.,1.,1.))
REPRESENTATION_ITEM('')
);
#761=(
BOUNDED_CURVE()
B_SPLINE_CURVE(5,(#52362,#52363,#52364,#52365,#52366,#52367,#52368,#52369,
#52370,#52371,#52372,#52373,#52374,#52375,#52376,#52377,#52378,#52379,#52380,
#52381,#52382,#52383,#52384,#52385,#52386,#52387),.UNSPECIFIED.,.F.,.F.)
B_SPLINE_CURVE_WITH_KNOTS((6,1,1,1,1,1,1,1,1,1,1,1,1,1,1,1,1,1,1,1,1,6),
(0.428061295609926,0.428571428571429,0.457142857142857,0.485714285714286,
0.514285714285714,0.542857142857143,0.571428571428572,0.6,0.628571428571429,
0.657142857142857,0.685714285714286,0.714285714285714,0.742857142857143,
0.771428571428572,0.8,0.828571428571429,0.857142857142857,0.885714285714286,
0.914285714285714,0.942857142857143,0.971428571428572,1.),.UNSPECIFIED.)
CURVE()
GEOMETRIC_REPRESENTATION_ITEM()
RATIONAL_B_SPLINE_CURVE((1.,1.,1.,1.,1.,1.,1.,1.,1.,1.,1.,1.,1.,1.,1.,1.,
1.,1.,1.,1.,1.,1.,1.,1.,1.,1.))
REPRESENTATION_ITEM('')
);
#762=(
BOUNDED_CURVE()
B_SPLINE_CURVE(5,(#52391,#52392,#52393,#52394,#52395,#52396,#52397,#52398,
#52399,#52400,#52401,#52402,#52403,#52404,#52405,#52406,#52407,#52408,#52409,
#52410,#52411,#52412,#52413,#52414,#52415,#52416,#52417,#52418,#52419),
 .UNSPECIFIED.,.F.,.F.)
B_SPLINE_CURVE_WITH_KNOTS((6,1,1,1,1,1,1,1,1,1,1,1,1,1,1,1,1,1,1,1,1,1,
1,1,6),(0.,0.0285714285714286,0.0571428571428571,0.0857142857142857,0.114285714285714,
0.142857142857143,0.171428571428571,0.2,0.228571428571429,0.257142857142857,
0.285714285714286,0.314285714285714,0.342857142857143,0.371428571428571,
0.4,0.428571428571429,0.457142857142857,0.485714285714286,0.514285714285714,
0.542857142857143,0.571428571428572,0.6,0.628571428571429,0.657142857142857,
0.670627588953112),.UNSPECIFIED.)
CURVE()
GEOMETRIC_REPRESENTATION_ITEM()
RATIONAL_B_SPLINE_CURVE((1.,1.,1.,1.,1.,1.,1.,1.,1.,1.,1.,1.,1.,1.,1.,1.,
1.,1.,1.,1.,1.,1.,1.,1.,1.,1.,1.,1.,1.))
REPRESENTATION_ITEM('')
);
#763=(
BOUNDED_CURVE()
B_SPLINE_CURVE(5,(#52423,#52424,#52425,#52426,#52427,#52428,#52429,#52430,
#52431,#52432,#52433,#52434,#52435,#52436,#52437,#52438,#52439,#52440,#52441,
#52442,#52443,#52444,#52445,#52446,#52447,#52448),.UNSPECIFIED.,.F.,.F.)
B_SPLINE_CURVE_WITH_KNOTS((6,1,1,1,1,1,1,1,1,1,1,1,1,1,1,1,1,1,1,1,1,6),
(0.428061295609926,0.428571428571429,0.457142857142857,0.485714285714286,
0.514285714285714,0.542857142857143,0.571428571428572,0.6,0.628571428571429,
0.657142857142857,0.685714285714286,0.714285714285714,0.742857142857143,
0.771428571428572,0.8,0.828571428571429,0.857142857142857,0.885714285714286,
0.914285714285714,0.942857142857143,0.971428571428572,1.),.UNSPECIFIED.)
CURVE()
GEOMETRIC_REPRESENTATION_ITEM()
RATIONAL_B_SPLINE_CURVE((1.,1.,1.,1.,1.,1.,1.,1.,1.,1.,1.,1.,1.,1.,1.,1.,
1.,1.,1.,1.,1.,1.,1.,1.,1.,1.))
REPRESENTATION_ITEM('')
);
#764=(
BOUNDED_CURVE()
B_SPLINE_CURVE(5,(#52452,#52453,#52454,#52455,#52456,#52457,#52458,#52459,
#52460,#52461,#52462,#52463,#52464,#52465,#52466,#52467,#52468,#52469,#52470,
#52471,#52472,#52473,#52474,#52475,#52476,#52477,#52478,#52479,#52480),
 .UNSPECIFIED.,.F.,.F.)
B_SPLINE_CURVE_WITH_KNOTS((6,1,1,1,1,1,1,1,1,1,1,1,1,1,1,1,1,1,1,1,1,1,
1,1,6),(0.,0.0285714285714286,0.0571428571428571,0.0857142857142857,0.114285714285714,
0.142857142857143,0.171428571428571,0.2,0.228571428571429,0.257142857142857,
0.285714285714286,0.314285714285714,0.342857142857143,0.371428571428571,
0.4,0.428571428571429,0.457142857142857,0.485714285714286,0.514285714285714,
0.542857142857143,0.571428571428572,0.6,0.628571428571429,0.657142857142857,
0.670627588953113),.UNSPECIFIED.)
CURVE()
GEOMETRIC_REPRESENTATION_ITEM()
RATIONAL_B_SPLINE_CURVE((1.,1.,1.,1.,1.,1.,1.,1.,1.,1.,1.,1.,1.,1.,1.,1.,
1.,1.,1.,1.,1.,1.,1.,1.,1.,1.,1.,1.,1.))
REPRESENTATION_ITEM('')
);
#765=(
BOUNDED_CURVE()
B_SPLINE_CURVE(5,(#52484,#52485,#52486,#52487,#52488,#52489,#52490,#52491,
#52492,#52493,#52494,#52495,#52496,#52497,#52498,#52499,#52500,#52501,#52502,
#52503,#52504,#52505,#52506,#52507,#52508,#52509),.UNSPECIFIED.,.F.,.F.)
B_SPLINE_CURVE_WITH_KNOTS((6,1,1,1,1,1,1,1,1,1,1,1,1,1,1,1,1,1,1,1,1,6),
(0.428061295609926,0.428571428571429,0.457142857142857,0.485714285714286,
0.514285714285714,0.542857142857143,0.571428571428572,0.6,0.628571428571429,
0.657142857142857,0.685714285714286,0.714285714285714,0.742857142857143,
0.771428571428572,0.8,0.828571428571429,0.857142857142857,0.885714285714286,
0.914285714285714,0.942857142857143,0.971428571428572,1.),.UNSPECIFIED.)
CURVE()
GEOMETRIC_REPRESENTATION_ITEM()
RATIONAL_B_SPLINE_CURVE((1.,1.,1.,1.,1.,1.,1.,1.,1.,1.,1.,1.,1.,1.,1.,1.,
1.,1.,1.,1.,1.,1.,1.,1.,1.,1.))
REPRESENTATION_ITEM('')
);
#766=(
BOUNDED_CURVE()
B_SPLINE_CURVE(5,(#52513,#52514,#52515,#52516,#52517,#52518,#52519,#52520,
#52521,#52522,#52523,#52524,#52525,#52526,#52527,#52528,#52529,#52530,#52531,
#52532,#52533,#52534,#52535,#52536,#52537,#52538,#52539,#52540,#52541),
 .UNSPECIFIED.,.F.,.F.)
B_SPLINE_CURVE_WITH_KNOTS((6,1,1,1,1,1,1,1,1,1,1,1,1,1,1,1,1,1,1,1,1,1,
1,1,6),(0.,0.0285714285714286,0.0571428571428571,0.0857142857142857,0.114285714285714,
0.142857142857143,0.171428571428571,0.2,0.228571428571429,0.257142857142857,
0.285714285714286,0.314285714285714,0.342857142857143,0.371428571428571,
0.4,0.428571428571429,0.457142857142857,0.485714285714286,0.514285714285714,
0.542857142857143,0.571428571428572,0.6,0.628571428571429,0.657142857142857,
0.670627588953113),.UNSPECIFIED.)
CURVE()
GEOMETRIC_REPRESENTATION_ITEM()
RATIONAL_B_SPLINE_CURVE((1.,1.,1.,1.,1.,1.,1.,1.,1.,1.,1.,1.,1.,1.,1.,1.,
1.,1.,1.,1.,1.,1.,1.,1.,1.,1.,1.,1.,1.))
REPRESENTATION_ITEM('')
);
#767=(
BOUNDED_CURVE()
B_SPLINE_CURVE(5,(#52545,#52546,#52547,#52548,#52549,#52550,#52551,#52552,
#52553,#52554,#52555,#52556,#52557,#52558,#52559,#52560,#52561,#52562,#52563,
#52564,#52565,#52566,#52567,#52568,#52569,#52570),.UNSPECIFIED.,.F.,.F.)
B_SPLINE_CURVE_WITH_KNOTS((6,1,1,1,1,1,1,1,1,1,1,1,1,1,1,1,1,1,1,1,1,6),
(0.428061295609926,0.428571428571429,0.457142857142857,0.485714285714286,
0.514285714285714,0.542857142857143,0.571428571428572,0.6,0.628571428571429,
0.657142857142857,0.685714285714286,0.714285714285714,0.742857142857143,
0.771428571428572,0.8,0.828571428571429,0.857142857142857,0.885714285714286,
0.914285714285714,0.942857142857143,0.971428571428572,1.),.UNSPECIFIED.)
CURVE()
GEOMETRIC_REPRESENTATION_ITEM()
RATIONAL_B_SPLINE_CURVE((1.,1.,1.,1.,1.,1.,1.,1.,1.,1.,1.,1.,1.,1.,1.,1.,
1.,1.,1.,1.,1.,1.,1.,1.,1.,1.))
REPRESENTATION_ITEM('')
);
#768=(
BOUNDED_CURVE()
B_SPLINE_CURVE(5,(#52574,#52575,#52576,#52577,#52578,#52579,#52580,#52581,
#52582,#52583,#52584,#52585,#52586,#52587,#52588,#52589,#52590,#52591,#52592,
#52593,#52594,#52595,#52596,#52597,#52598,#52599,#52600,#52601,#52602),
 .UNSPECIFIED.,.F.,.F.)
B_SPLINE_CURVE_WITH_KNOTS((6,1,1,1,1,1,1,1,1,1,1,1,1,1,1,1,1,1,1,1,1,1,
1,1,6),(0.,0.0285714285714286,0.0571428571428571,0.0857142857142857,0.114285714285714,
0.142857142857143,0.171428571428571,0.2,0.228571428571429,0.257142857142857,
0.285714285714286,0.314285714285714,0.342857142857143,0.371428571428571,
0.4,0.428571428571429,0.457142857142857,0.485714285714286,0.514285714285714,
0.542857142857143,0.571428571428572,0.6,0.628571428571429,0.657142857142857,
0.670627588953112),.UNSPECIFIED.)
CURVE()
GEOMETRIC_REPRESENTATION_ITEM()
RATIONAL_B_SPLINE_CURVE((1.,1.,1.,1.,1.,1.,1.,1.,1.,1.,1.,1.,1.,1.,1.,1.,
1.,1.,1.,1.,1.,1.,1.,1.,1.,1.,1.,1.,1.))
REPRESENTATION_ITEM('')
);
#769=(
BOUNDED_CURVE()
B_SPLINE_CURVE(5,(#52606,#52607,#52608,#52609,#52610,#52611,#52612,#52613,
#52614,#52615,#52616,#52617,#52618,#52619,#52620,#52621,#52622,#52623,#52624,
#52625,#52626,#52627,#52628,#52629,#52630,#52631),.UNSPECIFIED.,.F.,.F.)
B_SPLINE_CURVE_WITH_KNOTS((6,1,1,1,1,1,1,1,1,1,1,1,1,1,1,1,1,1,1,1,1,6),
(0.428061295609926,0.428571428571429,0.457142857142857,0.485714285714286,
0.514285714285714,0.542857142857143,0.571428571428572,0.6,0.628571428571429,
0.657142857142857,0.685714285714286,0.714285714285714,0.742857142857143,
0.771428571428572,0.8,0.828571428571429,0.857142857142857,0.885714285714286,
0.914285714285714,0.942857142857143,0.971428571428572,1.),.UNSPECIFIED.)
CURVE()
GEOMETRIC_REPRESENTATION_ITEM()
RATIONAL_B_SPLINE_CURVE((1.,1.,1.,1.,1.,1.,1.,1.,1.,1.,1.,1.,1.,1.,1.,1.,
1.,1.,1.,1.,1.,1.,1.,1.,1.,1.))
REPRESENTATION_ITEM('')
);
#770=(
BOUNDED_CURVE()
B_SPLINE_CURVE(5,(#52635,#52636,#52637,#52638,#52639,#52640,#52641,#52642,
#52643,#52644,#52645,#52646,#52647,#52648,#52649,#52650,#52651,#52652,#52653,
#52654,#52655,#52656,#52657,#52658,#52659,#52660,#52661,#52662,#52663),
 .UNSPECIFIED.,.F.,.F.)
B_SPLINE_CURVE_WITH_KNOTS((6,1,1,1,1,1,1,1,1,1,1,1,1,1,1,1,1,1,1,1,1,1,
1,1,6),(0.,0.0285714285714286,0.0571428571428571,0.0857142857142857,0.114285714285714,
0.142857142857143,0.171428571428571,0.2,0.228571428571429,0.257142857142857,
0.285714285714286,0.314285714285714,0.342857142857143,0.371428571428571,
0.4,0.428571428571429,0.457142857142857,0.485714285714286,0.514285714285714,
0.542857142857143,0.571428571428572,0.6,0.628571428571429,0.657142857142857,
0.670627588953113),.UNSPECIFIED.)
CURVE()
GEOMETRIC_REPRESENTATION_ITEM()
RATIONAL_B_SPLINE_CURVE((1.,1.,1.,1.,1.,1.,1.,1.,1.,1.,1.,1.,1.,1.,1.,1.,
1.,1.,1.,1.,1.,1.,1.,1.,1.,1.,1.,1.,1.))
REPRESENTATION_ITEM('')
);
#771=(
BOUNDED_CURVE()
B_SPLINE_CURVE(5,(#52667,#52668,#52669,#52670,#52671,#52672,#52673,#52674,
#52675,#52676,#52677,#52678,#52679,#52680,#52681,#52682,#52683,#52684,#52685,
#52686,#52687,#52688,#52689,#52690,#52691,#52692),.UNSPECIFIED.,.F.,.F.)
B_SPLINE_CURVE_WITH_KNOTS((6,1,1,1,1,1,1,1,1,1,1,1,1,1,1,1,1,1,1,1,1,6),
(0.428061295609925,0.428571428571429,0.457142857142857,0.485714285714286,
0.514285714285714,0.542857142857143,0.571428571428572,0.6,0.628571428571429,
0.657142857142857,0.685714285714286,0.714285714285714,0.742857142857143,
0.771428571428572,0.8,0.828571428571429,0.857142857142857,0.885714285714286,
0.914285714285714,0.942857142857143,0.971428571428572,1.),.UNSPECIFIED.)
CURVE()
GEOMETRIC_REPRESENTATION_ITEM()
RATIONAL_B_SPLINE_CURVE((1.,1.,1.,1.,1.,1.,1.,1.,1.,1.,1.,1.,1.,1.,1.,1.,
1.,1.,1.,1.,1.,1.,1.,1.,1.,1.))
REPRESENTATION_ITEM('')
);
#772=(
BOUNDED_CURVE()
B_SPLINE_CURVE(5,(#52696,#52697,#52698,#52699,#52700,#52701,#52702,#52703,
#52704,#52705,#52706,#52707,#52708,#52709,#52710,#52711,#52712,#52713,#52714,
#52715,#52716,#52717,#52718,#52719,#52720,#52721,#52722,#52723,#52724),
 .UNSPECIFIED.,.F.,.F.)
B_SPLINE_CURVE_WITH_KNOTS((6,1,1,1,1,1,1,1,1,1,1,1,1,1,1,1,1,1,1,1,1,1,
1,1,6),(0.,0.0285714285714286,0.0571428571428571,0.0857142857142857,0.114285714285714,
0.142857142857143,0.171428571428571,0.2,0.228571428571429,0.257142857142857,
0.285714285714286,0.314285714285714,0.342857142857143,0.371428571428571,
0.4,0.428571428571429,0.457142857142857,0.485714285714286,0.514285714285714,
0.542857142857143,0.571428571428572,0.6,0.628571428571429,0.657142857142857,
0.670627588953112),.UNSPECIFIED.)
CURVE()
GEOMETRIC_REPRESENTATION_ITEM()
RATIONAL_B_SPLINE_CURVE((1.,1.,1.,1.,1.,1.,1.,1.,1.,1.,1.,1.,1.,1.,1.,1.,
1.,1.,1.,1.,1.,1.,1.,1.,1.,1.,1.,1.,1.))
REPRESENTATION_ITEM('')
);
#773=(
BOUNDED_CURVE()
B_SPLINE_CURVE(5,(#52728,#52729,#52730,#52731,#52732,#52733,#52734,#52735,
#52736,#52737,#52738,#52739,#52740,#52741,#52742,#52743,#52744,#52745,#52746,
#52747,#52748,#52749,#52750,#52751,#52752,#52753),.UNSPECIFIED.,.F.,.F.)
B_SPLINE_CURVE_WITH_KNOTS((6,1,1,1,1,1,1,1,1,1,1,1,1,1,1,1,1,1,1,1,1,6),
(0.428061295609926,0.428571428571429,0.457142857142857,0.485714285714286,
0.514285714285714,0.542857142857143,0.571428571428572,0.6,0.628571428571429,
0.657142857142857,0.685714285714286,0.714285714285714,0.742857142857143,
0.771428571428572,0.8,0.828571428571429,0.857142857142857,0.885714285714286,
0.914285714285714,0.942857142857143,0.971428571428572,1.),.UNSPECIFIED.)
CURVE()
GEOMETRIC_REPRESENTATION_ITEM()
RATIONAL_B_SPLINE_CURVE((1.,1.,1.,1.,1.,1.,1.,1.,1.,1.,1.,1.,1.,1.,1.,1.,
1.,1.,1.,1.,1.,1.,1.,1.,1.,1.))
REPRESENTATION_ITEM('')
);
#774=(
BOUNDED_CURVE()
B_SPLINE_CURVE(5,(#52757,#52758,#52759,#52760,#52761,#52762,#52763,#52764,
#52765,#52766,#52767,#52768,#52769,#52770,#52771,#52772,#52773,#52774,#52775,
#52776,#52777,#52778,#52779,#52780,#52781,#52782,#52783,#52784,#52785),
 .UNSPECIFIED.,.F.,.F.)
B_SPLINE_CURVE_WITH_KNOTS((6,1,1,1,1,1,1,1,1,1,1,1,1,1,1,1,1,1,1,1,1,1,
1,1,6),(0.,0.0285714285714286,0.0571428571428571,0.0857142857142857,0.114285714285714,
0.142857142857143,0.171428571428571,0.2,0.228571428571429,0.257142857142857,
0.285714285714286,0.314285714285714,0.342857142857143,0.371428571428571,
0.4,0.428571428571429,0.457142857142857,0.485714285714286,0.514285714285714,
0.542857142857143,0.571428571428572,0.6,0.628571428571429,0.657142857142857,
0.670627588953112),.UNSPECIFIED.)
CURVE()
GEOMETRIC_REPRESENTATION_ITEM()
RATIONAL_B_SPLINE_CURVE((1.,1.,1.,1.,1.,1.,1.,1.,1.,1.,1.,1.,1.,1.,1.,1.,
1.,1.,1.,1.,1.,1.,1.,1.,1.,1.,1.,1.,1.))
REPRESENTATION_ITEM('')
);
#775=(
BOUNDED_CURVE()
B_SPLINE_CURVE(5,(#52789,#52790,#52791,#52792,#52793,#52794,#52795,#52796,
#52797,#52798,#52799,#52800,#52801,#52802,#52803,#52804,#52805,#52806,#52807,
#52808,#52809,#52810,#52811,#52812,#52813,#52814),.UNSPECIFIED.,.F.,.F.)
B_SPLINE_CURVE_WITH_KNOTS((6,1,1,1,1,1,1,1,1,1,1,1,1,1,1,1,1,1,1,1,1,6),
(0.428061295609925,0.428571428571429,0.457142857142857,0.485714285714286,
0.514285714285714,0.542857142857143,0.571428571428572,0.6,0.628571428571429,
0.657142857142857,0.685714285714286,0.714285714285714,0.742857142857143,
0.771428571428572,0.8,0.828571428571429,0.857142857142857,0.885714285714286,
0.914285714285714,0.942857142857143,0.971428571428572,1.),.UNSPECIFIED.)
CURVE()
GEOMETRIC_REPRESENTATION_ITEM()
RATIONAL_B_SPLINE_CURVE((1.,1.,1.,1.,1.,1.,1.,1.,1.,1.,1.,1.,1.,1.,1.,1.,
1.,1.,1.,1.,1.,1.,1.,1.,1.,1.))
REPRESENTATION_ITEM('')
);
#776=(
BOUNDED_CURVE()
B_SPLINE_CURVE(5,(#52818,#52819,#52820,#52821,#52822,#52823,#52824,#52825,
#52826,#52827,#52828,#52829,#52830,#52831,#52832,#52833,#52834,#52835,#52836,
#52837,#52838,#52839,#52840,#52841,#52842,#52843,#52844,#52845,#52846),
 .UNSPECIFIED.,.F.,.F.)
B_SPLINE_CURVE_WITH_KNOTS((6,1,1,1,1,1,1,1,1,1,1,1,1,1,1,1,1,1,1,1,1,1,
1,1,6),(0.,0.0285714285714286,0.0571428571428571,0.0857142857142857,0.114285714285714,
0.142857142857143,0.171428571428571,0.2,0.228571428571429,0.257142857142857,
0.285714285714286,0.314285714285714,0.342857142857143,0.371428571428571,
0.4,0.428571428571429,0.457142857142857,0.485714285714286,0.514285714285714,
0.542857142857143,0.571428571428572,0.6,0.628571428571429,0.657142857142857,
0.670627588953113),.UNSPECIFIED.)
CURVE()
GEOMETRIC_REPRESENTATION_ITEM()
RATIONAL_B_SPLINE_CURVE((1.,1.,1.,1.,1.,1.,1.,1.,1.,1.,1.,1.,1.,1.,1.,1.,
1.,1.,1.,1.,1.,1.,1.,1.,1.,1.,1.,1.,1.))
REPRESENTATION_ITEM('')
);
#777=(
BOUNDED_CURVE()
B_SPLINE_CURVE(5,(#52850,#52851,#52852,#52853,#52854,#52855,#52856,#52857,
#52858,#52859,#52860,#52861,#52862,#52863,#52864,#52865,#52866,#52867,#52868,
#52869,#52870,#52871,#52872,#52873,#52874,#52875),.UNSPECIFIED.,.F.,.F.)
B_SPLINE_CURVE_WITH_KNOTS((6,1,1,1,1,1,1,1,1,1,1,1,1,1,1,1,1,1,1,1,1,6),
(0.428061295609925,0.428571428571429,0.457142857142857,0.485714285714286,
0.514285714285714,0.542857142857143,0.571428571428572,0.6,0.628571428571429,
0.657142857142857,0.685714285714286,0.714285714285714,0.742857142857143,
0.771428571428572,0.8,0.828571428571429,0.857142857142857,0.885714285714286,
0.914285714285714,0.942857142857143,0.971428571428572,1.),.UNSPECIFIED.)
CURVE()
GEOMETRIC_REPRESENTATION_ITEM()
RATIONAL_B_SPLINE_CURVE((1.,1.,1.,1.,1.,1.,1.,1.,1.,1.,1.,1.,1.,1.,1.,1.,
1.,1.,1.,1.,1.,1.,1.,1.,1.,1.))
REPRESENTATION_ITEM('')
);
#778=(
BOUNDED_CURVE()
B_SPLINE_CURVE(5,(#52879,#52880,#52881,#52882,#52883,#52884,#52885,#52886,
#52887,#52888,#52889,#52890,#52891,#52892,#52893,#52894,#52895,#52896,#52897,
#52898,#52899,#52900,#52901,#52902,#52903,#52904,#52905,#52906,#52907),
 .UNSPECIFIED.,.F.,.F.)
B_SPLINE_CURVE_WITH_KNOTS((6,1,1,1,1,1,1,1,1,1,1,1,1,1,1,1,1,1,1,1,1,1,
1,1,6),(0.,0.0285714285714286,0.0571428571428571,0.0857142857142857,0.114285714285714,
0.142857142857143,0.171428571428571,0.2,0.228571428571429,0.257142857142857,
0.285714285714286,0.314285714285714,0.342857142857143,0.371428571428571,
0.4,0.428571428571429,0.457142857142857,0.485714285714286,0.514285714285714,
0.542857142857143,0.571428571428572,0.6,0.628571428571429,0.657142857142857,
0.670627588953112),.UNSPECIFIED.)
CURVE()
GEOMETRIC_REPRESENTATION_ITEM()
RATIONAL_B_SPLINE_CURVE((1.,1.,1.,1.,1.,1.,1.,1.,1.,1.,1.,1.,1.,1.,1.,1.,
1.,1.,1.,1.,1.,1.,1.,1.,1.,1.,1.,1.,1.))
REPRESENTATION_ITEM('')
);
#779=(
BOUNDED_CURVE()
B_SPLINE_CURVE(5,(#52911,#52912,#52913,#52914,#52915,#52916,#52917,#52918,
#52919,#52920,#52921,#52922,#52923,#52924,#52925,#52926,#52927,#52928,#52929,
#52930,#52931,#52932,#52933,#52934,#52935,#52936),.UNSPECIFIED.,.F.,.F.)
B_SPLINE_CURVE_WITH_KNOTS((6,1,1,1,1,1,1,1,1,1,1,1,1,1,1,1,1,1,1,1,1,6),
(0.428061295609926,0.428571428571429,0.457142857142857,0.485714285714286,
0.514285714285714,0.542857142857143,0.571428571428572,0.6,0.628571428571429,
0.657142857142857,0.685714285714286,0.714285714285714,0.742857142857143,
0.771428571428572,0.8,0.828571428571429,0.857142857142857,0.885714285714286,
0.914285714285714,0.942857142857143,0.971428571428572,1.),.UNSPECIFIED.)
CURVE()
GEOMETRIC_REPRESENTATION_ITEM()
RATIONAL_B_SPLINE_CURVE((1.,1.,1.,1.,1.,1.,1.,1.,1.,1.,1.,1.,1.,1.,1.,1.,
1.,1.,1.,1.,1.,1.,1.,1.,1.,1.))
REPRESENTATION_ITEM('')
);
#780=(
BOUNDED_CURVE()
B_SPLINE_CURVE(5,(#52940,#52941,#52942,#52943,#52944,#52945,#52946,#52947,
#52948,#52949,#52950,#52951,#52952,#52953,#52954,#52955,#52956,#52957,#52958,
#52959,#52960,#52961,#52962,#52963,#52964,#52965,#52966,#52967,#52968),
 .UNSPECIFIED.,.F.,.F.)
B_SPLINE_CURVE_WITH_KNOTS((6,1,1,1,1,1,1,1,1,1,1,1,1,1,1,1,1,1,1,1,1,1,
1,1,6),(0.,0.0285714285714286,0.0571428571428571,0.0857142857142857,0.114285714285714,
0.142857142857143,0.171428571428571,0.2,0.228571428571429,0.257142857142857,
0.285714285714286,0.314285714285714,0.342857142857143,0.371428571428571,
0.4,0.428571428571429,0.457142857142857,0.485714285714286,0.514285714285714,
0.542857142857143,0.571428571428572,0.6,0.628571428571429,0.657142857142857,
0.670627588953112),.UNSPECIFIED.)
CURVE()
GEOMETRIC_REPRESENTATION_ITEM()
RATIONAL_B_SPLINE_CURVE((1.,1.,1.,1.,1.,1.,1.,1.,1.,1.,1.,1.,1.,1.,1.,1.,
1.,1.,1.,1.,1.,1.,1.,1.,1.,1.,1.,1.,1.))
REPRESENTATION_ITEM('')
);
#781=(
BOUNDED_CURVE()
B_SPLINE_CURVE(5,(#52972,#52973,#52974,#52975,#52976,#52977,#52978,#52979,
#52980,#52981,#52982,#52983,#52984,#52985,#52986,#52987,#52988,#52989,#52990,
#52991,#52992,#52993,#52994,#52995,#52996,#52997),.UNSPECIFIED.,.F.,.F.)
B_SPLINE_CURVE_WITH_KNOTS((6,1,1,1,1,1,1,1,1,1,1,1,1,1,1,1,1,1,1,1,1,6),
(0.428061295609926,0.428571428571429,0.457142857142857,0.485714285714286,
0.514285714285714,0.542857142857143,0.571428571428572,0.6,0.628571428571429,
0.657142857142857,0.685714285714286,0.714285714285714,0.742857142857143,
0.771428571428572,0.8,0.828571428571429,0.857142857142857,0.885714285714286,
0.914285714285714,0.942857142857143,0.971428571428572,1.),.UNSPECIFIED.)
CURVE()
GEOMETRIC_REPRESENTATION_ITEM()
RATIONAL_B_SPLINE_CURVE((1.,1.,1.,1.,1.,1.,1.,1.,1.,1.,1.,1.,1.,1.,1.,1.,
1.,1.,1.,1.,1.,1.,1.,1.,1.,1.))
REPRESENTATION_ITEM('')
);
#782=(
BOUNDED_CURVE()
B_SPLINE_CURVE(5,(#53001,#53002,#53003,#53004,#53005,#53006,#53007,#53008,
#53009,#53010,#53011,#53012,#53013,#53014,#53015,#53016,#53017,#53018,#53019,
#53020,#53021,#53022,#53023,#53024,#53025,#53026,#53027,#53028,#53029),
 .UNSPECIFIED.,.F.,.F.)
B_SPLINE_CURVE_WITH_KNOTS((6,1,1,1,1,1,1,1,1,1,1,1,1,1,1,1,1,1,1,1,1,1,
1,1,6),(0.,0.0285714285714286,0.0571428571428571,0.0857142857142857,0.114285714285714,
0.142857142857143,0.171428571428571,0.2,0.228571428571429,0.257142857142857,
0.285714285714286,0.314285714285714,0.342857142857143,0.371428571428571,
0.4,0.428571428571429,0.457142857142857,0.485714285714286,0.514285714285714,
0.542857142857143,0.571428571428572,0.6,0.628571428571429,0.657142857142857,
0.670627588953112),.UNSPECIFIED.)
CURVE()
GEOMETRIC_REPRESENTATION_ITEM()
RATIONAL_B_SPLINE_CURVE((1.,1.,1.,1.,1.,1.,1.,1.,1.,1.,1.,1.,1.,1.,1.,1.,
1.,1.,1.,1.,1.,1.,1.,1.,1.,1.,1.,1.,1.))
REPRESENTATION_ITEM('')
);
#783=(
BOUNDED_CURVE()
B_SPLINE_CURVE(5,(#53033,#53034,#53035,#53036,#53037,#53038,#53039,#53040,
#53041,#53042,#53043,#53044,#53045,#53046,#53047,#53048,#53049,#53050,#53051,
#53052,#53053,#53054,#53055,#53056,#53057,#53058),.UNSPECIFIED.,.F.,.F.)
B_SPLINE_CURVE_WITH_KNOTS((6,1,1,1,1,1,1,1,1,1,1,1,1,1,1,1,1,1,1,1,1,6),
(0.428061295609926,0.428571428571429,0.457142857142857,0.485714285714286,
0.514285714285714,0.542857142857143,0.571428571428572,0.6,0.628571428571429,
0.657142857142857,0.685714285714286,0.714285714285714,0.742857142857143,
0.771428571428572,0.8,0.828571428571429,0.857142857142857,0.885714285714286,
0.914285714285714,0.942857142857143,0.971428571428572,1.),.UNSPECIFIED.)
CURVE()
GEOMETRIC_REPRESENTATION_ITEM()
RATIONAL_B_SPLINE_CURVE((1.,1.,1.,1.,1.,1.,1.,1.,1.,1.,1.,1.,1.,1.,1.,1.,
1.,1.,1.,1.,1.,1.,1.,1.,1.,1.))
REPRESENTATION_ITEM('')
);
#784=(
BOUNDED_CURVE()
B_SPLINE_CURVE(5,(#53062,#53063,#53064,#53065,#53066,#53067,#53068,#53069,
#53070,#53071,#53072,#53073,#53074,#53075,#53076,#53077,#53078,#53079,#53080,
#53081,#53082,#53083,#53084,#53085,#53086,#53087,#53088,#53089,#53090),
 .UNSPECIFIED.,.F.,.F.)
B_SPLINE_CURVE_WITH_KNOTS((6,1,1,1,1,1,1,1,1,1,1,1,1,1,1,1,1,1,1,1,1,1,
1,1,6),(0.,0.0285714285714286,0.0571428571428571,0.0857142857142857,0.114285714285714,
0.142857142857143,0.171428571428571,0.2,0.228571428571429,0.257142857142857,
0.285714285714286,0.314285714285714,0.342857142857143,0.371428571428571,
0.4,0.428571428571429,0.457142857142857,0.485714285714286,0.514285714285714,
0.542857142857143,0.571428571428572,0.6,0.628571428571429,0.657142857142857,
0.670627588953113),.UNSPECIFIED.)
CURVE()
GEOMETRIC_REPRESENTATION_ITEM()
RATIONAL_B_SPLINE_CURVE((1.,1.,1.,1.,1.,1.,1.,1.,1.,1.,1.,1.,1.,1.,1.,1.,
1.,1.,1.,1.,1.,1.,1.,1.,1.,1.,1.,1.,1.))
REPRESENTATION_ITEM('')
);
#785=(
BOUNDED_CURVE()
B_SPLINE_CURVE(5,(#53094,#53095,#53096,#53097,#53098,#53099,#53100,#53101,
#53102,#53103,#53104,#53105,#53106,#53107,#53108,#53109,#53110,#53111,#53112,
#53113,#53114,#53115,#53116,#53117,#53118,#53119),.UNSPECIFIED.,.F.,.F.)
B_SPLINE_CURVE_WITH_KNOTS((6,1,1,1,1,1,1,1,1,1,1,1,1,1,1,1,1,1,1,1,1,6),
(0.428061295609926,0.428571428571429,0.457142857142857,0.485714285714286,
0.514285714285714,0.542857142857143,0.571428571428572,0.6,0.628571428571429,
0.657142857142857,0.685714285714286,0.714285714285714,0.742857142857143,
0.771428571428572,0.8,0.828571428571429,0.857142857142857,0.885714285714286,
0.914285714285714,0.942857142857143,0.971428571428572,1.),.UNSPECIFIED.)
CURVE()
GEOMETRIC_REPRESENTATION_ITEM()
RATIONAL_B_SPLINE_CURVE((1.,1.,1.,1.,1.,1.,1.,1.,1.,1.,1.,1.,1.,1.,1.,1.,
1.,1.,1.,1.,1.,1.,1.,1.,1.,1.))
REPRESENTATION_ITEM('')
);
#786=(
BOUNDED_CURVE()
B_SPLINE_CURVE(5,(#53123,#53124,#53125,#53126,#53127,#53128,#53129,#53130,
#53131,#53132,#53133,#53134,#53135,#53136,#53137,#53138,#53139,#53140,#53141,
#53142,#53143,#53144,#53145,#53146,#53147,#53148,#53149,#53150,#53151),
 .UNSPECIFIED.,.F.,.F.)
B_SPLINE_CURVE_WITH_KNOTS((6,1,1,1,1,1,1,1,1,1,1,1,1,1,1,1,1,1,1,1,1,1,
1,1,6),(0.,0.0285714285714286,0.0571428571428571,0.0857142857142857,0.114285714285714,
0.142857142857143,0.171428571428571,0.2,0.228571428571429,0.257142857142857,
0.285714285714286,0.314285714285714,0.342857142857143,0.371428571428571,
0.4,0.428571428571429,0.457142857142857,0.485714285714286,0.514285714285714,
0.542857142857143,0.571428571428572,0.6,0.628571428571429,0.657142857142857,
0.670627588953111),.UNSPECIFIED.)
CURVE()
GEOMETRIC_REPRESENTATION_ITEM()
RATIONAL_B_SPLINE_CURVE((1.,1.,1.,1.,1.,1.,1.,1.,1.,1.,1.,1.,1.,1.,1.,1.,
1.,1.,1.,1.,1.,1.,1.,1.,1.,1.,1.,1.,1.))
REPRESENTATION_ITEM('')
);
#787=(
BOUNDED_CURVE()
B_SPLINE_CURVE(5,(#53155,#53156,#53157,#53158,#53159,#53160,#53161,#53162,
#53163,#53164,#53165,#53166,#53167,#53168,#53169,#53170,#53171,#53172,#53173,
#53174,#53175,#53176,#53177,#53178,#53179,#53180),.UNSPECIFIED.,.F.,.F.)
B_SPLINE_CURVE_WITH_KNOTS((6,1,1,1,1,1,1,1,1,1,1,1,1,1,1,1,1,1,1,1,1,6),
(0.428061295609925,0.428571428571429,0.457142857142857,0.485714285714286,
0.514285714285714,0.542857142857143,0.571428571428572,0.6,0.628571428571429,
0.657142857142857,0.685714285714286,0.714285714285714,0.742857142857143,
0.771428571428572,0.8,0.828571428571429,0.857142857142857,0.885714285714286,
0.914285714285714,0.942857142857143,0.971428571428572,1.),.UNSPECIFIED.)
CURVE()
GEOMETRIC_REPRESENTATION_ITEM()
RATIONAL_B_SPLINE_CURVE((1.,1.,1.,1.,1.,1.,1.,1.,1.,1.,1.,1.,1.,1.,1.,1.,
1.,1.,1.,1.,1.,1.,1.,1.,1.,1.))
REPRESENTATION_ITEM('')
);
#788=(
BOUNDED_CURVE()
B_SPLINE_CURVE(5,(#53184,#53185,#53186,#53187,#53188,#53189,#53190,#53191,
#53192,#53193,#53194,#53195,#53196,#53197,#53198,#53199,#53200,#53201,#53202,
#53203,#53204,#53205,#53206,#53207,#53208,#53209,#53210,#53211,#53212),
 .UNSPECIFIED.,.F.,.F.)
B_SPLINE_CURVE_WITH_KNOTS((6,1,1,1,1,1,1,1,1,1,1,1,1,1,1,1,1,1,1,1,1,1,
1,1,6),(0.,0.0285714285714286,0.0571428571428571,0.0857142857142857,0.114285714285714,
0.142857142857143,0.171428571428571,0.2,0.228571428571429,0.257142857142857,
0.285714285714286,0.314285714285714,0.342857142857143,0.371428571428571,
0.4,0.428571428571429,0.457142857142857,0.485714285714286,0.514285714285714,
0.542857142857143,0.571428571428572,0.6,0.628571428571429,0.657142857142857,
0.670627588953113),.UNSPECIFIED.)
CURVE()
GEOMETRIC_REPRESENTATION_ITEM()
RATIONAL_B_SPLINE_CURVE((1.,1.,1.,1.,1.,1.,1.,1.,1.,1.,1.,1.,1.,1.,1.,1.,
1.,1.,1.,1.,1.,1.,1.,1.,1.,1.,1.,1.,1.))
REPRESENTATION_ITEM('')
);
#789=(
BOUNDED_CURVE()
B_SPLINE_CURVE(5,(#53216,#53217,#53218,#53219,#53220,#53221,#53222,#53223,
#53224,#53225,#53226,#53227,#53228,#53229,#53230,#53231,#53232,#53233,#53234,
#53235,#53236,#53237,#53238,#53239,#53240,#53241),.UNSPECIFIED.,.F.,.F.)
B_SPLINE_CURVE_WITH_KNOTS((6,1,1,1,1,1,1,1,1,1,1,1,1,1,1,1,1,1,1,1,1,6),
(0.428061295609926,0.428571428571429,0.457142857142857,0.485714285714286,
0.514285714285714,0.542857142857143,0.571428571428572,0.6,0.628571428571429,
0.657142857142857,0.685714285714286,0.714285714285714,0.742857142857143,
0.771428571428572,0.8,0.828571428571429,0.857142857142857,0.885714285714286,
0.914285714285714,0.942857142857143,0.971428571428572,1.),.UNSPECIFIED.)
CURVE()
GEOMETRIC_REPRESENTATION_ITEM()
RATIONAL_B_SPLINE_CURVE((1.,1.,1.,1.,1.,1.,1.,1.,1.,1.,1.,1.,1.,1.,1.,1.,
1.,1.,1.,1.,1.,1.,1.,1.,1.,1.))
REPRESENTATION_ITEM('')
);
#790=(
BOUNDED_CURVE()
B_SPLINE_CURVE(5,(#53245,#53246,#53247,#53248,#53249,#53250,#53251,#53252,
#53253,#53254,#53255,#53256,#53257,#53258,#53259,#53260,#53261,#53262,#53263,
#53264,#53265,#53266,#53267,#53268,#53269,#53270,#53271,#53272,#53273),
 .UNSPECIFIED.,.F.,.F.)
B_SPLINE_CURVE_WITH_KNOTS((6,1,1,1,1,1,1,1,1,1,1,1,1,1,1,1,1,1,1,1,1,1,
1,1,6),(0.,0.0285714285714286,0.0571428571428571,0.0857142857142857,0.114285714285714,
0.142857142857143,0.171428571428571,0.2,0.228571428571429,0.257142857142857,
0.285714285714286,0.314285714285714,0.342857142857143,0.371428571428571,
0.4,0.428571428571429,0.457142857142857,0.485714285714286,0.514285714285714,
0.542857142857143,0.571428571428572,0.6,0.628571428571429,0.657142857142857,
0.670627588953113),.UNSPECIFIED.)
CURVE()
GEOMETRIC_REPRESENTATION_ITEM()
RATIONAL_B_SPLINE_CURVE((1.,1.,1.,1.,1.,1.,1.,1.,1.,1.,1.,1.,1.,1.,1.,1.,
1.,1.,1.,1.,1.,1.,1.,1.,1.,1.,1.,1.,1.))
REPRESENTATION_ITEM('')
);
#791=(
BOUNDED_CURVE()
B_SPLINE_CURVE(5,(#53277,#53278,#53279,#53280,#53281,#53282,#53283,#53284,
#53285,#53286,#53287,#53288,#53289,#53290,#53291,#53292,#53293,#53294,#53295,
#53296,#53297,#53298,#53299,#53300,#53301,#53302),.UNSPECIFIED.,.F.,.F.)
B_SPLINE_CURVE_WITH_KNOTS((6,1,1,1,1,1,1,1,1,1,1,1,1,1,1,1,1,1,1,1,1,6),
(0.428061295609925,0.428571428571429,0.457142857142857,0.485714285714286,
0.514285714285714,0.542857142857143,0.571428571428572,0.6,0.628571428571429,
0.657142857142857,0.685714285714286,0.714285714285714,0.742857142857143,
0.771428571428572,0.8,0.828571428571429,0.857142857142857,0.885714285714286,
0.914285714285714,0.942857142857143,0.971428571428572,1.),.UNSPECIFIED.)
CURVE()
GEOMETRIC_REPRESENTATION_ITEM()
RATIONAL_B_SPLINE_CURVE((1.,1.,1.,1.,1.,1.,1.,1.,1.,1.,1.,1.,1.,1.,1.,1.,
1.,1.,1.,1.,1.,1.,1.,1.,1.,1.))
REPRESENTATION_ITEM('')
);
#792=(
BOUNDED_CURVE()
B_SPLINE_CURVE(5,(#53306,#53307,#53308,#53309,#53310,#53311,#53312,#53313,
#53314,#53315,#53316,#53317,#53318,#53319,#53320,#53321,#53322,#53323,#53324,
#53325,#53326,#53327,#53328,#53329,#53330,#53331,#53332,#53333,#53334),
 .UNSPECIFIED.,.F.,.F.)
B_SPLINE_CURVE_WITH_KNOTS((6,1,1,1,1,1,1,1,1,1,1,1,1,1,1,1,1,1,1,1,1,1,
1,1,6),(0.,0.0285714285714286,0.0571428571428571,0.0857142857142857,0.114285714285714,
0.142857142857143,0.171428571428571,0.2,0.228571428571429,0.257142857142857,
0.285714285714286,0.314285714285714,0.342857142857143,0.371428571428571,
0.4,0.428571428571429,0.457142857142857,0.485714285714286,0.514285714285714,
0.542857142857143,0.571428571428572,0.6,0.628571428571429,0.657142857142857,
0.670627588953112),.UNSPECIFIED.)
CURVE()
GEOMETRIC_REPRESENTATION_ITEM()
RATIONAL_B_SPLINE_CURVE((1.,1.,1.,1.,1.,1.,1.,1.,1.,1.,1.,1.,1.,1.,1.,1.,
1.,1.,1.,1.,1.,1.,1.,1.,1.,1.,1.,1.,1.))
REPRESENTATION_ITEM('')
);
#793=(
BOUNDED_CURVE()
B_SPLINE_CURVE(5,(#53338,#53339,#53340,#53341,#53342,#53343,#53344,#53345,
#53346,#53347,#53348,#53349,#53350,#53351,#53352,#53353,#53354,#53355,#53356,
#53357,#53358,#53359,#53360,#53361,#53362,#53363),.UNSPECIFIED.,.F.,.F.)
B_SPLINE_CURVE_WITH_KNOTS((6,1,1,1,1,1,1,1,1,1,1,1,1,1,1,1,1,1,1,1,1,6),
(0.428061295609925,0.428571428571429,0.457142857142857,0.485714285714286,
0.514285714285714,0.542857142857143,0.571428571428572,0.6,0.628571428571429,
0.657142857142857,0.685714285714286,0.714285714285714,0.742857142857143,
0.771428571428572,0.8,0.828571428571429,0.857142857142857,0.885714285714286,
0.914285714285714,0.942857142857143,0.971428571428572,1.),.UNSPECIFIED.)
CURVE()
GEOMETRIC_REPRESENTATION_ITEM()
RATIONAL_B_SPLINE_CURVE((1.,1.,1.,1.,1.,1.,1.,1.,1.,1.,1.,1.,1.,1.,1.,1.,
1.,1.,1.,1.,1.,1.,1.,1.,1.,1.))
REPRESENTATION_ITEM('')
);
#794=(
BOUNDED_CURVE()
B_SPLINE_CURVE(5,(#53367,#53368,#53369,#53370,#53371,#53372,#53373,#53374,
#53375,#53376,#53377,#53378,#53379,#53380,#53381,#53382,#53383,#53384,#53385,
#53386,#53387,#53388,#53389,#53390,#53391,#53392,#53393,#53394,#53395),
 .UNSPECIFIED.,.F.,.F.)
B_SPLINE_CURVE_WITH_KNOTS((6,1,1,1,1,1,1,1,1,1,1,1,1,1,1,1,1,1,1,1,1,1,
1,1,6),(0.,0.0285714285714286,0.0571428571428571,0.0857142857142857,0.114285714285714,
0.142857142857143,0.171428571428571,0.2,0.228571428571429,0.257142857142857,
0.285714285714286,0.314285714285714,0.342857142857143,0.371428571428571,
0.4,0.428571428571429,0.457142857142857,0.485714285714286,0.514285714285714,
0.542857142857143,0.571428571428572,0.6,0.628571428571429,0.657142857142857,
0.670627588953112),.UNSPECIFIED.)
CURVE()
GEOMETRIC_REPRESENTATION_ITEM()
RATIONAL_B_SPLINE_CURVE((1.,1.,1.,1.,1.,1.,1.,1.,1.,1.,1.,1.,1.,1.,1.,1.,
1.,1.,1.,1.,1.,1.,1.,1.,1.,1.,1.,1.,1.))
REPRESENTATION_ITEM('')
);
#795=(
BOUNDED_CURVE()
B_SPLINE_CURVE(5,(#53399,#53400,#53401,#53402,#53403,#53404,#53405,#53406,
#53407,#53408,#53409,#53410,#53411,#53412,#53413,#53414,#53415,#53416,#53417,
#53418,#53419,#53420,#53421,#53422,#53423,#53424),.UNSPECIFIED.,.F.,.F.)
B_SPLINE_CURVE_WITH_KNOTS((6,1,1,1,1,1,1,1,1,1,1,1,1,1,1,1,1,1,1,1,1,6),
(0.428061295609926,0.428571428571429,0.457142857142857,0.485714285714286,
0.514285714285714,0.542857142857143,0.571428571428572,0.6,0.628571428571429,
0.657142857142857,0.685714285714286,0.714285714285714,0.742857142857143,
0.771428571428572,0.8,0.828571428571429,0.857142857142857,0.885714285714286,
0.914285714285714,0.942857142857143,0.971428571428572,1.),.UNSPECIFIED.)
CURVE()
GEOMETRIC_REPRESENTATION_ITEM()
RATIONAL_B_SPLINE_CURVE((1.,1.,1.,1.,1.,1.,1.,1.,1.,1.,1.,1.,1.,1.,1.,1.,
1.,1.,1.,1.,1.,1.,1.,1.,1.,1.))
REPRESENTATION_ITEM('')
);
#796=(
BOUNDED_CURVE()
B_SPLINE_CURVE(5,(#53428,#53429,#53430,#53431,#53432,#53433,#53434,#53435,
#53436,#53437,#53438,#53439,#53440,#53441,#53442,#53443,#53444,#53445,#53446,
#53447,#53448,#53449,#53450,#53451,#53452,#53453,#53454,#53455,#53456),
 .UNSPECIFIED.,.F.,.F.)
B_SPLINE_CURVE_WITH_KNOTS((6,1,1,1,1,1,1,1,1,1,1,1,1,1,1,1,1,1,1,1,1,1,
1,1,6),(0.,0.0285714285714286,0.0571428571428571,0.0857142857142857,0.114285714285714,
0.142857142857143,0.171428571428571,0.2,0.228571428571429,0.257142857142857,
0.285714285714286,0.314285714285714,0.342857142857143,0.371428571428571,
0.4,0.428571428571429,0.457142857142857,0.485714285714286,0.514285714285714,
0.542857142857143,0.571428571428572,0.6,0.628571428571429,0.657142857142857,
0.670627588953112),.UNSPECIFIED.)
CURVE()
GEOMETRIC_REPRESENTATION_ITEM()
RATIONAL_B_SPLINE_CURVE((1.,1.,1.,1.,1.,1.,1.,1.,1.,1.,1.,1.,1.,1.,1.,1.,
1.,1.,1.,1.,1.,1.,1.,1.,1.,1.,1.,1.,1.))
REPRESENTATION_ITEM('')
);
#797=(
BOUNDED_CURVE()
B_SPLINE_CURVE(5,(#53460,#53461,#53462,#53463,#53464,#53465,#53466,#53467,
#53468,#53469,#53470,#53471,#53472,#53473,#53474,#53475,#53476,#53477,#53478,
#53479,#53480,#53481,#53482,#53483,#53484,#53485),.UNSPECIFIED.,.F.,.F.)
B_SPLINE_CURVE_WITH_KNOTS((6,1,1,1,1,1,1,1,1,1,1,1,1,1,1,1,1,1,1,1,1,6),
(0.428061295609926,0.428571428571429,0.457142857142857,0.485714285714286,
0.514285714285714,0.542857142857143,0.571428571428572,0.6,0.628571428571429,
0.657142857142857,0.685714285714286,0.714285714285714,0.742857142857143,
0.771428571428572,0.8,0.828571428571429,0.857142857142857,0.885714285714286,
0.914285714285714,0.942857142857143,0.971428571428572,1.),.UNSPECIFIED.)
CURVE()
GEOMETRIC_REPRESENTATION_ITEM()
RATIONAL_B_SPLINE_CURVE((1.,1.,1.,1.,1.,1.,1.,1.,1.,1.,1.,1.,1.,1.,1.,1.,
1.,1.,1.,1.,1.,1.,1.,1.,1.,1.))
REPRESENTATION_ITEM('')
);
#798=(
BOUNDED_CURVE()
B_SPLINE_CURVE(5,(#53489,#53490,#53491,#53492,#53493,#53494,#53495,#53496,
#53497,#53498,#53499,#53500,#53501,#53502,#53503,#53504,#53505,#53506,#53507,
#53508,#53509,#53510,#53511,#53512,#53513,#53514,#53515,#53516,#53517),
 .UNSPECIFIED.,.F.,.F.)
B_SPLINE_CURVE_WITH_KNOTS((6,1,1,1,1,1,1,1,1,1,1,1,1,1,1,1,1,1,1,1,1,1,
1,1,6),(0.,0.0285714285714286,0.0571428571428571,0.0857142857142857,0.114285714285714,
0.142857142857143,0.171428571428571,0.2,0.228571428571429,0.257142857142857,
0.285714285714286,0.314285714285714,0.342857142857143,0.371428571428571,
0.4,0.428571428571429,0.457142857142857,0.485714285714286,0.514285714285714,
0.542857142857143,0.571428571428572,0.6,0.628571428571429,0.657142857142857,
0.670627588953113),.UNSPECIFIED.)
CURVE()
GEOMETRIC_REPRESENTATION_ITEM()
RATIONAL_B_SPLINE_CURVE((1.,1.,1.,1.,1.,1.,1.,1.,1.,1.,1.,1.,1.,1.,1.,1.,
1.,1.,1.,1.,1.,1.,1.,1.,1.,1.,1.,1.,1.))
REPRESENTATION_ITEM('')
);
#799=(
BOUNDED_CURVE()
B_SPLINE_CURVE(5,(#53521,#53522,#53523,#53524,#53525,#53526,#53527,#53528,
#53529,#53530,#53531,#53532,#53533,#53534,#53535,#53536,#53537,#53538,#53539,
#53540,#53541,#53542,#53543,#53544,#53545,#53546),.UNSPECIFIED.,.F.,.F.)
B_SPLINE_CURVE_WITH_KNOTS((6,1,1,1,1,1,1,1,1,1,1,1,1,1,1,1,1,1,1,1,1,6),
(0.428061295609925,0.428571428571429,0.457142857142857,0.485714285714286,
0.514285714285714,0.542857142857143,0.571428571428572,0.6,0.628571428571429,
0.657142857142857,0.685714285714286,0.714285714285714,0.742857142857143,
0.771428571428572,0.8,0.828571428571429,0.857142857142857,0.885714285714286,
0.914285714285714,0.942857142857143,0.971428571428572,1.),.UNSPECIFIED.)
CURVE()
GEOMETRIC_REPRESENTATION_ITEM()
RATIONAL_B_SPLINE_CURVE((1.,1.,1.,1.,1.,1.,1.,1.,1.,1.,1.,1.,1.,1.,1.,1.,
1.,1.,1.,1.,1.,1.,1.,1.,1.,1.))
REPRESENTATION_ITEM('')
);
#800=(
BOUNDED_CURVE()
B_SPLINE_CURVE(5,(#53550,#53551,#53552,#53553,#53554,#53555,#53556,#53557,
#53558,#53559,#53560,#53561,#53562,#53563,#53564,#53565,#53566,#53567,#53568,
#53569,#53570,#53571,#53572,#53573,#53574,#53575,#53576,#53577,#53578),
 .UNSPECIFIED.,.F.,.F.)
B_SPLINE_CURVE_WITH_KNOTS((6,1,1,1,1,1,1,1,1,1,1,1,1,1,1,1,1,1,1,1,1,1,
1,1,6),(0.,0.0285714285714286,0.0571428571428571,0.0857142857142857,0.114285714285714,
0.142857142857143,0.171428571428571,0.2,0.228571428571429,0.257142857142857,
0.285714285714286,0.314285714285714,0.342857142857143,0.371428571428571,
0.4,0.428571428571429,0.457142857142857,0.485714285714286,0.514285714285714,
0.542857142857143,0.571428571428572,0.6,0.628571428571429,0.657142857142857,
0.670627588953112),.UNSPECIFIED.)
CURVE()
GEOMETRIC_REPRESENTATION_ITEM()
RATIONAL_B_SPLINE_CURVE((1.,1.,1.,1.,1.,1.,1.,1.,1.,1.,1.,1.,1.,1.,1.,1.,
1.,1.,1.,1.,1.,1.,1.,1.,1.,1.,1.,1.,1.))
REPRESENTATION_ITEM('')
);
#801=(
BOUNDED_CURVE()
B_SPLINE_CURVE(5,(#53582,#53583,#53584,#53585,#53586,#53587,#53588,#53589,
#53590,#53591,#53592,#53593,#53594,#53595,#53596,#53597,#53598,#53599,#53600,
#53601,#53602,#53603,#53604,#53605,#53606,#53607),.UNSPECIFIED.,.F.,.F.)
B_SPLINE_CURVE_WITH_KNOTS((6,1,1,1,1,1,1,1,1,1,1,1,1,1,1,1,1,1,1,1,1,6),
(0.428061295609926,0.428571428571429,0.457142857142857,0.485714285714286,
0.514285714285714,0.542857142857143,0.571428571428572,0.6,0.628571428571429,
0.657142857142857,0.685714285714286,0.714285714285714,0.742857142857143,
0.771428571428572,0.8,0.828571428571429,0.857142857142857,0.885714285714286,
0.914285714285714,0.942857142857143,0.971428571428572,1.),.UNSPECIFIED.)
CURVE()
GEOMETRIC_REPRESENTATION_ITEM()
RATIONAL_B_SPLINE_CURVE((1.,1.,1.,1.,1.,1.,1.,1.,1.,1.,1.,1.,1.,1.,1.,1.,
1.,1.,1.,1.,1.,1.,1.,1.,1.,1.))
REPRESENTATION_ITEM('')
);
#802=(
BOUNDED_CURVE()
B_SPLINE_CURVE(5,(#53611,#53612,#53613,#53614,#53615,#53616,#53617,#53618,
#53619,#53620,#53621,#53622,#53623,#53624,#53625,#53626,#53627,#53628,#53629,
#53630,#53631,#53632,#53633,#53634,#53635,#53636,#53637,#53638,#53639),
 .UNSPECIFIED.,.F.,.F.)
B_SPLINE_CURVE_WITH_KNOTS((6,1,1,1,1,1,1,1,1,1,1,1,1,1,1,1,1,1,1,1,1,1,
1,1,6),(0.,0.0285714285714286,0.0571428571428571,0.0857142857142857,0.114285714285714,
0.142857142857143,0.171428571428571,0.2,0.228571428571429,0.257142857142857,
0.285714285714286,0.314285714285714,0.342857142857143,0.371428571428571,
0.4,0.428571428571429,0.457142857142857,0.485714285714286,0.514285714285714,
0.542857142857143,0.571428571428572,0.6,0.628571428571429,0.657142857142857,
0.670627588953112),.UNSPECIFIED.)
CURVE()
GEOMETRIC_REPRESENTATION_ITEM()
RATIONAL_B_SPLINE_CURVE((1.,1.,1.,1.,1.,1.,1.,1.,1.,1.,1.,1.,1.,1.,1.,1.,
1.,1.,1.,1.,1.,1.,1.,1.,1.,1.,1.,1.,1.))
REPRESENTATION_ITEM('')
);
#803=(
BOUNDED_CURVE()
B_SPLINE_CURVE(5,(#53643,#53644,#53645,#53646,#53647,#53648,#53649,#53650,
#53651,#53652,#53653,#53654,#53655,#53656,#53657,#53658,#53659,#53660,#53661,
#53662,#53663,#53664,#53665,#53666,#53667,#53668),.UNSPECIFIED.,.F.,.F.)
B_SPLINE_CURVE_WITH_KNOTS((6,1,1,1,1,1,1,1,1,1,1,1,1,1,1,1,1,1,1,1,1,6),
(0.428061295609926,0.428571428571429,0.457142857142857,0.485714285714286,
0.514285714285714,0.542857142857143,0.571428571428572,0.6,0.628571428571429,
0.657142857142857,0.685714285714286,0.714285714285714,0.742857142857143,
0.771428571428572,0.8,0.828571428571429,0.857142857142857,0.885714285714286,
0.914285714285714,0.942857142857143,0.971428571428572,1.),.UNSPECIFIED.)
CURVE()
GEOMETRIC_REPRESENTATION_ITEM()
RATIONAL_B_SPLINE_CURVE((1.,1.,1.,1.,1.,1.,1.,1.,1.,1.,1.,1.,1.,1.,1.,1.,
1.,1.,1.,1.,1.,1.,1.,1.,1.,1.))
REPRESENTATION_ITEM('')
);
#804=(
BOUNDED_CURVE()
B_SPLINE_CURVE(5,(#53674,#53675,#53676,#53677,#53678,#53679,#53680,#53681,
#53682,#53683,#53684,#53685,#53686,#53687,#53688,#53689,#53690,#53691,#53692,
#53693,#53694,#53695,#53696,#53697,#53698,#53699,#53700,#53701,#53702,#53703,
#53704,#53705,#53706,#53707),.UNSPECIFIED.,.F.,.F.)
B_SPLINE_CURVE_WITH_KNOTS((6,1,1,1,1,1,1,1,1,1,1,1,1,1,1,1,1,1,1,1,1,1,
1,1,1,1,1,1,1,6),(0.,0.0285714285714286,0.0571428571428571,0.0857142857142857,
0.114285714285714,0.142857142857143,0.171428571428571,0.2,0.228571428571429,
0.257142857142857,0.285714285714286,0.314285714285714,0.342857142857143,
0.371428571428571,0.4,0.428571428571429,0.457142857142857,0.485714285714286,
0.514285714285714,0.542857142857143,0.571428571428572,0.6,0.628571428571429,
0.657142857142857,0.685714285714286,0.714285714285714,0.742857142857143,
0.771428571428572,0.8,0.816564825616131),.UNSPECIFIED.)
CURVE()
GEOMETRIC_REPRESENTATION_ITEM()
RATIONAL_B_SPLINE_CURVE((1.,1.,1.,1.,1.,1.,1.,1.,1.,1.,1.,1.,1.,1.,1.,1.,
1.,1.,1.,1.,1.,1.,1.,1.,1.,1.,1.,1.,1.,1.,1.,1.,1.,1.))
REPRESENTATION_ITEM('')
);
#805=(
BOUNDED_CURVE()
B_SPLINE_CURVE(5,(#53711,#53712,#53713,#53714,#53715,#53716,#53717,#53718,
#53719,#53720,#53721,#53722,#53723,#53724,#53725,#53726,#53727,#53728,#53729,
#53730,#53731,#53732,#53733,#53734,#53735,#53736,#53737,#53738,#53739),
 .UNSPECIFIED.,.F.,.F.)
B_SPLINE_CURVE_WITH_KNOTS((6,1,1,1,1,1,1,1,1,1,1,1,1,1,1,1,1,1,1,1,1,1,
1,1,6),(0.315728291775709,0.342857142857143,0.371428571428571,0.4,0.428571428571429,
0.457142857142857,0.485714285714286,0.514285714285714,0.542857142857143,
0.571428571428572,0.6,0.628571428571429,0.657142857142857,0.685714285714286,
0.714285714285714,0.742857142857143,0.771428571428572,0.8,0.828571428571429,
0.857142857142857,0.885714285714286,0.914285714285714,0.942857142857143,
0.971428571428572,1.),.UNSPECIFIED.)
CURVE()
GEOMETRIC_REPRESENTATION_ITEM()
RATIONAL_B_SPLINE_CURVE((1.,1.,1.,1.,1.,1.,1.,1.,1.,1.,1.,1.,1.,1.,1.,1.,
1.,1.,1.,1.,1.,1.,1.,1.,1.,1.,1.,1.,1.))
REPRESENTATION_ITEM('')
);
#806=(
BOUNDED_CURVE()
B_SPLINE_CURVE(5,(#53743,#53744,#53745,#53746,#53747,#53748,#53749,#53750,
#53751,#53752,#53753,#53754,#53755,#53756,#53757,#53758,#53759,#53760,#53761,
#53762,#53763,#53764,#53765,#53766,#53767,#53768,#53769,#53770,#53771,#53772,
#53773,#53774,#53775,#53776),.UNSPECIFIED.,.F.,.F.)
B_SPLINE_CURVE_WITH_KNOTS((6,1,1,1,1,1,1,1,1,1,1,1,1,1,1,1,1,1,1,1,1,1,
1,1,1,1,1,1,1,6),(0.,0.0285714285714286,0.0571428571428571,0.0857142857142857,
0.114285714285714,0.142857142857143,0.171428571428571,0.2,0.228571428571429,
0.257142857142857,0.285714285714286,0.314285714285714,0.342857142857143,
0.371428571428571,0.4,0.428571428571429,0.457142857142857,0.485714285714286,
0.514285714285714,0.542857142857143,0.571428571428572,0.6,0.628571428571429,
0.657142857142857,0.685714285714286,0.714285714285714,0.742857142857143,
0.771428571428572,0.8,0.816564825616034),.UNSPECIFIED.)
CURVE()
GEOMETRIC_REPRESENTATION_ITEM()
RATIONAL_B_SPLINE_CURVE((1.,1.,1.,1.,1.,1.,1.,1.,1.,1.,1.,1.,1.,1.,1.,1.,
1.,1.,1.,1.,1.,1.,1.,1.,1.,1.,1.,1.,1.,1.,1.,1.,1.,1.))
REPRESENTATION_ITEM('')
);
#807=(
BOUNDED_CURVE()
B_SPLINE_CURVE(5,(#53780,#53781,#53782,#53783,#53784,#53785,#53786,#53787,
#53788,#53789,#53790,#53791,#53792,#53793,#53794,#53795,#53796,#53797,#53798,
#53799,#53800,#53801,#53802,#53803,#53804,#53805,#53806,#53807,#53808),
 .UNSPECIFIED.,.F.,.F.)
B_SPLINE_CURVE_WITH_KNOTS((6,1,1,1,1,1,1,1,1,1,1,1,1,1,1,1,1,1,1,1,1,1,
1,1,6),(0.31572829177571,0.342857142857143,0.371428571428571,0.4,0.428571428571429,
0.457142857142857,0.485714285714286,0.514285714285714,0.542857142857143,
0.571428571428572,0.6,0.628571428571429,0.657142857142857,0.685714285714286,
0.714285714285714,0.742857142857143,0.771428571428572,0.8,0.828571428571429,
0.857142857142857,0.885714285714286,0.914285714285714,0.942857142857143,
0.971428571428572,1.),.UNSPECIFIED.)
CURVE()
GEOMETRIC_REPRESENTATION_ITEM()
RATIONAL_B_SPLINE_CURVE((1.,1.,1.,1.,1.,1.,1.,1.,1.,1.,1.,1.,1.,1.,1.,1.,
1.,1.,1.,1.,1.,1.,1.,1.,1.,1.,1.,1.,1.))
REPRESENTATION_ITEM('')
);
#808=(
BOUNDED_CURVE()
B_SPLINE_CURVE(5,(#53812,#53813,#53814,#53815,#53816,#53817,#53818,#53819,
#53820,#53821,#53822,#53823,#53824,#53825,#53826,#53827,#53828,#53829,#53830,
#53831,#53832,#53833,#53834,#53835,#53836,#53837,#53838,#53839,#53840,#53841,
#53842,#53843,#53844,#53845),.UNSPECIFIED.,.F.,.F.)
B_SPLINE_CURVE_WITH_KNOTS((6,1,1,1,1,1,1,1,1,1,1,1,1,1,1,1,1,1,1,1,1,1,
1,1,1,1,1,1,1,6),(0.,0.0285714285714286,0.0571428571428571,0.0857142857142857,
0.114285714285714,0.142857142857143,0.171428571428571,0.2,0.228571428571429,
0.257142857142857,0.285714285714286,0.314285714285714,0.342857142857143,
0.371428571428571,0.4,0.428571428571429,0.457142857142857,0.485714285714286,
0.514285714285714,0.542857142857143,0.571428571428572,0.6,0.628571428571429,
0.657142857142857,0.685714285714286,0.714285714285714,0.742857142857143,
0.771428571428572,0.8,0.816564825616131),.UNSPECIFIED.)
CURVE()
GEOMETRIC_REPRESENTATION_ITEM()
RATIONAL_B_SPLINE_CURVE((1.,1.,1.,1.,1.,1.,1.,1.,1.,1.,1.,1.,1.,1.,1.,1.,
1.,1.,1.,1.,1.,1.,1.,1.,1.,1.,1.,1.,1.,1.,1.,1.,1.,1.))
REPRESENTATION_ITEM('')
);
#809=(
BOUNDED_CURVE()
B_SPLINE_CURVE(5,(#53849,#53850,#53851,#53852,#53853,#53854,#53855,#53856,
#53857,#53858,#53859,#53860,#53861,#53862,#53863,#53864,#53865,#53866,#53867,
#53868,#53869,#53870,#53871,#53872,#53873,#53874,#53875,#53876,#53877),
 .UNSPECIFIED.,.F.,.F.)
B_SPLINE_CURVE_WITH_KNOTS((6,1,1,1,1,1,1,1,1,1,1,1,1,1,1,1,1,1,1,1,1,1,
1,1,6),(0.315728291775709,0.342857142857143,0.371428571428571,0.4,0.428571428571429,
0.457142857142857,0.485714285714286,0.514285714285714,0.542857142857143,
0.571428571428572,0.6,0.628571428571429,0.657142857142857,0.685714285714286,
0.714285714285714,0.742857142857143,0.771428571428572,0.8,0.828571428571429,
0.857142857142857,0.885714285714286,0.914285714285714,0.942857142857143,
0.971428571428572,1.),.UNSPECIFIED.)
CURVE()
GEOMETRIC_REPRESENTATION_ITEM()
RATIONAL_B_SPLINE_CURVE((1.,1.,1.,1.,1.,1.,1.,1.,1.,1.,1.,1.,1.,1.,1.,1.,
1.,1.,1.,1.,1.,1.,1.,1.,1.,1.,1.,1.,1.))
REPRESENTATION_ITEM('')
);
#810=(
BOUNDED_CURVE()
B_SPLINE_CURVE(5,(#53881,#53882,#53883,#53884,#53885,#53886,#53887,#53888,
#53889,#53890,#53891,#53892,#53893,#53894,#53895,#53896,#53897,#53898,#53899,
#53900,#53901,#53902,#53903,#53904,#53905,#53906,#53907,#53908,#53909,#53910,
#53911,#53912,#53913,#53914),.UNSPECIFIED.,.F.,.F.)
B_SPLINE_CURVE_WITH_KNOTS((6,1,1,1,1,1,1,1,1,1,1,1,1,1,1,1,1,1,1,1,1,1,
1,1,1,1,1,1,1,6),(0.,0.0285714285714286,0.0571428571428571,0.0857142857142857,
0.114285714285714,0.142857142857143,0.171428571428571,0.2,0.228571428571429,
0.257142857142857,0.285714285714286,0.314285714285714,0.342857142857143,
0.371428571428571,0.4,0.428571428571429,0.457142857142857,0.485714285714286,
0.514285714285714,0.542857142857143,0.571428571428572,0.6,0.628571428571429,
0.657142857142857,0.685714285714286,0.714285714285714,0.742857142857143,
0.771428571428572,0.8,0.816564825616034),.UNSPECIFIED.)
CURVE()
GEOMETRIC_REPRESENTATION_ITEM()
RATIONAL_B_SPLINE_CURVE((1.,1.,1.,1.,1.,1.,1.,1.,1.,1.,1.,1.,1.,1.,1.,1.,
1.,1.,1.,1.,1.,1.,1.,1.,1.,1.,1.,1.,1.,1.,1.,1.,1.,1.))
REPRESENTATION_ITEM('')
);
#811=(
BOUNDED_CURVE()
B_SPLINE_CURVE(5,(#53918,#53919,#53920,#53921,#53922,#53923,#53924,#53925,
#53926,#53927,#53928,#53929,#53930,#53931,#53932,#53933,#53934,#53935,#53936,
#53937,#53938,#53939,#53940,#53941,#53942,#53943,#53944,#53945,#53946),
 .UNSPECIFIED.,.F.,.F.)
B_SPLINE_CURVE_WITH_KNOTS((6,1,1,1,1,1,1,1,1,1,1,1,1,1,1,1,1,1,1,1,1,1,
1,1,6),(0.315728291775709,0.342857142857143,0.371428571428571,0.4,0.428571428571429,
0.457142857142857,0.485714285714286,0.514285714285714,0.542857142857143,
0.571428571428572,0.6,0.628571428571429,0.657142857142857,0.685714285714286,
0.714285714285714,0.742857142857143,0.771428571428572,0.8,0.828571428571429,
0.857142857142857,0.885714285714286,0.914285714285714,0.942857142857143,
0.971428571428572,1.),.UNSPECIFIED.)
CURVE()
GEOMETRIC_REPRESENTATION_ITEM()
RATIONAL_B_SPLINE_CURVE((1.,1.,1.,1.,1.,1.,1.,1.,1.,1.,1.,1.,1.,1.,1.,1.,
1.,1.,1.,1.,1.,1.,1.,1.,1.,1.,1.,1.,1.))
REPRESENTATION_ITEM('')
);
#812=(
BOUNDED_CURVE()
B_SPLINE_CURVE(5,(#53950,#53951,#53952,#53953,#53954,#53955,#53956,#53957,
#53958,#53959,#53960,#53961,#53962,#53963,#53964,#53965,#53966,#53967,#53968,
#53969,#53970,#53971,#53972,#53973,#53974,#53975,#53976,#53977,#53978,#53979,
#53980,#53981,#53982,#53983),.UNSPECIFIED.,.F.,.F.)
B_SPLINE_CURVE_WITH_KNOTS((6,1,1,1,1,1,1,1,1,1,1,1,1,1,1,1,1,1,1,1,1,1,
1,1,1,1,1,1,1,6),(0.,0.0285714285714286,0.0571428571428571,0.0857142857142857,
0.114285714285714,0.142857142857143,0.171428571428571,0.2,0.228571428571429,
0.257142857142857,0.285714285714286,0.314285714285714,0.342857142857143,
0.371428571428571,0.4,0.428571428571429,0.457142857142857,0.485714285714286,
0.514285714285714,0.542857142857143,0.571428571428572,0.6,0.628571428571429,
0.657142857142857,0.685714285714286,0.714285714285714,0.742857142857143,
0.771428571428572,0.8,0.816564825616131),.UNSPECIFIED.)
CURVE()
GEOMETRIC_REPRESENTATION_ITEM()
RATIONAL_B_SPLINE_CURVE((1.,1.,1.,1.,1.,1.,1.,1.,1.,1.,1.,1.,1.,1.,1.,1.,
1.,1.,1.,1.,1.,1.,1.,1.,1.,1.,1.,1.,1.,1.,1.,1.,1.,1.))
REPRESENTATION_ITEM('')
);
#813=(
BOUNDED_CURVE()
B_SPLINE_CURVE(5,(#53987,#53988,#53989,#53990,#53991,#53992,#53993,#53994,
#53995,#53996,#53997,#53998,#53999,#54000,#54001,#54002,#54003,#54004,#54005,
#54006,#54007,#54008,#54009,#54010,#54011,#54012,#54013,#54014,#54015),
 .UNSPECIFIED.,.F.,.F.)
B_SPLINE_CURVE_WITH_KNOTS((6,1,1,1,1,1,1,1,1,1,1,1,1,1,1,1,1,1,1,1,1,1,
1,1,6),(0.315728291775709,0.342857142857143,0.371428571428571,0.4,0.428571428571429,
0.457142857142857,0.485714285714286,0.514285714285714,0.542857142857143,
0.571428571428572,0.6,0.628571428571429,0.657142857142857,0.685714285714286,
0.714285714285714,0.742857142857143,0.771428571428572,0.8,0.828571428571429,
0.857142857142857,0.885714285714286,0.914285714285714,0.942857142857143,
0.971428571428572,1.),.UNSPECIFIED.)
CURVE()
GEOMETRIC_REPRESENTATION_ITEM()
RATIONAL_B_SPLINE_CURVE((1.,1.,1.,1.,1.,1.,1.,1.,1.,1.,1.,1.,1.,1.,1.,1.,
1.,1.,1.,1.,1.,1.,1.,1.,1.,1.,1.,1.,1.))
REPRESENTATION_ITEM('')
);
#814=(
BOUNDED_CURVE()
B_SPLINE_CURVE(5,(#54019,#54020,#54021,#54022,#54023,#54024,#54025,#54026,
#54027,#54028,#54029,#54030,#54031,#54032,#54033,#54034,#54035,#54036,#54037,
#54038,#54039,#54040,#54041,#54042,#54043,#54044,#54045,#54046,#54047,#54048,
#54049,#54050,#54051,#54052),.UNSPECIFIED.,.F.,.F.)
B_SPLINE_CURVE_WITH_KNOTS((6,1,1,1,1,1,1,1,1,1,1,1,1,1,1,1,1,1,1,1,1,1,
1,1,1,1,1,1,1,6),(0.,0.0285714285714286,0.0571428571428571,0.0857142857142857,
0.114285714285714,0.142857142857143,0.171428571428571,0.2,0.228571428571429,
0.257142857142857,0.285714285714286,0.314285714285714,0.342857142857143,
0.371428571428571,0.4,0.428571428571429,0.457142857142857,0.485714285714286,
0.514285714285714,0.542857142857143,0.571428571428572,0.6,0.628571428571429,
0.657142857142857,0.685714285714286,0.714285714285714,0.742857142857143,
0.771428571428572,0.8,0.816564825616033),.UNSPECIFIED.)
CURVE()
GEOMETRIC_REPRESENTATION_ITEM()
RATIONAL_B_SPLINE_CURVE((1.,1.,1.,1.,1.,1.,1.,1.,1.,1.,1.,1.,1.,1.,1.,1.,
1.,1.,1.,1.,1.,1.,1.,1.,1.,1.,1.,1.,1.,1.,1.,1.,1.,1.))
REPRESENTATION_ITEM('')
);
#815=(
BOUNDED_CURVE()
B_SPLINE_CURVE(5,(#54056,#54057,#54058,#54059,#54060,#54061,#54062,#54063,
#54064,#54065,#54066,#54067,#54068,#54069,#54070,#54071,#54072,#54073,#54074,
#54075,#54076,#54077,#54078,#54079,#54080,#54081,#54082,#54083,#54084),
 .UNSPECIFIED.,.F.,.F.)
B_SPLINE_CURVE_WITH_KNOTS((6,1,1,1,1,1,1,1,1,1,1,1,1,1,1,1,1,1,1,1,1,1,
1,1,6),(0.31572829177571,0.342857142857143,0.371428571428571,0.4,0.428571428571429,
0.457142857142857,0.485714285714286,0.514285714285714,0.542857142857143,
0.571428571428572,0.6,0.628571428571429,0.657142857142857,0.685714285714286,
0.714285714285714,0.742857142857143,0.771428571428572,0.8,0.828571428571429,
0.857142857142857,0.885714285714286,0.914285714285714,0.942857142857143,
0.971428571428572,1.),.UNSPECIFIED.)
CURVE()
GEOMETRIC_REPRESENTATION_ITEM()
RATIONAL_B_SPLINE_CURVE((1.,1.,1.,1.,1.,1.,1.,1.,1.,1.,1.,1.,1.,1.,1.,1.,
1.,1.,1.,1.,1.,1.,1.,1.,1.,1.,1.,1.,1.))
REPRESENTATION_ITEM('')
);
#816=(
BOUNDED_CURVE()
B_SPLINE_CURVE(5,(#54088,#54089,#54090,#54091,#54092,#54093,#54094,#54095,
#54096,#54097,#54098,#54099,#54100,#54101,#54102,#54103,#54104,#54105,#54106,
#54107,#54108,#54109,#54110,#54111,#54112,#54113,#54114,#54115,#54116,#54117,
#54118,#54119,#54120,#54121),.UNSPECIFIED.,.F.,.F.)
B_SPLINE_CURVE_WITH_KNOTS((6,1,1,1,1,1,1,1,1,1,1,1,1,1,1,1,1,1,1,1,1,1,
1,1,1,1,1,1,1,6),(0.,0.0285714285714286,0.0571428571428571,0.0857142857142857,
0.114285714285714,0.142857142857143,0.171428571428571,0.2,0.228571428571429,
0.257142857142857,0.285714285714286,0.314285714285714,0.342857142857143,
0.371428571428571,0.4,0.428571428571429,0.457142857142857,0.485714285714286,
0.514285714285714,0.542857142857143,0.571428571428572,0.6,0.628571428571429,
0.657142857142857,0.685714285714286,0.714285714285714,0.742857142857143,
0.771428571428572,0.8,0.816564825616131),.UNSPECIFIED.)
CURVE()
GEOMETRIC_REPRESENTATION_ITEM()
RATIONAL_B_SPLINE_CURVE((1.,1.,1.,1.,1.,1.,1.,1.,1.,1.,1.,1.,1.,1.,1.,1.,
1.,1.,1.,1.,1.,1.,1.,1.,1.,1.,1.,1.,1.,1.,1.,1.,1.,1.))
REPRESENTATION_ITEM('')
);
#817=(
BOUNDED_CURVE()
B_SPLINE_CURVE(5,(#54125,#54126,#54127,#54128,#54129,#54130,#54131,#54132,
#54133,#54134,#54135,#54136,#54137,#54138,#54139,#54140,#54141,#54142,#54143,
#54144,#54145,#54146,#54147,#54148,#54149,#54150,#54151,#54152,#54153),
 .UNSPECIFIED.,.F.,.F.)
B_SPLINE_CURVE_WITH_KNOTS((6,1,1,1,1,1,1,1,1,1,1,1,1,1,1,1,1,1,1,1,1,1,
1,1,6),(0.315728291775709,0.342857142857143,0.371428571428571,0.4,0.428571428571429,
0.457142857142857,0.485714285714286,0.514285714285714,0.542857142857143,
0.571428571428572,0.6,0.628571428571429,0.657142857142857,0.685714285714286,
0.714285714285714,0.742857142857143,0.771428571428572,0.8,0.828571428571429,
0.857142857142857,0.885714285714286,0.914285714285714,0.942857142857143,
0.971428571428572,1.),.UNSPECIFIED.)
CURVE()
GEOMETRIC_REPRESENTATION_ITEM()
RATIONAL_B_SPLINE_CURVE((1.,1.,1.,1.,1.,1.,1.,1.,1.,1.,1.,1.,1.,1.,1.,1.,
1.,1.,1.,1.,1.,1.,1.,1.,1.,1.,1.,1.,1.))
REPRESENTATION_ITEM('')
);
#818=(
BOUNDED_CURVE()
B_SPLINE_CURVE(5,(#54157,#54158,#54159,#54160,#54161,#54162,#54163,#54164,
#54165,#54166,#54167,#54168,#54169,#54170,#54171,#54172,#54173,#54174,#54175,
#54176,#54177,#54178,#54179,#54180,#54181,#54182,#54183,#54184,#54185,#54186,
#54187,#54188,#54189,#54190),.UNSPECIFIED.,.F.,.F.)
B_SPLINE_CURVE_WITH_KNOTS((6,1,1,1,1,1,1,1,1,1,1,1,1,1,1,1,1,1,1,1,1,1,
1,1,1,1,1,1,1,6),(0.,0.0285714285714286,0.0571428571428571,0.0857142857142857,
0.114285714285714,0.142857142857143,0.171428571428571,0.2,0.228571428571429,
0.257142857142857,0.285714285714286,0.314285714285714,0.342857142857143,
0.371428571428571,0.4,0.428571428571429,0.457142857142857,0.485714285714286,
0.514285714285714,0.542857142857143,0.571428571428572,0.6,0.628571428571429,
0.657142857142857,0.685714285714286,0.714285714285714,0.742857142857143,
0.771428571428572,0.8,0.816564825616034),.UNSPECIFIED.)
CURVE()
GEOMETRIC_REPRESENTATION_ITEM()
RATIONAL_B_SPLINE_CURVE((1.,1.,1.,1.,1.,1.,1.,1.,1.,1.,1.,1.,1.,1.,1.,1.,
1.,1.,1.,1.,1.,1.,1.,1.,1.,1.,1.,1.,1.,1.,1.,1.,1.,1.))
REPRESENTATION_ITEM('')
);
#819=(
BOUNDED_CURVE()
B_SPLINE_CURVE(5,(#54194,#54195,#54196,#54197,#54198,#54199,#54200,#54201,
#54202,#54203,#54204,#54205,#54206,#54207,#54208,#54209,#54210,#54211,#54212,
#54213,#54214,#54215,#54216,#54217,#54218,#54219,#54220,#54221,#54222),
 .UNSPECIFIED.,.F.,.F.)
B_SPLINE_CURVE_WITH_KNOTS((6,1,1,1,1,1,1,1,1,1,1,1,1,1,1,1,1,1,1,1,1,1,
1,1,6),(0.315728291775709,0.342857142857143,0.371428571428571,0.4,0.428571428571429,
0.457142857142857,0.485714285714286,0.514285714285714,0.542857142857143,
0.571428571428572,0.6,0.628571428571429,0.657142857142857,0.685714285714286,
0.714285714285714,0.742857142857143,0.771428571428572,0.8,0.828571428571429,
0.857142857142857,0.885714285714286,0.914285714285714,0.942857142857143,
0.971428571428572,1.),.UNSPECIFIED.)
CURVE()
GEOMETRIC_REPRESENTATION_ITEM()
RATIONAL_B_SPLINE_CURVE((1.,1.,1.,1.,1.,1.,1.,1.,1.,1.,1.,1.,1.,1.,1.,1.,
1.,1.,1.,1.,1.,1.,1.,1.,1.,1.,1.,1.,1.))
REPRESENTATION_ITEM('')
);
#820=(
BOUNDED_CURVE()
B_SPLINE_CURVE(5,(#54226,#54227,#54228,#54229,#54230,#54231,#54232,#54233,
#54234,#54235,#54236,#54237,#54238,#54239,#54240,#54241,#54242,#54243,#54244,
#54245,#54246,#54247,#54248,#54249,#54250,#54251,#54252,#54253,#54254,#54255,
#54256,#54257,#54258,#54259),.UNSPECIFIED.,.F.,.F.)
B_SPLINE_CURVE_WITH_KNOTS((6,1,1,1,1,1,1,1,1,1,1,1,1,1,1,1,1,1,1,1,1,1,
1,1,1,1,1,1,1,6),(0.,0.0285714285714286,0.0571428571428571,0.0857142857142857,
0.114285714285714,0.142857142857143,0.171428571428571,0.2,0.228571428571429,
0.257142857142857,0.285714285714286,0.314285714285714,0.342857142857143,
0.371428571428571,0.4,0.428571428571429,0.457142857142857,0.485714285714286,
0.514285714285714,0.542857142857143,0.571428571428572,0.6,0.628571428571429,
0.657142857142857,0.685714285714286,0.714285714285714,0.742857142857143,
0.771428571428572,0.8,0.816564825616131),.UNSPECIFIED.)
CURVE()
GEOMETRIC_REPRESENTATION_ITEM()
RATIONAL_B_SPLINE_CURVE((1.,1.,1.,1.,1.,1.,1.,1.,1.,1.,1.,1.,1.,1.,1.,1.,
1.,1.,1.,1.,1.,1.,1.,1.,1.,1.,1.,1.,1.,1.,1.,1.,1.,1.))
REPRESENTATION_ITEM('')
);
#821=(
BOUNDED_CURVE()
B_SPLINE_CURVE(5,(#54263,#54264,#54265,#54266,#54267,#54268,#54269,#54270,
#54271,#54272,#54273,#54274,#54275,#54276,#54277,#54278,#54279,#54280,#54281,
#54282,#54283,#54284,#54285,#54286,#54287,#54288,#54289,#54290,#54291),
 .UNSPECIFIED.,.F.,.F.)
B_SPLINE_CURVE_WITH_KNOTS((6,1,1,1,1,1,1,1,1,1,1,1,1,1,1,1,1,1,1,1,1,1,
1,1,6),(0.31572829177571,0.342857142857143,0.371428571428571,0.4,0.428571428571429,
0.457142857142857,0.485714285714286,0.514285714285714,0.542857142857143,
0.571428571428572,0.6,0.628571428571429,0.657142857142857,0.685714285714286,
0.714285714285714,0.742857142857143,0.771428571428572,0.8,0.828571428571429,
0.857142857142857,0.885714285714286,0.914285714285714,0.942857142857143,
0.971428571428572,1.),.UNSPECIFIED.)
CURVE()
GEOMETRIC_REPRESENTATION_ITEM()
RATIONAL_B_SPLINE_CURVE((1.,1.,1.,1.,1.,1.,1.,1.,1.,1.,1.,1.,1.,1.,1.,1.,
1.,1.,1.,1.,1.,1.,1.,1.,1.,1.,1.,1.,1.))
REPRESENTATION_ITEM('')
);
#822=(
BOUNDED_CURVE()
B_SPLINE_CURVE(5,(#54295,#54296,#54297,#54298,#54299,#54300,#54301,#54302,
#54303,#54304,#54305,#54306,#54307,#54308,#54309,#54310,#54311,#54312,#54313,
#54314,#54315,#54316,#54317,#54318,#54319,#54320,#54321,#54322,#54323,#54324,
#54325,#54326,#54327,#54328),.UNSPECIFIED.,.F.,.F.)
B_SPLINE_CURVE_WITH_KNOTS((6,1,1,1,1,1,1,1,1,1,1,1,1,1,1,1,1,1,1,1,1,1,
1,1,1,1,1,1,1,6),(0.,0.0285714285714286,0.0571428571428571,0.0857142857142857,
0.114285714285714,0.142857142857143,0.171428571428571,0.2,0.228571428571429,
0.257142857142857,0.285714285714286,0.314285714285714,0.342857142857143,
0.371428571428571,0.4,0.428571428571429,0.457142857142857,0.485714285714286,
0.514285714285714,0.542857142857143,0.571428571428572,0.6,0.628571428571429,
0.657142857142857,0.685714285714286,0.714285714285714,0.742857142857143,
0.771428571428572,0.8,0.816564825616034),.UNSPECIFIED.)
CURVE()
GEOMETRIC_REPRESENTATION_ITEM()
RATIONAL_B_SPLINE_CURVE((1.,1.,1.,1.,1.,1.,1.,1.,1.,1.,1.,1.,1.,1.,1.,1.,
1.,1.,1.,1.,1.,1.,1.,1.,1.,1.,1.,1.,1.,1.,1.,1.,1.,1.))
REPRESENTATION_ITEM('')
);
#823=(
BOUNDED_CURVE()
B_SPLINE_CURVE(5,(#54332,#54333,#54334,#54335,#54336,#54337,#54338,#54339,
#54340,#54341,#54342,#54343,#54344,#54345,#54346,#54347,#54348,#54349,#54350,
#54351,#54352,#54353,#54354,#54355,#54356,#54357,#54358,#54359,#54360),
 .UNSPECIFIED.,.F.,.F.)
B_SPLINE_CURVE_WITH_KNOTS((6,1,1,1,1,1,1,1,1,1,1,1,1,1,1,1,1,1,1,1,1,1,
1,1,6),(0.31572829177571,0.342857142857143,0.371428571428571,0.4,0.428571428571429,
0.457142857142857,0.485714285714286,0.514285714285714,0.542857142857143,
0.571428571428572,0.6,0.628571428571429,0.657142857142857,0.685714285714286,
0.714285714285714,0.742857142857143,0.771428571428572,0.8,0.828571428571429,
0.857142857142857,0.885714285714286,0.914285714285714,0.942857142857143,
0.971428571428572,1.),.UNSPECIFIED.)
CURVE()
GEOMETRIC_REPRESENTATION_ITEM()
RATIONAL_B_SPLINE_CURVE((1.,1.,1.,1.,1.,1.,1.,1.,1.,1.,1.,1.,1.,1.,1.,1.,
1.,1.,1.,1.,1.,1.,1.,1.,1.,1.,1.,1.,1.))
REPRESENTATION_ITEM('')
);
#824=(
BOUNDED_CURVE()
B_SPLINE_CURVE(5,(#54364,#54365,#54366,#54367,#54368,#54369,#54370,#54371,
#54372,#54373,#54374,#54375,#54376,#54377,#54378,#54379,#54380,#54381,#54382,
#54383,#54384,#54385,#54386,#54387,#54388,#54389,#54390,#54391,#54392,#54393,
#54394,#54395,#54396,#54397),.UNSPECIFIED.,.F.,.F.)
B_SPLINE_CURVE_WITH_KNOTS((6,1,1,1,1,1,1,1,1,1,1,1,1,1,1,1,1,1,1,1,1,1,
1,1,1,1,1,1,1,6),(0.,0.0285714285714286,0.0571428571428571,0.0857142857142857,
0.114285714285714,0.142857142857143,0.171428571428571,0.2,0.228571428571429,
0.257142857142857,0.285714285714286,0.314285714285714,0.342857142857143,
0.371428571428571,0.4,0.428571428571429,0.457142857142857,0.485714285714286,
0.514285714285714,0.542857142857143,0.571428571428572,0.6,0.628571428571429,
0.657142857142857,0.685714285714286,0.714285714285714,0.742857142857143,
0.771428571428572,0.8,0.816564825616131),.UNSPECIFIED.)
CURVE()
GEOMETRIC_REPRESENTATION_ITEM()
RATIONAL_B_SPLINE_CURVE((1.,1.,1.,1.,1.,1.,1.,1.,1.,1.,1.,1.,1.,1.,1.,1.,
1.,1.,1.,1.,1.,1.,1.,1.,1.,1.,1.,1.,1.,1.,1.,1.,1.,1.))
REPRESENTATION_ITEM('')
);
#825=(
BOUNDED_CURVE()
B_SPLINE_CURVE(5,(#54401,#54402,#54403,#54404,#54405,#54406,#54407,#54408,
#54409,#54410,#54411,#54412,#54413,#54414,#54415,#54416,#54417,#54418,#54419,
#54420,#54421,#54422,#54423,#54424,#54425,#54426,#54427,#54428,#54429),
 .UNSPECIFIED.,.F.,.F.)
B_SPLINE_CURVE_WITH_KNOTS((6,1,1,1,1,1,1,1,1,1,1,1,1,1,1,1,1,1,1,1,1,1,
1,1,6),(0.315728291775709,0.342857142857143,0.371428571428571,0.4,0.428571428571429,
0.457142857142857,0.485714285714286,0.514285714285714,0.542857142857143,
0.571428571428572,0.6,0.628571428571429,0.657142857142857,0.685714285714286,
0.714285714285714,0.742857142857143,0.771428571428572,0.8,0.828571428571429,
0.857142857142857,0.885714285714286,0.914285714285714,0.942857142857143,
0.971428571428572,1.),.UNSPECIFIED.)
CURVE()
GEOMETRIC_REPRESENTATION_ITEM()
RATIONAL_B_SPLINE_CURVE((1.,1.,1.,1.,1.,1.,1.,1.,1.,1.,1.,1.,1.,1.,1.,1.,
1.,1.,1.,1.,1.,1.,1.,1.,1.,1.,1.,1.,1.))
REPRESENTATION_ITEM('')
);
#826=(
BOUNDED_CURVE()
B_SPLINE_CURVE(5,(#54433,#54434,#54435,#54436,#54437,#54438,#54439,#54440,
#54441,#54442,#54443,#54444,#54445,#54446,#54447,#54448,#54449,#54450,#54451,
#54452,#54453,#54454,#54455,#54456,#54457,#54458,#54459,#54460,#54461,#54462,
#54463,#54464,#54465,#54466),.UNSPECIFIED.,.F.,.F.)
B_SPLINE_CURVE_WITH_KNOTS((6,1,1,1,1,1,1,1,1,1,1,1,1,1,1,1,1,1,1,1,1,1,
1,1,1,1,1,1,1,6),(0.,0.0285714285714286,0.0571428571428571,0.0857142857142857,
0.114285714285714,0.142857142857143,0.171428571428571,0.2,0.228571428571429,
0.257142857142857,0.285714285714286,0.314285714285714,0.342857142857143,
0.371428571428571,0.4,0.428571428571429,0.457142857142857,0.485714285714286,
0.514285714285714,0.542857142857143,0.571428571428572,0.6,0.628571428571429,
0.657142857142857,0.685714285714286,0.714285714285714,0.742857142857143,
0.771428571428572,0.8,0.816564825616131),.UNSPECIFIED.)
CURVE()
GEOMETRIC_REPRESENTATION_ITEM()
RATIONAL_B_SPLINE_CURVE((1.,1.,1.,1.,1.,1.,1.,1.,1.,1.,1.,1.,1.,1.,1.,1.,
1.,1.,1.,1.,1.,1.,1.,1.,1.,1.,1.,1.,1.,1.,1.,1.,1.,1.))
REPRESENTATION_ITEM('')
);
#827=(
BOUNDED_CURVE()
B_SPLINE_CURVE(5,(#54469,#54470,#54471,#54472,#54473,#54474,#54475,#54476,
#54477,#54478,#54479,#54480,#54481,#54482,#54483,#54484,#54485,#54486,#54487,
#54488,#54489,#54490,#54491,#54492,#54493,#54494,#54495,#54496,#54497),
 .UNSPECIFIED.,.F.,.F.)
B_SPLINE_CURVE_WITH_KNOTS((6,1,1,1,1,1,1,1,1,1,1,1,1,1,1,1,1,1,1,1,1,1,
1,1,6),(0.315728291775709,0.342857142857143,0.371428571428571,0.4,0.428571428571429,
0.457142857142857,0.485714285714286,0.514285714285714,0.542857142857143,
0.571428571428572,0.6,0.628571428571429,0.657142857142857,0.685714285714286,
0.714285714285714,0.742857142857143,0.771428571428572,0.8,0.828571428571429,
0.857142857142857,0.885714285714286,0.914285714285714,0.942857142857143,
0.971428571428572,1.),.UNSPECIFIED.)
CURVE()
GEOMETRIC_REPRESENTATION_ITEM()
RATIONAL_B_SPLINE_CURVE((1.,1.,1.,1.,1.,1.,1.,1.,1.,1.,1.,1.,1.,1.,1.,1.,
1.,1.,1.,1.,1.,1.,1.,1.,1.,1.,1.,1.,1.))
REPRESENTATION_ITEM('')
);
#828=(
BOUNDED_CURVE()
B_SPLINE_CURVE(2,(#64727,#64728,#64729),.UNSPECIFIED.,.F.,.F.)
B_SPLINE_CURVE_WITH_KNOTS((3,3),(0.338124280435932,0.360943681531408),
 .UNSPECIFIED.)
CURVE()
GEOMETRIC_REPRESENTATION_ITEM()
RATIONAL_B_SPLINE_CURVE((1.00248873269084,1.00246071159709,1.00241757299052))
REPRESENTATION_ITEM('')
);
#829=(
BOUNDED_CURVE()
B_SPLINE_CURVE(2,(#64784,#64785,#64786),.UNSPECIFIED.,.F.,.F.)
B_SPLINE_CURVE_WITH_KNOTS((3,3),(0.230710993510061,0.25353039460556),
 .UNSPECIFIED.)
CURVE()
GEOMETRIC_REPRESENTATION_ITEM()
RATIONAL_B_SPLINE_CURVE((1.00241757299153,1.00246071159813,1.00248873269188))
REPRESENTATION_ITEM('')
);
#830=(
BOUNDED_CURVE()
B_SPLINE_CURVE(2,(#64793,#64794,#64795),.UNSPECIFIED.,.F.,.F.)
B_SPLINE_CURVE_WITH_KNOTS((3,3),(0.338124280435769,0.360943681531267),
 .UNSPECIFIED.)
CURVE()
GEOMETRIC_REPRESENTATION_ITEM()
RATIONAL_B_SPLINE_CURVE((1.00248873269167,1.00246071159791,1.00241757299132))
REPRESENTATION_ITEM('')
);
#831=(
BOUNDED_CURVE()
B_SPLINE_CURVE(2,(#64802,#64803,#64804),.UNSPECIFIED.,.F.,.F.)
B_SPLINE_CURVE_WITH_KNOTS((3,3),(0.230710993510149,0.253530394605615),
 .UNSPECIFIED.)
CURVE()
GEOMETRIC_REPRESENTATION_ITEM()
RATIONAL_B_SPLINE_CURVE((1.00241757299006,1.00246071159663,1.00248873269037))
REPRESENTATION_ITEM('')
);
#832=(
BOUNDED_CURVE()
B_SPLINE_CURVE(2,(#64812,#64813,#64814),.UNSPECIFIED.,.F.,.F.)
B_SPLINE_CURVE_WITH_KNOTS((3,3),(0.230710993510133,0.253530394605583),
 .UNSPECIFIED.)
CURVE()
GEOMETRIC_REPRESENTATION_ITEM()
RATIONAL_B_SPLINE_CURVE((1.00241757298939,1.00246071159594,1.00248873268967))
REPRESENTATION_ITEM('')
);
#833=(
BOUNDED_CURVE()
B_SPLINE_CURVE(2,(#64818,#64819,#64820),.UNSPECIFIED.,.F.,.F.)
B_SPLINE_CURVE_WITH_KNOTS((3,3),(0.338124280435993,0.360943681531517),
 .UNSPECIFIED.)
CURVE()
GEOMETRIC_REPRESENTATION_ITEM()
RATIONAL_B_SPLINE_CURVE((1.00248873269308,1.00246071159931,1.0024175729927))
REPRESENTATION_ITEM('')
);
#834=B_SPLINE_SURFACE_WITH_KNOTS('',3,3,((#35741,#35742,#35743,#35744,#35745,
#35746,#35747,#35748,#35749,#35750,#35751,#35752,#35753,#35754,#35755,#35756,
#35757,#35758,#35759,#35760,#35761,#35762,#35763,#35764,#35765,#35766,#35767,
#35768,#35769,#35770,#35771,#35772,#35773,#35774,#35775,#35776,#35777,#35778,
#35779,#35780,#35781,#35782,#35783,#35784,#35785,#35786,#35787,#35788,#35789,
#35790,#35791,#35792,#35793,#35794,#35795,#35796,#35797,#35798,#35799,#35800,
#35801,#35802,#35803,#35804,#35805,#35806,#35807,#35808,#35809,#35810,#35811,
#35812,#35813,#35814,#35815,#35816,#35817,#35818,#35819,#35820,#35821,#35822,
#35823,#35824,#35825,#35826,#35827,#35828,#35829,#35830,#35831,#35832,#35833,
#35834,#35835,#35836,#35837,#35838,#35839,#35840,#35841,#35842,#35843,#35844,
#35845,#35846,#35847,#35848,#35849,#35850,#35851,#35852,#35853,#35854,#35855,
#35856,#35857,#35858,#35859,#35860,#35861,#35862,#35863,#35864,#35865,#35866,
#35867,#35868,#35869,#35870,#35871,#35872,#35873,#35874,#35875,#35876,#35877,
#35878,#35879,#35880,#35881,#35882,#35883,#35884,#35885,#35886,#35887,#35888,
#35889,#35890,#35891,#35892,#35893,#35894,#35895,#35896,#35897,#35898,#35899,
#35900,#35901,#35902,#35903,#35904,#35905,#35906,#35907,#35908,#35909,#35910,
#35911,#35912,#35913,#35914,#35915,#35916,#35917,#35918,#35919,#35920,#35921,
#35922,#35923,#35924,#35925,#35926,#35927,#35928,#35929,#35930,#35931,#35932,
#35933,#35934,#35935,#35936,#35937,#35938,#35939,#35940,#35941,#35942,#35943,
#35944,#35945,#35946,#35947,#35948,#35949,#35950,#35951,#35952,#35953,#35954,
#35955,#35956,#35957,#35958,#35959,#35960,#35961,#35962,#35963,#35964,#35965,
#35966,#35967,#35968,#35969,#35970,#35971,#35972,#35973,#35974,#35975,#35976,
#35977,#35978,#35979,#35980,#35981,#35982,#35983,#35984,#35985,#35986,#35987,
#35988,#35989,#35990,#35991,#35992,#35993,#35994,#35995,#35996,#35997,#35998,
#35999,#36000,#36001,#36002,#36003,#36004,#36005,#36006,#36007,#36008,#36009,
#36010,#36011,#36012,#36013,#36014,#36015,#36016,#36017,#36018,#36019,#36020,
#36021,#36022,#36023,#36024,#36025,#36026,#36027,#36028,#36029,#36030,#36031,
#36032,#36033,#36034,#36035,#36036,#36037,#36038,#36039,#36040,#36041,#36042,
#36043,#36044,#36045,#36046,#36047,#36048,#36049,#36050,#36051,#36052,#36053,
#36054,#36055,#36056,#36057,#36058,#36059,#36060,#36061,#36062,#36063,#36064,
#36065,#36066,#36067,#36068,#36069,#36070,#36071,#36072,#36073,#36074,#36075,
#36076,#36077,#36078,#36079,#36080,#36081,#36082,#36083,#36084,#36085,#36086,
#36087,#36088,#36089,#36090,#36091,#36092,#36093,#36094,#36095,#36096,#36097,
#36098,#36099,#36100,#36101,#36102,#36103,#36104,#36105,#36106,#36107,#36108,
#36109,#36110,#36111,#36112,#36113,#36114,#36115,#36116,#36117,#36118,#36119,
#36120,#36121,#36122,#36123,#36124,#36125,#36126,#36127,#36128,#36129,#36130,
#36131,#36132,#36133,#36134,#36135,#36136,#36137,#36138,#36139,#36140,#36141,
#36142,#36143,#36144,#36145,#36146,#36147,#36148,#36149,#36150,#36151,#36152,
#36153,#36154,#36155,#36156,#36157,#36158,#36159,#36160,#36161,#36162,#36163,
#36164,#36165,#36166,#36167,#36168,#36169,#36170,#36171,#36172,#36173,#36174,
#36175,#36176,#36177,#36178,#36179,#36180,#36181,#36182,#36183,#36184,#36185,
#36186,#36187,#36188,#36189,#36190,#36191,#36192,#36193,#36194,#36195,#36196,
#36197,#36198,#36199,#36200,#36201,#36202,#36203,#36204,#36205,#36206,#36207,
#36208,#36209,#36210,#36211,#36212,#36213,#36214,#36215,#36216,#36217,#36218,
#36219,#36220,#36221,#36222,#36223,#36224,#36225,#36226,#36227,#36228,#36229,
#36230,#36231,#36232,#36233,#36234,#36235,#36236,#36237,#36238,#36239,#36240,
#36241,#36242,#36243,#36244,#36245,#36246,#36247,#36248,#36249,#36250,#36251,
#36252,#36253),(#36254,#36255,#36256,#36257,#36258,#36259,#36260,#36261,
#36262,#36263,#36264,#36265,#36266,#36267,#36268,#36269,#36270,#36271,#36272,
#36273,#36274,#36275,#36276,#36277,#36278,#36279,#36280,#36281,#36282,#36283,
#36284,#36285,#36286,#36287,#36288,#36289,#36290,#36291,#36292,#36293,#36294,
#36295,#36296,#36297,#36298,#36299,#36300,#36301,#36302,#36303,#36304,#36305,
#36306,#36307,#36308,#36309,#36310,#36311,#36312,#36313,#36314,#36315,#36316,
#36317,#36318,#36319,#36320,#36321,#36322,#36323,#36324,#36325,#36326,#36327,
#36328,#36329,#36330,#36331,#36332,#36333,#36334,#36335,#36336,#36337,#36338,
#36339,#36340,#36341,#36342,#36343,#36344,#36345,#36346,#36347,#36348,#36349,
#36350,#36351,#36352,#36353,#36354,#36355,#36356,#36357,#36358,#36359,#36360,
#36361,#36362,#36363,#36364,#36365,#36366,#36367,#36368,#36369,#36370,#36371,
#36372,#36373,#36374,#36375,#36376,#36377,#36378,#36379,#36380,#36381,#36382,
#36383,#36384,#36385,#36386,#36387,#36388,#36389,#36390,#36391,#36392,#36393,
#36394,#36395,#36396,#36397,#36398,#36399,#36400,#36401,#36402,#36403,#36404,
#36405,#36406,#36407,#36408,#36409,#36410,#36411,#36412,#36413,#36414,#36415,
#36416,#36417,#36418,#36419,#36420,#36421,#36422,#36423,#36424,#36425,#36426,
#36427,#36428,#36429,#36430,#36431,#36432,#36433,#36434,#36435,#36436,#36437,
#36438,#36439,#36440,#36441,#36442,#36443,#36444,#36445,#36446,#36447,#36448,
#36449,#36450,#36451,#36452,#36453,#36454,#36455,#36456,#36457,#36458,#36459,
#36460,#36461,#36462,#36463,#36464,#36465,#36466,#36467,#36468,#36469,#36470,
#36471,#36472,#36473,#36474,#36475,#36476,#36477,#36478,#36479,#36480,#36481,
#36482,#36483,#36484,#36485,#36486,#36487,#36488,#36489,#36490,#36491,#36492,
#36493,#36494,#36495,#36496,#36497,#36498,#36499,#36500,#36501,#36502,#36503,
#36504,#36505,#36506,#36507,#36508,#36509,#36510,#36511,#36512,#36513,#36514,
#36515,#36516,#36517,#36518,#36519,#36520,#36521,#36522,#36523,#36524,#36525,
#36526,#36527,#36528,#36529,#36530,#36531,#36532,#36533,#36534,#36535,#36536,
#36537,#36538,#36539,#36540,#36541,#36542,#36543,#36544,#36545,#36546,#36547,
#36548,#36549,#36550,#36551,#36552,#36553,#36554,#36555,#36556,#36557,#36558,
#36559,#36560,#36561,#36562,#36563,#36564,#36565,#36566,#36567,#36568,#36569,
#36570,#36571,#36572,#36573,#36574,#36575,#36576,#36577,#36578,#36579,#36580,
#36581,#36582,#36583,#36584,#36585,#36586,#36587,#36588,#36589,#36590,#36591,
#36592,#36593,#36594,#36595,#36596,#36597,#36598,#36599,#36600,#36601,#36602,
#36603,#36604,#36605,#36606,#36607,#36608,#36609,#36610,#36611,#36612,#36613,
#36614,#36615,#36616,#36617,#36618,#36619,#36620,#36621,#36622,#36623,#36624,
#36625,#36626,#36627,#36628,#36629,#36630,#36631,#36632,#36633,#36634,#36635,
#36636,#36637,#36638,#36639,#36640,#36641,#36642,#36643,#36644,#36645,#36646,
#36647,#36648,#36649,#36650,#36651,#36652,#36653,#36654,#36655,#36656,#36657,
#36658,#36659,#36660,#36661,#36662,#36663,#36664,#36665,#36666,#36667,#36668,
#36669,#36670,#36671,#36672,#36673,#36674,#36675,#36676,#36677,#36678,#36679,
#36680,#36681,#36682,#36683,#36684,#36685,#36686,#36687,#36688,#36689,#36690,
#36691,#36692,#36693,#36694,#36695,#36696,#36697,#36698,#36699,#36700,#36701,
#36702,#36703,#36704,#36705,#36706,#36707,#36708,#36709,#36710,#36711,#36712,
#36713,#36714,#36715,#36716,#36717,#36718,#36719,#36720,#36721,#36722,#36723,
#36724,#36725,#36726,#36727,#36728,#36729,#36730,#36731,#36732,#36733,#36734,
#36735,#36736,#36737,#36738,#36739,#36740,#36741,#36742,#36743,#36744,#36745,
#36746,#36747,#36748,#36749,#36750,#36751,#36752,#36753,#36754,#36755,#36756,
#36757,#36758,#36759,#36760,#36761,#36762,#36763,#36764,#36765,#36766),
(#36767,#36768,#36769,#36770,#36771,#36772,#36773,#36774,#36775,#36776,
#36777,#36778,#36779,#36780,#36781,#36782,#36783,#36784,#36785,#36786,#36787,
#36788,#36789,#36790,#36791,#36792,#36793,#36794,#36795,#36796,#36797,#36798,
#36799,#36800,#36801,#36802,#36803,#36804,#36805,#36806,#36807,#36808,#36809,
#36810,#36811,#36812,#36813,#36814,#36815,#36816,#36817,#36818,#36819,#36820,
#36821,#36822,#36823,#36824,#36825,#36826,#36827,#36828,#36829,#36830,#36831,
#36832,#36833,#36834,#36835,#36836,#36837,#36838,#36839,#36840,#36841,#36842,
#36843,#36844,#36845,#36846,#36847,#36848,#36849,#36850,#36851,#36852,#36853,
#36854,#36855,#36856,#36857,#36858,#36859,#36860,#36861,#36862,#36863,#36864,
#36865,#36866,#36867,#36868,#36869,#36870,#36871,#36872,#36873,#36874,#36875,
#36876,#36877,#36878,#36879,#36880,#36881,#36882,#36883,#36884,#36885,#36886,
#36887,#36888,#36889,#36890,#36891,#36892,#36893,#36894,#36895,#36896,#36897,
#36898,#36899,#36900,#36901,#36902,#36903,#36904,#36905,#36906,#36907,#36908,
#36909,#36910,#36911,#36912,#36913,#36914,#36915,#36916,#36917,#36918,#36919,
#36920,#36921,#36922,#36923,#36924,#36925,#36926,#36927,#36928,#36929,#36930,
#36931,#36932,#36933,#36934,#36935,#36936,#36937,#36938,#36939,#36940,#36941,
#36942,#36943,#36944,#36945,#36946,#36947,#36948,#36949,#36950,#36951,#36952,
#36953,#36954,#36955,#36956,#36957,#36958,#36959,#36960,#36961,#36962,#36963,
#36964,#36965,#36966,#36967,#36968,#36969,#36970,#36971,#36972,#36973,#36974,
#36975,#36976,#36977,#36978,#36979,#36980,#36981,#36982,#36983,#36984,#36985,
#36986,#36987,#36988,#36989,#36990,#36991,#36992,#36993,#36994,#36995,#36996,
#36997,#36998,#36999,#37000,#37001,#37002,#37003,#37004,#37005,#37006,#37007,
#37008,#37009,#37010,#37011,#37012,#37013,#37014,#37015,#37016,#37017,#37018,
#37019,#37020,#37021,#37022,#37023,#37024,#37025,#37026,#37027,#37028,#37029,
#37030,#37031,#37032,#37033,#37034,#37035,#37036,#37037,#37038,#37039,#37040,
#37041,#37042,#37043,#37044,#37045,#37046,#37047,#37048,#37049,#37050,#37051,
#37052,#37053,#37054,#37055,#37056,#37057,#37058,#37059,#37060,#37061,#37062,
#37063,#37064,#37065,#37066,#37067,#37068,#37069,#37070,#37071,#37072,#37073,
#37074,#37075,#37076,#37077,#37078,#37079,#37080,#37081,#37082,#37083,#37084,
#37085,#37086,#37087,#37088,#37089,#37090,#37091,#37092,#37093,#37094,#37095,
#37096,#37097,#37098,#37099,#37100,#37101,#37102,#37103,#37104,#37105,#37106,
#37107,#37108,#37109,#37110,#37111,#37112,#37113,#37114,#37115,#37116,#37117,
#37118,#37119,#37120,#37121,#37122,#37123,#37124,#37125,#37126,#37127,#37128,
#37129,#37130,#37131,#37132,#37133,#37134,#37135,#37136,#37137,#37138,#37139,
#37140,#37141,#37142,#37143,#37144,#37145,#37146,#37147,#37148,#37149,#37150,
#37151,#37152,#37153,#37154,#37155,#37156,#37157,#37158,#37159,#37160,#37161,
#37162,#37163,#37164,#37165,#37166,#37167,#37168,#37169,#37170,#37171,#37172,
#37173,#37174,#37175,#37176,#37177,#37178,#37179,#37180,#37181,#37182,#37183,
#37184,#37185,#37186,#37187,#37188,#37189,#37190,#37191,#37192,#37193,#37194,
#37195,#37196,#37197,#37198,#37199,#37200,#37201,#37202,#37203,#37204,#37205,
#37206,#37207,#37208,#37209,#37210,#37211,#37212,#37213,#37214,#37215,#37216,
#37217,#37218,#37219,#37220,#37221,#37222,#37223,#37224,#37225,#37226,#37227,
#37228,#37229,#37230,#37231,#37232,#37233,#37234,#37235,#37236,#37237,#37238,
#37239,#37240,#37241,#37242,#37243,#37244,#37245,#37246,#37247,#37248,#37249,
#37250,#37251,#37252,#37253,#37254,#37255,#37256,#37257,#37258,#37259,#37260,
#37261,#37262,#37263,#37264,#37265,#37266,#37267,#37268,#37269,#37270,#37271,
#37272,#37273,#37274,#37275,#37276,#37277,#37278,#37279),(#37280,#37281,
#37282,#37283,#37284,#37285,#37286,#37287,#37288,#37289,#37290,#37291,#37292,
#37293,#37294,#37295,#37296,#37297,#37298,#37299,#37300,#37301,#37302,#37303,
#37304,#37305,#37306,#37307,#37308,#37309,#37310,#37311,#37312,#37313,#37314,
#37315,#37316,#37317,#37318,#37319,#37320,#37321,#37322,#37323,#37324,#37325,
#37326,#37327,#37328,#37329,#37330,#37331,#37332,#37333,#37334,#37335,#37336,
#37337,#37338,#37339,#37340,#37341,#37342,#37343,#37344,#37345,#37346,#37347,
#37348,#37349,#37350,#37351,#37352,#37353,#37354,#37355,#37356,#37357,#37358,
#37359,#37360,#37361,#37362,#37363,#37364,#37365,#37366,#37367,#37368,#37369,
#37370,#37371,#37372,#37373,#37374,#37375,#37376,#37377,#37378,#37379,#37380,
#37381,#37382,#37383,#37384,#37385,#37386,#37387,#37388,#37389,#37390,#37391,
#37392,#37393,#37394,#37395,#37396,#37397,#37398,#37399,#37400,#37401,#37402,
#37403,#37404,#37405,#37406,#37407,#37408,#37409,#37410,#37411,#37412,#37413,
#37414,#37415,#37416,#37417,#37418,#37419,#37420,#37421,#37422,#37423,#37424,
#37425,#37426,#37427,#37428,#37429,#37430,#37431,#37432,#37433,#37434,#37435,
#37436,#37437,#37438,#37439,#37440,#37441,#37442,#37443,#37444,#37445,#37446,
#37447,#37448,#37449,#37450,#37451,#37452,#37453,#37454,#37455,#37456,#37457,
#37458,#37459,#37460,#37461,#37462,#37463,#37464,#37465,#37466,#37467,#37468,
#37469,#37470,#37471,#37472,#37473,#37474,#37475,#37476,#37477,#37478,#37479,
#37480,#37481,#37482,#37483,#37484,#37485,#37486,#37487,#37488,#37489,#37490,
#37491,#37492,#37493,#37494,#37495,#37496,#37497,#37498,#37499,#37500,#37501,
#37502,#37503,#37504,#37505,#37506,#37507,#37508,#37509,#37510,#37511,#37512,
#37513,#37514,#37515,#37516,#37517,#37518,#37519,#37520,#37521,#37522,#37523,
#37524,#37525,#37526,#37527,#37528,#37529,#37530,#37531,#37532,#37533,#37534,
#37535,#37536,#37537,#37538,#37539,#37540,#37541,#37542,#37543,#37544,#37545,
#37546,#37547,#37548,#37549,#37550,#37551,#37552,#37553,#37554,#37555,#37556,
#37557,#37558,#37559,#37560,#37561,#37562,#37563,#37564,#37565,#37566,#37567,
#37568,#37569,#37570,#37571,#37572,#37573,#37574,#37575,#37576,#37577,#37578,
#37579,#37580,#37581,#37582,#37583,#37584,#37585,#37586,#37587,#37588,#37589,
#37590,#37591,#37592,#37593,#37594,#37595,#37596,#37597,#37598,#37599,#37600,
#37601,#37602,#37603,#37604,#37605,#37606,#37607,#37608,#37609,#37610,#37611,
#37612,#37613,#37614,#37615,#37616,#37617,#37618,#37619,#37620,#37621,#37622,
#37623,#37624,#37625,#37626,#37627,#37628,#37629,#37630,#37631,#37632,#37633,
#37634,#37635,#37636,#37637,#37638,#37639,#37640,#37641,#37642,#37643,#37644,
#37645,#37646,#37647,#37648,#37649,#37650,#37651,#37652,#37653,#37654,#37655,
#37656,#37657,#37658,#37659,#37660,#37661,#37662,#37663,#37664,#37665,#37666,
#37667,#37668,#37669,#37670,#37671,#37672,#37673,#37674,#37675,#37676,#37677,
#37678,#37679,#37680,#37681,#37682,#37683,#37684,#37685,#37686,#37687,#37688,
#37689,#37690,#37691,#37692,#37693,#37694,#37695,#37696,#37697,#37698,#37699,
#37700,#37701,#37702,#37703,#37704,#37705,#37706,#37707,#37708,#37709,#37710,
#37711,#37712,#37713,#37714,#37715,#37716,#37717,#37718,#37719,#37720,#37721,
#37722,#37723,#37724,#37725,#37726,#37727,#37728,#37729,#37730,#37731,#37732,
#37733,#37734,#37735,#37736,#37737,#37738,#37739,#37740,#37741,#37742,#37743,
#37744,#37745,#37746,#37747,#37748,#37749,#37750,#37751,#37752,#37753,#37754,
#37755,#37756,#37757,#37758,#37759,#37760,#37761,#37762,#37763,#37764,#37765,
#37766,#37767,#37768,#37769,#37770,#37771,#37772,#37773,#37774,#37775,#37776,
#37777,#37778,#37779,#37780,#37781,#37782,#37783,#37784,#37785,#37786,#37787,
#37788,#37789,#37790,#37791,#37792)),.UNSPECIFIED.,.F.,.F.,.F.,(4,4),(4,
1,1,1,1,1,1,1,1,1,1,1,1,1,1,1,1,1,1,1,1,1,1,1,1,1,1,1,1,1,1,1,1,1,1,1,1,
1,1,1,1,1,1,1,1,1,1,1,1,1,1,1,1,1,1,1,1,1,1,1,1,1,1,1,1,1,1,1,1,1,1,1,1,
1,1,1,1,1,1,1,1,1,1,1,1,1,1,1,1,1,1,1,1,1,1,1,1,1,1,1,1,1,1,1,1,1,1,1,1,
1,1,1,1,1,1,1,1,1,1,1,1,1,1,1,1,1,1,1,1,1,1,1,1,1,1,1,1,1,1,1,1,1,1,1,1,
1,1,1,1,1,1,1,1,1,1,1,1,1,1,1,1,1,1,1,1,1,1,1,1,1,1,1,1,1,1,1,1,1,1,1,1,
1,1,1,1,1,1,1,1,1,1,1,1,1,1,1,1,1,1,1,1,1,1,1,1,1,1,1,1,1,1,1,1,1,1,1,1,
1,1,1,1,1,1,1,1,1,1,1,1,1,1,1,1,1,1,1,1,1,1,1,1,1,1,1,1,1,1,1,1,1,1,1,1,
1,1,1,1,1,1,1,1,1,1,1,1,1,1,1,1,1,1,1,1,1,1,1,1,1,1,1,1,1,1,1,1,1,1,1,1,
1,1,1,1,1,1,1,1,1,1,1,1,1,1,1,1,1,1,1,1,1,1,1,1,1,1,1,1,1,1,1,1,1,1,1,1,
1,1,1,1,1,1,1,1,1,1,1,1,1,1,1,1,1,1,1,1,1,1,1,1,1,1,1,1,1,1,1,1,1,1,1,1,
1,1,1,1,1,1,1,1,1,1,1,1,1,1,1,1,1,1,1,1,1,1,1,1,1,1,1,1,1,1,1,1,1,1,1,1,
1,1,1,1,1,1,1,1,1,1,1,1,1,1,1,1,1,1,1,1,1,1,1,1,1,1,1,1,1,1,1,1,1,1,1,1,
1,1,1,1,1,1,1,1,1,1,1,1,1,1,1,1,1,1,1,1,1,1,1,1,1,1,1,1,1,1,1,1,1,1,1,1,
1,1,1,1,1,1,1,1,1,1,1,1,1,1,1,1,1,1,1,1,1,1,1,1,1,1,1,1,1,1,1,1,1,1,1,1,
1,1,1,1,1,4),(0.,0.082416750926819),(11.1008888355104,11.5998029140446,
12.0987169925787,12.5976310711128,13.096545149647,14.0943733067152,15.0922014637835,
16.0900296208517,16.5889436993859,17.08785777792,17.5867718564541,18.0856859349882,
19.0835140920565,20.0813422491248,21.079170406193,22.0769985632613,23.0748267203295,
23.5737407988637,24.0726548773978,24.5715689559319,25.070483034466,26.0683111915343,
27.0661393486026,28.0639675056708,29.0617956627391,30.0596238198073,30.5585378983415,
31.0574519768756,31.5563660554097,32.0552801339438,33.0531082910121,34.0509364480804,
35.0487646051486,36.0465927622169,37.0444209192851,37.5433349978193,38.0422490763534,
38.5411631548875,39.0400772334217,40.0379053904899,41.0357335475582,42.0335617046264,
43.0313898616947,44.0292180187629,44.5281320972971,45.0270461758312,45.5259602543653,
46.0248743328995,47.0227024899677,48.020530647036,49.0183588041042,50.0161869611725,
51.0140151182407,51.5129291967749,52.011843275309,52.5107573538431,53.0096714323773,
54.0074995894455,55.0053277465138,56.003155903582,57.0009840606503,57.9988122177186,
58.4977262962527,58.9966403747868,59.4955544533209,59.9944685318551,60.9922966889233,
61.9901248459916,62.9879530030598,63.9857811601281,64.9836093171964,65.4825233957305,
65.9814374742646,66.4803515527987,66.9792656313329,67.9770937884011,68.9749219454694,
69.9727501025376,70.9705782596059,71.9684064166742,72.4673204952083,72.9662345737424,
73.4651486522765,73.9640627308107,74.9618908878789,75.9597190449472,76.9575472020154,
77.9553753590837,78.953203516152,79.4521175946861,79.9510316732202,80.4499457517543,
80.9488598302885,81.9466879873567,82.944516144425,83.9423443014932,84.9401724585615,
85.9380006156298,86.4369146941639,86.935828772698,87.4347428512321,87.9336569297663,
88.9314850868345,89.9293132439028,90.927141400971,91.9249695580393,92.9227977151076,
93.4217117936417,93.9206258721758,94.4195399507099,94.9184540292441,95.9162821863123,
96.9141103433806,97.9119385004489,98.9097666575171,99.9075948145854,100.406508893119,
100.905422971654,101.404337050188,101.903251128722,102.90107928579,103.898907442858,
104.896735599927,105.894563756995,106.892391914063,107.391305992597,107.890220071131,
108.389134149666,108.8880482282,109.885876385268,110.883704542336,111.881532699404,
112.879360856473,113.877189013541,114.376103092075,114.875017170609,115.373931249143,
115.872845327677,116.870673484746,117.868501641814,118.866329798882,119.864157955951,
120.861986113019,121.360900191553,121.859814270087,122.358728348621,122.857642427155,
123.855470584224,124.853298741292,125.85112689836,126.848955055428,127.846783212497,
128.345697291031,128.844611369565,129.343525448099,129.842439526633,130.840267683701,
131.83809584077,132.835923997838,133.833752154906,134.831580311974,135.330494390509,
135.829408469043,136.328322547577,136.827236626111,137.825064783179,138.822892940247,
139.820721097316,140.818549254384,141.816377411452,142.315291489986,142.81420556852,
143.313119647055,143.812033725589,144.809861882657,145.807690039725,146.805518196793,
147.803346353862,148.80117451093,149.300088589464,149.799002667998,150.297916746532,
150.796830825067,151.794658982135,152.792487139203,153.790315296271,154.78814345334,
155.785971610408,156.284885688942,156.783799767476,157.28271384601,157.781627924544,
158.779456081613,159.777284238681,160.775112395749,161.772940552817,162.770768709886,
163.26968278842,163.768596866954,164.267510945488,164.766425024022,165.76425318109,
166.762081338159,167.759909495227,168.757737652295,169.755565809363,170.254479887898,
170.753393966432,171.252308044966,171.7512221235,172.749050280568,173.746878437636,
174.744706594705,175.742534751773,176.740362908841,177.239276987375,177.738191065909,
178.237105144444,178.736019222978,179.733847380046,180.731675537114,181.729503694182,
182.727331851251,183.725160008319,184.224074086853,184.722988165387,185.221902243921,
185.720816322456,186.718644479524,187.716472636592,188.71430079366,189.712128950729,
190.709957107797,191.208871186331,191.707785264865,192.206699343399,192.705613421933,
193.703441579002,194.70126973607,195.699097893138,196.696926050206,197.694754207275,
198.193668285809,198.692582364343,199.191496442877,199.690410521411,200.688238678479,
201.686066835548,202.683894992616,203.681723149684,204.679551306752,205.178465385287,
205.677379463821,206.176293542355,206.675207620889,207.673035777957,208.670863935025,
209.668692092094,210.666520249162,211.66434840623,212.662176563298,213.161090641833,
213.660004720367,214.657832877435,215.655661034503,216.653489191572,217.152403270106,
217.65131734864,218.150231427174,218.649145505708,219.646973662776,220.644801819845,
221.642629976913,222.640458133981,223.638286291049,224.137200369583,224.636114448118,
225.135028526652,225.633942605186,226.631770762254,227.629598919322,228.627427076391,
229.625255233459,230.623083390527,231.121997469061,231.620911547595,232.11982562613,
232.618739704664,233.616567861732,234.6143960188,235.612224175868,236.610052332937,
237.607880490005,238.106794568539,238.605708647073,239.104622725607,239.603536804141,
240.60136496121,241.599193118278,242.597021275346,243.594849432414,244.592677589483,
245.091591668017,245.590505746551,246.089419825085,246.588333903619,247.586162060688,
248.583990217756,249.581818374824,250.579646531892,251.577474688961,252.076388767495,
252.575302846029,253.074216924563,253.573131003097,254.570959160165,255.568787317234,
256.566615474302,257.56444363137,258.562271788438,259.061185866972,259.560099945507,
260.059014024041,260.557928102575,261.555756259643,262.553584416711,263.55141257378,
264.549240730848,265.547068887916,266.04598296645,266.544897044984,267.043811123519,
267.542725202053,268.540553359121,269.538381516189,270.536209673257,271.534037830326,
272.531865987394,273.030780065928,273.529694144462,274.028608222996,274.52752230153,
275.525350458599,276.523178615667,277.521006772735,278.518834929803,279.516663086872,
280.015577165406,280.51449124394,281.013405322474,281.512319401008,282.510147558077,
283.507975715145,284.505803872213,285.503632029281,286.50146018635,287.000374264884,
287.499288343418,287.998202421952,288.497116500486,289.494944657554,290.492772814623,
291.490600971691,292.488429128759,293.486257285827,293.985171364361,294.484085442896,
294.98299952143,295.481913599964,296.479741757032,297.4775699141,298.475398071169,
299.473226228237,300.471054385305,300.969968463839,301.468882542373,301.967796620908,
302.466710699442,303.46453885651,304.462367013578,305.460195170646,306.458023327715,
307.455851484783,307.954765563317,308.453679641851,308.952593720385,309.451507798919,
310.449335955988,311.447164113056,312.444992270124,313.442820427192,314.440648584261,
314.939562662795,315.438476741329,315.937390819863,316.436304898397,317.434133055466,
318.431961212534,319.429789369602,320.42761752667,321.425445683739,321.924359762273,
322.423273840807,322.922187919341,323.421101997875,324.418930154943,325.416758312012,
326.41458646908,327.412414626148,328.410242783216,328.90915686175,329.408070940285,
329.906985018819,330.405899097353,331.403727254421,332.401555411489,333.399383568558,
334.397211725626,335.395039882694,335.893953961228,336.392868039762,336.891782118297,
337.390696196831,338.388524353899,339.386352510967,340.384180668035,341.382008825104,
342.379836982172,342.878751060706,343.37766513924,343.876579217774,344.375493296308,
345.373321453377,346.371149610445,347.368977767513,348.366805924582,349.36463408165,
349.863548160184,350.362462238718,350.861376317252,351.360290395786,352.358118552855,
353.355946709923,354.353774866991,355.351603024059,356.349431181128,356.848345259662,
357.347259338196,357.84617341673,358.345087495264,359.342915652332,360.340743809401,
361.338571966469,362.336400123537,363.334228280605,363.83314235914,364.332056437674,
364.830970516208,365.329884594742,366.32771275181,367.325540908878,368.323369065947,
369.321197223015,370.319025380083,370.817939458617,371.316853537151,371.815767615686,
372.31468169422,373.312509851288,374.310338008356,375.308166165424,376.305994322493,
377.303822479561,377.802736558095,378.301650636629,378.800564715163,379.299478793698,
380.297306950766,381.295135107834,382.292963264902,383.290791421971,384.288619579039,
384.787533657573,385.286447736107,385.785361814641,386.284275893175,387.282104050244,
388.279932207312,389.27776036438,390.275588521448,391.273416678517,391.772330757051,
392.271244835585,392.770158914119,393.269072992653,394.266901149721,395.26472930679,
396.262557463858,397.260385620926,398.258213777994,398.757127856529,399.256041935063,
399.754956013597,400.253870092131,401.251698249199,402.249526406267,403.247354563336,
403.74626864187,404.245182720404,404.744096798938,405.243010877472),
 .UNSPECIFIED.);
#835=B_SPLINE_SURFACE_WITH_KNOTS('',3,3,((#38059,#38060,#38061,#38062,#38063,
#38064,#38065,#38066,#38067,#38068,#38069,#38070,#38071,#38072,#38073,#38074,
#38075,#38076,#38077,#38078,#38079,#38080,#38081,#38082,#38083,#38084,#38085,
#38086,#38087,#38088,#38089,#38090,#38091,#38092,#38093,#38094,#38095,#38096,
#38097,#38098,#38099,#38100,#38101,#38102,#38103,#38104,#38105,#38106,#38107,
#38108,#38109,#38110,#38111,#38112,#38113,#38114,#38115,#38116,#38117,#38118,
#38119,#38120,#38121,#38122,#38123,#38124,#38125,#38126,#38127,#38128,#38129,
#38130,#38131,#38132,#38133,#38134,#38135,#38136,#38137,#38138,#38139,#38140,
#38141,#38142,#38143,#38144,#38145,#38146,#38147,#38148,#38149,#38150,#38151,
#38152,#38153,#38154,#38155,#38156,#38157,#38158,#38159,#38160,#38161,#38162,
#38163,#38164,#38165,#38166,#38167,#38168,#38169,#38170,#38171,#38172,#38173,
#38174,#38175,#38176,#38177,#38178,#38179,#38180,#38181,#38182,#38183,#38184,
#38185,#38186,#38187,#38188,#38189,#38190,#38191,#38192,#38193,#38194,#38195,
#38196,#38197,#38198,#38199,#38200,#38201,#38202,#38203,#38204,#38205,#38206,
#38207,#38208,#38209,#38210,#38211,#38212,#38213,#38214,#38215,#38216,#38217,
#38218,#38219,#38220,#38221,#38222,#38223,#38224,#38225,#38226,#38227,#38228,
#38229,#38230,#38231,#38232,#38233,#38234,#38235,#38236,#38237,#38238,#38239,
#38240,#38241,#38242,#38243,#38244,#38245,#38246,#38247,#38248,#38249,#38250,
#38251,#38252,#38253,#38254,#38255,#38256,#38257,#38258,#38259,#38260,#38261,
#38262,#38263,#38264,#38265,#38266,#38267,#38268,#38269,#38270,#38271,#38272,
#38273,#38274,#38275,#38276,#38277,#38278,#38279,#38280,#38281,#38282,#38283,
#38284,#38285,#38286,#38287,#38288,#38289,#38290,#38291,#38292,#38293,#38294,
#38295,#38296,#38297,#38298,#38299,#38300,#38301,#38302,#38303,#38304,#38305,
#38306,#38307,#38308,#38309,#38310,#38311,#38312,#38313,#38314,#38315,#38316,
#38317,#38318,#38319,#38320,#38321,#38322,#38323,#38324,#38325,#38326,#38327,
#38328,#38329,#38330,#38331,#38332,#38333,#38334,#38335,#38336,#38337,#38338,
#38339,#38340,#38341,#38342,#38343,#38344,#38345,#38346,#38347,#38348,#38349,
#38350,#38351,#38352,#38353,#38354,#38355,#38356,#38357,#38358,#38359,#38360,
#38361,#38362,#38363,#38364,#38365,#38366,#38367,#38368,#38369,#38370,#38371,
#38372,#38373,#38374,#38375,#38376,#38377,#38378,#38379,#38380,#38381,#38382,
#38383,#38384,#38385,#38386,#38387,#38388,#38389,#38390,#38391,#38392,#38393,
#38394,#38395,#38396,#38397,#38398,#38399,#38400,#38401,#38402,#38403,#38404,
#38405,#38406,#38407,#38408,#38409,#38410,#38411,#38412,#38413,#38414,#38415,
#38416,#38417,#38418,#38419,#38420,#38421,#38422,#38423,#38424,#38425,#38426,
#38427,#38428,#38429,#38430,#38431,#38432,#38433,#38434,#38435,#38436,#38437,
#38438,#38439,#38440,#38441,#38442,#38443,#38444,#38445,#38446,#38447,#38448,
#38449,#38450,#38451,#38452,#38453,#38454,#38455,#38456,#38457,#38458,#38459,
#38460,#38461,#38462,#38463,#38464,#38465,#38466,#38467,#38468,#38469,#38470,
#38471,#38472,#38473,#38474,#38475,#38476,#38477,#38478,#38479,#38480,#38481,
#38482,#38483,#38484,#38485,#38486,#38487,#38488,#38489,#38490,#38491,#38492,
#38493,#38494,#38495,#38496,#38497,#38498,#38499,#38500,#38501,#38502,#38503,
#38504,#38505,#38506,#38507,#38508,#38509,#38510,#38511,#38512,#38513,#38514,
#38515,#38516,#38517,#38518,#38519,#38520,#38521,#38522,#38523,#38524,#38525,
#38526,#38527,#38528,#38529,#38530,#38531,#38532,#38533,#38534,#38535,#38536,
#38537,#38538,#38539,#38540,#38541,#38542,#38543,#38544,#38545,#38546,#38547,
#38548,#38549,#38550,#38551,#38552,#38553,#38554,#38555,#38556,#38557,#38558,
#38559,#38560,#38561,#38562,#38563,#38564,#38565,#38566,#38567,#38568,#38569,
#38570,#38571),(#38572,#38573,#38574,#38575,#38576,#38577,#38578,#38579,
#38580,#38581,#38582,#38583,#38584,#38585,#38586,#38587,#38588,#38589,#38590,
#38591,#38592,#38593,#38594,#38595,#38596,#38597,#38598,#38599,#38600,#38601,
#38602,#38603,#38604,#38605,#38606,#38607,#38608,#38609,#38610,#38611,#38612,
#38613,#38614,#38615,#38616,#38617,#38618,#38619,#38620,#38621,#38622,#38623,
#38624,#38625,#38626,#38627,#38628,#38629,#38630,#38631,#38632,#38633,#38634,
#38635,#38636,#38637,#38638,#38639,#38640,#38641,#38642,#38643,#38644,#38645,
#38646,#38647,#38648,#38649,#38650,#38651,#38652,#38653,#38654,#38655,#38656,
#38657,#38658,#38659,#38660,#38661,#38662,#38663,#38664,#38665,#38666,#38667,
#38668,#38669,#38670,#38671,#38672,#38673,#38674,#38675,#38676,#38677,#38678,
#38679,#38680,#38681,#38682,#38683,#38684,#38685,#38686,#38687,#38688,#38689,
#38690,#38691,#38692,#38693,#38694,#38695,#38696,#38697,#38698,#38699,#38700,
#38701,#38702,#38703,#38704,#38705,#38706,#38707,#38708,#38709,#38710,#38711,
#38712,#38713,#38714,#38715,#38716,#38717,#38718,#38719,#38720,#38721,#38722,
#38723,#38724,#38725,#38726,#38727,#38728,#38729,#38730,#38731,#38732,#38733,
#38734,#38735,#38736,#38737,#38738,#38739,#38740,#38741,#38742,#38743,#38744,
#38745,#38746,#38747,#38748,#38749,#38750,#38751,#38752,#38753,#38754,#38755,
#38756,#38757,#38758,#38759,#38760,#38761,#38762,#38763,#38764,#38765,#38766,
#38767,#38768,#38769,#38770,#38771,#38772,#38773,#38774,#38775,#38776,#38777,
#38778,#38779,#38780,#38781,#38782,#38783,#38784,#38785,#38786,#38787,#38788,
#38789,#38790,#38791,#38792,#38793,#38794,#38795,#38796,#38797,#38798,#38799,
#38800,#38801,#38802,#38803,#38804,#38805,#38806,#38807,#38808,#38809,#38810,
#38811,#38812,#38813,#38814,#38815,#38816,#38817,#38818,#38819,#38820,#38821,
#38822,#38823,#38824,#38825,#38826,#38827,#38828,#38829,#38830,#38831,#38832,
#38833,#38834,#38835,#38836,#38837,#38838,#38839,#38840,#38841,#38842,#38843,
#38844,#38845,#38846,#38847,#38848,#38849,#38850,#38851,#38852,#38853,#38854,
#38855,#38856,#38857,#38858,#38859,#38860,#38861,#38862,#38863,#38864,#38865,
#38866,#38867,#38868,#38869,#38870,#38871,#38872,#38873,#38874,#38875,#38876,
#38877,#38878,#38879,#38880,#38881,#38882,#38883,#38884,#38885,#38886,#38887,
#38888,#38889,#38890,#38891,#38892,#38893,#38894,#38895,#38896,#38897,#38898,
#38899,#38900,#38901,#38902,#38903,#38904,#38905,#38906,#38907,#38908,#38909,
#38910,#38911,#38912,#38913,#38914,#38915,#38916,#38917,#38918,#38919,#38920,
#38921,#38922,#38923,#38924,#38925,#38926,#38927,#38928,#38929,#38930,#38931,
#38932,#38933,#38934,#38935,#38936,#38937,#38938,#38939,#38940,#38941,#38942,
#38943,#38944,#38945,#38946,#38947,#38948,#38949,#38950,#38951,#38952,#38953,
#38954,#38955,#38956,#38957,#38958,#38959,#38960,#38961,#38962,#38963,#38964,
#38965,#38966,#38967,#38968,#38969,#38970,#38971,#38972,#38973,#38974,#38975,
#38976,#38977,#38978,#38979,#38980,#38981,#38982,#38983,#38984,#38985,#38986,
#38987,#38988,#38989,#38990,#38991,#38992,#38993,#38994,#38995,#38996,#38997,
#38998,#38999,#39000,#39001,#39002,#39003,#39004,#39005,#39006,#39007,#39008,
#39009,#39010,#39011,#39012,#39013,#39014,#39015,#39016,#39017,#39018,#39019,
#39020,#39021,#39022,#39023,#39024,#39025,#39026,#39027,#39028,#39029,#39030,
#39031,#39032,#39033,#39034,#39035,#39036,#39037,#39038,#39039,#39040,#39041,
#39042,#39043,#39044,#39045,#39046,#39047,#39048,#39049,#39050,#39051,#39052,
#39053,#39054,#39055,#39056,#39057,#39058,#39059,#39060,#39061,#39062,#39063,
#39064,#39065,#39066,#39067,#39068,#39069,#39070,#39071,#39072,#39073,#39074,
#39075,#39076,#39077,#39078,#39079,#39080,#39081,#39082,#39083,#39084),
(#39085,#39086,#39087,#39088,#39089,#39090,#39091,#39092,#39093,#39094,
#39095,#39096,#39097,#39098,#39099,#39100,#39101,#39102,#39103,#39104,#39105,
#39106,#39107,#39108,#39109,#39110,#39111,#39112,#39113,#39114,#39115,#39116,
#39117,#39118,#39119,#39120,#39121,#39122,#39123,#39124,#39125,#39126,#39127,
#39128,#39129,#39130,#39131,#39132,#39133,#39134,#39135,#39136,#39137,#39138,
#39139,#39140,#39141,#39142,#39143,#39144,#39145,#39146,#39147,#39148,#39149,
#39150,#39151,#39152,#39153,#39154,#39155,#39156,#39157,#39158,#39159,#39160,
#39161,#39162,#39163,#39164,#39165,#39166,#39167,#39168,#39169,#39170,#39171,
#39172,#39173,#39174,#39175,#39176,#39177,#39178,#39179,#39180,#39181,#39182,
#39183,#39184,#39185,#39186,#39187,#39188,#39189,#39190,#39191,#39192,#39193,
#39194,#39195,#39196,#39197,#39198,#39199,#39200,#39201,#39202,#39203,#39204,
#39205,#39206,#39207,#39208,#39209,#39210,#39211,#39212,#39213,#39214,#39215,
#39216,#39217,#39218,#39219,#39220,#39221,#39222,#39223,#39224,#39225,#39226,
#39227,#39228,#39229,#39230,#39231,#39232,#39233,#39234,#39235,#39236,#39237,
#39238,#39239,#39240,#39241,#39242,#39243,#39244,#39245,#39246,#39247,#39248,
#39249,#39250,#39251,#39252,#39253,#39254,#39255,#39256,#39257,#39258,#39259,
#39260,#39261,#39262,#39263,#39264,#39265,#39266,#39267,#39268,#39269,#39270,
#39271,#39272,#39273,#39274,#39275,#39276,#39277,#39278,#39279,#39280,#39281,
#39282,#39283,#39284,#39285,#39286,#39287,#39288,#39289,#39290,#39291,#39292,
#39293,#39294,#39295,#39296,#39297,#39298,#39299,#39300,#39301,#39302,#39303,
#39304,#39305,#39306,#39307,#39308,#39309,#39310,#39311,#39312,#39313,#39314,
#39315,#39316,#39317,#39318,#39319,#39320,#39321,#39322,#39323,#39324,#39325,
#39326,#39327,#39328,#39329,#39330,#39331,#39332,#39333,#39334,#39335,#39336,
#39337,#39338,#39339,#39340,#39341,#39342,#39343,#39344,#39345,#39346,#39347,
#39348,#39349,#39350,#39351,#39352,#39353,#39354,#39355,#39356,#39357,#39358,
#39359,#39360,#39361,#39362,#39363,#39364,#39365,#39366,#39367,#39368,#39369,
#39370,#39371,#39372,#39373,#39374,#39375,#39376,#39377,#39378,#39379,#39380,
#39381,#39382,#39383,#39384,#39385,#39386,#39387,#39388,#39389,#39390,#39391,
#39392,#39393,#39394,#39395,#39396,#39397,#39398,#39399,#39400,#39401,#39402,
#39403,#39404,#39405,#39406,#39407,#39408,#39409,#39410,#39411,#39412,#39413,
#39414,#39415,#39416,#39417,#39418,#39419,#39420,#39421,#39422,#39423,#39424,
#39425,#39426,#39427,#39428,#39429,#39430,#39431,#39432,#39433,#39434,#39435,
#39436,#39437,#39438,#39439,#39440,#39441,#39442,#39443,#39444,#39445,#39446,
#39447,#39448,#39449,#39450,#39451,#39452,#39453,#39454,#39455,#39456,#39457,
#39458,#39459,#39460,#39461,#39462,#39463,#39464,#39465,#39466,#39467,#39468,
#39469,#39470,#39471,#39472,#39473,#39474,#39475,#39476,#39477,#39478,#39479,
#39480,#39481,#39482,#39483,#39484,#39485,#39486,#39487,#39488,#39489,#39490,
#39491,#39492,#39493,#39494,#39495,#39496,#39497,#39498,#39499,#39500,#39501,
#39502,#39503,#39504,#39505,#39506,#39507,#39508,#39509,#39510,#39511,#39512,
#39513,#39514,#39515,#39516,#39517,#39518,#39519,#39520,#39521,#39522,#39523,
#39524,#39525,#39526,#39527,#39528,#39529,#39530,#39531,#39532,#39533,#39534,
#39535,#39536,#39537,#39538,#39539,#39540,#39541,#39542,#39543,#39544,#39545,
#39546,#39547,#39548,#39549,#39550,#39551,#39552,#39553,#39554,#39555,#39556,
#39557,#39558,#39559,#39560,#39561,#39562,#39563,#39564,#39565,#39566,#39567,
#39568,#39569,#39570,#39571,#39572,#39573,#39574,#39575,#39576,#39577,#39578,
#39579,#39580,#39581,#39582,#39583,#39584,#39585,#39586,#39587,#39588,#39589,
#39590,#39591,#39592,#39593,#39594,#39595,#39596,#39597),(#39598,#39599,
#39600,#39601,#39602,#39603,#39604,#39605,#39606,#39607,#39608,#39609,#39610,
#39611,#39612,#39613,#39614,#39615,#39616,#39617,#39618,#39619,#39620,#39621,
#39622,#39623,#39624,#39625,#39626,#39627,#39628,#39629,#39630,#39631,#39632,
#39633,#39634,#39635,#39636,#39637,#39638,#39639,#39640,#39641,#39642,#39643,
#39644,#39645,#39646,#39647,#39648,#39649,#39650,#39651,#39652,#39653,#39654,
#39655,#39656,#39657,#39658,#39659,#39660,#39661,#39662,#39663,#39664,#39665,
#39666,#39667,#39668,#39669,#39670,#39671,#39672,#39673,#39674,#39675,#39676,
#39677,#39678,#39679,#39680,#39681,#39682,#39683,#39684,#39685,#39686,#39687,
#39688,#39689,#39690,#39691,#39692,#39693,#39694,#39695,#39696,#39697,#39698,
#39699,#39700,#39701,#39702,#39703,#39704,#39705,#39706,#39707,#39708,#39709,
#39710,#39711,#39712,#39713,#39714,#39715,#39716,#39717,#39718,#39719,#39720,
#39721,#39722,#39723,#39724,#39725,#39726,#39727,#39728,#39729,#39730,#39731,
#39732,#39733,#39734,#39735,#39736,#39737,#39738,#39739,#39740,#39741,#39742,
#39743,#39744,#39745,#39746,#39747,#39748,#39749,#39750,#39751,#39752,#39753,
#39754,#39755,#39756,#39757,#39758,#39759,#39760,#39761,#39762,#39763,#39764,
#39765,#39766,#39767,#39768,#39769,#39770,#39771,#39772,#39773,#39774,#39775,
#39776,#39777,#39778,#39779,#39780,#39781,#39782,#39783,#39784,#39785,#39786,
#39787,#39788,#39789,#39790,#39791,#39792,#39793,#39794,#39795,#39796,#39797,
#39798,#39799,#39800,#39801,#39802,#39803,#39804,#39805,#39806,#39807,#39808,
#39809,#39810,#39811,#39812,#39813,#39814,#39815,#39816,#39817,#39818,#39819,
#39820,#39821,#39822,#39823,#39824,#39825,#39826,#39827,#39828,#39829,#39830,
#39831,#39832,#39833,#39834,#39835,#39836,#39837,#39838,#39839,#39840,#39841,
#39842,#39843,#39844,#39845,#39846,#39847,#39848,#39849,#39850,#39851,#39852,
#39853,#39854,#39855,#39856,#39857,#39858,#39859,#39860,#39861,#39862,#39863,
#39864,#39865,#39866,#39867,#39868,#39869,#39870,#39871,#39872,#39873,#39874,
#39875,#39876,#39877,#39878,#39879,#39880,#39881,#39882,#39883,#39884,#39885,
#39886,#39887,#39888,#39889,#39890,#39891,#39892,#39893,#39894,#39895,#39896,
#39897,#39898,#39899,#39900,#39901,#39902,#39903,#39904,#39905,#39906,#39907,
#39908,#39909,#39910,#39911,#39912,#39913,#39914,#39915,#39916,#39917,#39918,
#39919,#39920,#39921,#39922,#39923,#39924,#39925,#39926,#39927,#39928,#39929,
#39930,#39931,#39932,#39933,#39934,#39935,#39936,#39937,#39938,#39939,#39940,
#39941,#39942,#39943,#39944,#39945,#39946,#39947,#39948,#39949,#39950,#39951,
#39952,#39953,#39954,#39955,#39956,#39957,#39958,#39959,#39960,#39961,#39962,
#39963,#39964,#39965,#39966,#39967,#39968,#39969,#39970,#39971,#39972,#39973,
#39974,#39975,#39976,#39977,#39978,#39979,#39980,#39981,#39982,#39983,#39984,
#39985,#39986,#39987,#39988,#39989,#39990,#39991,#39992,#39993,#39994,#39995,
#39996,#39997,#39998,#39999,#40000,#40001,#40002,#40003,#40004,#40005,#40006,
#40007,#40008,#40009,#40010,#40011,#40012,#40013,#40014,#40015,#40016,#40017,
#40018,#40019,#40020,#40021,#40022,#40023,#40024,#40025,#40026,#40027,#40028,
#40029,#40030,#40031,#40032,#40033,#40034,#40035,#40036,#40037,#40038,#40039,
#40040,#40041,#40042,#40043,#40044,#40045,#40046,#40047,#40048,#40049,#40050,
#40051,#40052,#40053,#40054,#40055,#40056,#40057,#40058,#40059,#40060,#40061,
#40062,#40063,#40064,#40065,#40066,#40067,#40068,#40069,#40070,#40071,#40072,
#40073,#40074,#40075,#40076,#40077,#40078,#40079,#40080,#40081,#40082,#40083,
#40084,#40085,#40086,#40087,#40088,#40089,#40090,#40091,#40092,#40093,#40094,
#40095,#40096,#40097,#40098,#40099,#40100,#40101,#40102,#40103,#40104,#40105,
#40106,#40107,#40108,#40109,#40110)),.UNSPECIFIED.,.F.,.F.,.F.,(4,4),(4,
1,1,1,1,1,1,1,1,1,1,1,1,1,1,1,1,1,1,1,1,1,1,1,1,1,1,1,1,1,1,1,1,1,1,1,1,
1,1,1,1,1,1,1,1,1,1,1,1,1,1,1,1,1,1,1,1,1,1,1,1,1,1,1,1,1,1,1,1,1,1,1,1,
1,1,1,1,1,1,1,1,1,1,1,1,1,1,1,1,1,1,1,1,1,1,1,1,1,1,1,1,1,1,1,1,1,1,1,1,
1,1,1,1,1,1,1,1,1,1,1,1,1,1,1,1,1,1,1,1,1,1,1,1,1,1,1,1,1,1,1,1,1,1,1,1,
1,1,1,1,1,1,1,1,1,1,1,1,1,1,1,1,1,1,1,1,1,1,1,1,1,1,1,1,1,1,1,1,1,1,1,1,
1,1,1,1,1,1,1,1,1,1,1,1,1,1,1,1,1,1,1,1,1,1,1,1,1,1,1,1,1,1,1,1,1,1,1,1,
1,1,1,1,1,1,1,1,1,1,1,1,1,1,1,1,1,1,1,1,1,1,1,1,1,1,1,1,1,1,1,1,1,1,1,1,
1,1,1,1,1,1,1,1,1,1,1,1,1,1,1,1,1,1,1,1,1,1,1,1,1,1,1,1,1,1,1,1,1,1,1,1,
1,1,1,1,1,1,1,1,1,1,1,1,1,1,1,1,1,1,1,1,1,1,1,1,1,1,1,1,1,1,1,1,1,1,1,1,
1,1,1,1,1,1,1,1,1,1,1,1,1,1,1,1,1,1,1,1,1,1,1,1,1,1,1,1,1,1,1,1,1,1,1,1,
1,1,1,1,1,1,1,1,1,1,1,1,1,1,1,1,1,1,1,1,1,1,1,1,1,1,1,1,1,1,1,1,1,1,1,1,
1,1,1,1,1,1,1,1,1,1,1,1,1,1,1,1,1,1,1,1,1,1,1,1,1,1,1,1,1,1,1,1,1,1,1,1,
1,1,1,1,1,1,1,1,1,1,1,1,1,1,1,1,1,1,1,1,1,1,1,1,1,1,1,1,1,1,1,1,1,1,1,1,
1,1,1,1,1,1,1,1,1,1,1,1,1,1,1,1,1,1,1,1,1,1,1,1,1,1,1,1,1,1,1,1,1,1,1,1,
1,1,1,1,1,4),(0.,0.082416750926819),(14.4112373819487,14.9101514604828,
15.4090655390169,15.9079796175511,16.4068936960852,17.4047218531535,18.4025500102217,
19.40037816729,19.8992922458241,20.3982063243582,20.8971204028924,21.3960344814265,
22.3938626384947,23.391690795563,24.3895189526313,25.3873471096995,26.3851752667678,
26.8840893453019,27.383003423836,27.8819175023702,28.3808315809043,29.3786597379725,
30.3764878950408,31.3743160521091,32.3721442091773,33.3699723662456,33.8688864447797,
34.3678005233138,34.866714601848,35.3656286803821,36.3634568374504,37.3612849945186,
38.3591131515869,39.3569413086551,40.3547694657234,40.8536835442575,41.3525976227916,
41.8515117013258,42.3504257798599,43.3482539369282,44.3460820939964,45.3439102510647,
46.3417384081329,47.3395665652012,47.8384806437353,48.3373947222694,48.8363088008036,
49.3352228793377,50.333051036406,51.3308791934742,52.3287073505425,53.3265355076107,
54.324363664679,54.8232777432131,55.3221918217472,55.8211059002814,56.3200199788155,
57.3178481358838,58.315676292952,59.3135044500203,60.3113326070885,61.3091607641568,
61.8080748426909,62.306988921225,62.8059029997592,63.3048170782933,64.3026452353616,
65.3004733924298,66.2983015494981,67.2961297065663,68.2939578636346,68.7928719421687,
69.2917860207028,69.790700099237,70.2896141777711,71.2874423348394,72.2852704919076,
73.2830986489759,74.2809268060441,75.2787549631124,75.7776690416465,76.2765831201806,
76.7754971987148,77.2744112772489,78.2722394343172,79.2700675913854,80.2678957484537,
81.2657239055219,82.2635520625902,82.7624661411243,83.2613802196584,83.7602942981926,
84.2592083767267,85.257036533795,86.2548646908632,87.2526928479315,88.2505210049997,
89.248349162068,89.7472632406021,90.2461773191363,90.7450913976704,91.2440054762045,
92.2418336332728,93.239661790341,94.2374899474093,95.2353181044775,96.2331462615458,
96.7320603400799,97.2309744186141,97.7298884971482,98.2288025756823,99.2266307327506,
100.224458889819,101.222287046887,102.220115203955,103.217943361024,103.716857439558,
104.215771518092,104.714685596626,105.21359967516,106.211427832228,107.209255989297,
108.207084146365,109.204912303433,110.202740460501,110.701654539036,111.20056861757,
111.699482696104,112.198396774638,113.196224931706,114.194053088774,115.191881245843,
116.189709402911,117.187537559979,117.686451638513,118.185365717047,118.684279795582,
119.183193874116,120.181022031184,121.178850188252,122.17667834532,123.174506502389,
124.172334659457,124.671248737991,125.170162816525,125.669076895059,126.167990973594,
127.165819130662,128.16364728773,129.161475444798,130.159303601867,131.157131758935,
131.656045837469,132.154959916003,132.653873994537,133.152788073071,134.15061623014,
135.148444387208,136.146272544276,137.144100701344,138.141928858413,138.640842936947,
139.139757015481,139.638671094015,140.137585172549,141.135413329617,142.133241486686,
143.131069643754,144.128897800822,145.12672595789,145.625640036425,146.124554114959,
146.623468193493,147.122382272027,148.120210429095,149.118038586163,150.115866743232,
151.1136949003,152.111523057368,152.610437135902,153.109351214436,153.608265292971,
154.107179371505,155.105007528573,156.102835685641,157.100663842709,158.098491999778,
159.096320156846,159.59523423538,160.094148313914,160.593062392448,161.091976470983,
162.089804628051,163.087632785119,164.085460942187,165.083289099256,166.081117256324,
166.580031334858,167.078945413392,167.577859491926,168.07677357046,169.074601727529,
170.072429884597,171.070258041665,172.068086198733,173.065914355802,173.564828434336,
174.06374251287,174.562656591404,175.061570669938,176.059398827006,177.057226984075,
178.055055141143,179.052883298211,180.050711455279,180.549625533814,181.048539612348,
181.547453690882,182.046367769416,183.044195926484,184.042024083552,185.039852240621,
186.037680397689,187.035508554757,187.534422633291,188.033336711825,188.53225079036,
189.031164868894,190.028993025962,191.02682118303,192.024649340099,193.022477497167,
194.020305654235,194.519219732769,195.018133811303,195.517047889837,196.015961968372,
197.01379012544,198.011618282508,199.009446439576,200.007274596645,201.005102753713,
201.504016832247,202.002930910781,202.501844989315,203.000759067849,203.998587224918,
204.996415381986,205.994243539054,206.992071696122,207.989899853191,208.488813931725,
208.987728010259,209.486642088793,209.985556167327,210.983384324395,211.981212481464,
212.979040638532,213.9768687956,214.974696952668,215.972525109737,216.471439188271,
216.970353266805,217.968181423873,218.966009580941,219.96383773801,220.462751816544,
220.961665895078,221.460579973612,221.959494052146,222.957322209214,223.955150366283,
224.952978523351,225.950806680419,226.948634837488,227.447548916022,227.946462994556,
228.44537707309,228.944291151624,229.942119308692,230.939947465761,231.937775622829,
232.935603779897,233.933431936965,234.432346015499,234.931260094034,235.430174172568,
235.929088251102,236.92691640817,237.924744565238,238.922572722307,239.920400879375,
240.918229036443,241.417143114977,241.916057193511,242.414971272045,242.91388535058,
243.911713507648,244.909541664716,245.907369821784,246.905197978853,247.903026135921,
248.401940214455,248.900854292989,249.399768371523,249.898682450057,250.896510607126,
251.894338764194,252.892166921262,253.88999507833,254.887823235399,255.386737313933,
255.885651392467,256.384565471001,256.883479549535,257.881307706603,258.879135863672,
259.87696402074,260.874792177808,261.872620334877,262.371534413411,262.870448491945,
263.369362570479,263.868276649013,264.866104806081,265.86393296315,266.861761120218,
267.859589277286,268.857417434354,269.356331512888,269.855245591423,270.354159669957,
270.853073748491,271.850901905559,272.848730062627,273.846558219696,274.844386376764,
275.842214533832,276.341128612366,276.8400426909,277.338956769435,277.837870847969,
278.835699005037,279.833527162105,280.831355319173,281.829183476242,282.82701163331,
283.325925711844,283.824839790378,284.323753868912,284.822667947446,285.820496104515,
286.818324261583,287.816152418651,288.813980575719,289.811808732788,290.310722811322,
290.809636889856,291.30855096839,291.807465046924,292.805293203993,293.803121361061,
294.800949518129,295.798777675197,296.796605832266,297.2955199108,297.794433989334,
298.293348067868,298.792262146402,299.79009030347,300.787918460539,301.785746617607,
302.783574774675,303.781402931743,304.280317010277,304.779231088812,305.278145167346,
305.77705924588,306.774887402948,307.772715560016,308.770543717085,309.768371874153,
310.766200031221,311.265114109755,311.764028188289,312.262942266824,312.761856345358,
313.759684502426,314.757512659494,315.755340816562,316.753168973631,317.750997130699,
318.249911209233,318.748825287767,319.247739366301,319.746653444835,320.744481601904,
321.742309758972,322.74013791604,323.737966073108,324.735794230177,325.234708308711,
325.733622387245,326.232536465779,326.731450544313,327.729278701381,328.72710685845,
329.724935015518,330.722763172586,331.720591329655,332.219505408189,332.718419486723,
333.217333565257,333.716247643791,334.714075800859,335.711903957928,336.709732114996,
337.707560272064,338.705388429132,339.204302507666,339.703216586201,340.202130664735,
340.701044743269,341.698872900337,342.696701057405,343.694529214474,344.692357371542,
345.69018552861,346.189099607144,346.688013685678,347.186927764213,347.685841842747,
348.683669999815,349.681498156883,350.679326313951,351.67715447102,352.674982628088,
353.173896706622,353.672810785156,354.17172486369,354.670638942224,355.668467099293,
356.666295256361,357.664123413429,358.661951570497,359.659779727566,360.1586938061,
360.657607884634,361.156521963168,361.655436041702,362.653264198771,363.651092355839,
364.648920512907,365.646748669975,366.644576827044,367.143490905578,367.642404984112,
368.141319062646,368.64023314118,369.638061298248,370.635889455317,371.633717612385,
372.631545769453,373.629373926521,374.128288005055,374.62720208359,375.126116162124,
375.625030240658,376.622858397726,377.620686554794,378.618514711863,379.616342868931,
380.614171025999,381.113085104533,381.611999183067,382.110913261602,382.609827340136,
383.607655497204,384.605483654272,385.60331181134,386.601139968409,387.598968125477,
388.097882204011,388.596796282545,389.095710361079,389.594624439613,390.592452596682,
391.59028075375,392.588108910818,393.585937067887,394.583765224955,395.082679303489,
395.581593382023,396.080507460557,396.579421539091,397.57724969616,398.575077853228,
399.572906010296,400.570734167364,401.568562324433,402.067476402967,402.566390481501,
403.065304560035,403.564218638569,404.562046795637,405.559874952706,406.557703109774,
407.056617188308,407.555531266842,408.054445345376,408.55335942391),
 .UNSPECIFIED.);
#836=B_SPLINE_SURFACE_WITH_KNOTS('',3,3,((#40363,#40364,#40365,#40366,#40367,
#40368,#40369,#40370,#40371,#40372,#40373,#40374,#40375,#40376,#40377,#40378,
#40379,#40380,#40381,#40382,#40383,#40384,#40385,#40386,#40387,#40388,#40389,
#40390,#40391,#40392,#40393,#40394,#40395,#40396,#40397,#40398,#40399,#40400,
#40401,#40402,#40403,#40404,#40405,#40406,#40407,#40408,#40409,#40410,#40411,
#40412,#40413,#40414,#40415,#40416,#40417,#40418,#40419,#40420,#40421,#40422,
#40423,#40424,#40425,#40426,#40427,#40428,#40429,#40430,#40431,#40432,#40433,
#40434,#40435,#40436,#40437,#40438,#40439,#40440,#40441,#40442,#40443,#40444,
#40445,#40446,#40447,#40448,#40449,#40450,#40451,#40452,#40453,#40454,#40455,
#40456,#40457,#40458,#40459,#40460,#40461,#40462,#40463,#40464,#40465,#40466,
#40467,#40468,#40469,#40470,#40471,#40472,#40473,#40474,#40475,#40476,#40477,
#40478,#40479,#40480,#40481,#40482,#40483,#40484,#40485,#40486,#40487,#40488,
#40489,#40490,#40491,#40492,#40493,#40494,#40495,#40496,#40497,#40498,#40499,
#40500,#40501,#40502,#40503,#40504,#40505,#40506,#40507,#40508,#40509,#40510,
#40511,#40512,#40513,#40514,#40515,#40516,#40517,#40518,#40519,#40520,#40521,
#40522,#40523,#40524,#40525,#40526,#40527,#40528,#40529,#40530,#40531,#40532,
#40533,#40534,#40535,#40536,#40537,#40538,#40539,#40540,#40541,#40542,#40543,
#40544,#40545,#40546,#40547,#40548,#40549,#40550,#40551,#40552,#40553,#40554,
#40555,#40556,#40557,#40558,#40559,#40560,#40561,#40562,#40563,#40564,#40565,
#40566,#40567,#40568,#40569,#40570,#40571),(#40572,#40573,#40574,#40575,
#40576,#40577,#40578,#40579,#40580,#40581,#40582,#40583,#40584,#40585,#40586,
#40587,#40588,#40589,#40590,#40591,#40592,#40593,#40594,#40595,#40596,#40597,
#40598,#40599,#40600,#40601,#40602,#40603,#40604,#40605,#40606,#40607,#40608,
#40609,#40610,#40611,#40612,#40613,#40614,#40615,#40616,#40617,#40618,#40619,
#40620,#40621,#40622,#40623,#40624,#40625,#40626,#40627,#40628,#40629,#40630,
#40631,#40632,#40633,#40634,#40635,#40636,#40637,#40638,#40639,#40640,#40641,
#40642,#40643,#40644,#40645,#40646,#40647,#40648,#40649,#40650,#40651,#40652,
#40653,#40654,#40655,#40656,#40657,#40658,#40659,#40660,#40661,#40662,#40663,
#40664,#40665,#40666,#40667,#40668,#40669,#40670,#40671,#40672,#40673,#40674,
#40675,#40676,#40677,#40678,#40679,#40680,#40681,#40682,#40683,#40684,#40685,
#40686,#40687,#40688,#40689,#40690,#40691,#40692,#40693,#40694,#40695,#40696,
#40697,#40698,#40699,#40700,#40701,#40702,#40703,#40704,#40705,#40706,#40707,
#40708,#40709,#40710,#40711,#40712,#40713,#40714,#40715,#40716,#40717,#40718,
#40719,#40720,#40721,#40722,#40723,#40724,#40725,#40726,#40727,#40728,#40729,
#40730,#40731,#40732,#40733,#40734,#40735,#40736,#40737,#40738,#40739,#40740,
#40741,#40742,#40743,#40744,#40745,#40746,#40747,#40748,#40749,#40750,#40751,
#40752,#40753,#40754,#40755,#40756,#40757,#40758,#40759,#40760,#40761,#40762,
#40763,#40764,#40765,#40766,#40767,#40768,#40769,#40770,#40771,#40772,#40773,
#40774,#40775,#40776,#40777,#40778,#40779,#40780),(#40781,#40782,#40783,
#40784,#40785,#40786,#40787,#40788,#40789,#40790,#40791,#40792,#40793,#40794,
#40795,#40796,#40797,#40798,#40799,#40800,#40801,#40802,#40803,#40804,#40805,
#40806,#40807,#40808,#40809,#40810,#40811,#40812,#40813,#40814,#40815,#40816,
#40817,#40818,#40819,#40820,#40821,#40822,#40823,#40824,#40825,#40826,#40827,
#40828,#40829,#40830,#40831,#40832,#40833,#40834,#40835,#40836,#40837,#40838,
#40839,#40840,#40841,#40842,#40843,#40844,#40845,#40846,#40847,#40848,#40849,
#40850,#40851,#40852,#40853,#40854,#40855,#40856,#40857,#40858,#40859,#40860,
#40861,#40862,#40863,#40864,#40865,#40866,#40867,#40868,#40869,#40870,#40871,
#40872,#40873,#40874,#40875,#40876,#40877,#40878,#40879,#40880,#40881,#40882,
#40883,#40884,#40885,#40886,#40887,#40888,#40889,#40890,#40891,#40892,#40893,
#40894,#40895,#40896,#40897,#40898,#40899,#40900,#40901,#40902,#40903,#40904,
#40905,#40906,#40907,#40908,#40909,#40910,#40911,#40912,#40913,#40914,#40915,
#40916,#40917,#40918,#40919,#40920,#40921,#40922,#40923,#40924,#40925,#40926,
#40927,#40928,#40929,#40930,#40931,#40932,#40933,#40934,#40935,#40936,#40937,
#40938,#40939,#40940,#40941,#40942,#40943,#40944,#40945,#40946,#40947,#40948,
#40949,#40950,#40951,#40952,#40953,#40954,#40955,#40956,#40957,#40958,#40959,
#40960,#40961,#40962,#40963,#40964,#40965,#40966,#40967,#40968,#40969,#40970,
#40971,#40972,#40973,#40974,#40975,#40976,#40977,#40978,#40979,#40980,#40981,
#40982,#40983,#40984,#40985,#40986,#40987,#40988,#40989),(#40990,#40991,
#40992,#40993,#40994,#40995,#40996,#40997,#40998,#40999,#41000,#41001,#41002,
#41003,#41004,#41005,#41006,#41007,#41008,#41009,#41010,#41011,#41012,#41013,
#41014,#41015,#41016,#41017,#41018,#41019,#41020,#41021,#41022,#41023,#41024,
#41025,#41026,#41027,#41028,#41029,#41030,#41031,#41032,#41033,#41034,#41035,
#41036,#41037,#41038,#41039,#41040,#41041,#41042,#41043,#41044,#41045,#41046,
#41047,#41048,#41049,#41050,#41051,#41052,#41053,#41054,#41055,#41056,#41057,
#41058,#41059,#41060,#41061,#41062,#41063,#41064,#41065,#41066,#41067,#41068,
#41069,#41070,#41071,#41072,#41073,#41074,#41075,#41076,#41077,#41078,#41079,
#41080,#41081,#41082,#41083,#41084,#41085,#41086,#41087,#41088,#41089,#41090,
#41091,#41092,#41093,#41094,#41095,#41096,#41097,#41098,#41099,#41100,#41101,
#41102,#41103,#41104,#41105,#41106,#41107,#41108,#41109,#41110,#41111,#41112,
#41113,#41114,#41115,#41116,#41117,#41118,#41119,#41120,#41121,#41122,#41123,
#41124,#41125,#41126,#41127,#41128,#41129,#41130,#41131,#41132,#41133,#41134,
#41135,#41136,#41137,#41138,#41139,#41140,#41141,#41142,#41143,#41144,#41145,
#41146,#41147,#41148,#41149,#41150,#41151,#41152,#41153,#41154,#41155,#41156,
#41157,#41158,#41159,#41160,#41161,#41162,#41163,#41164,#41165,#41166,#41167,
#41168,#41169,#41170,#41171,#41172,#41173,#41174,#41175,#41176,#41177,#41178,
#41179,#41180,#41181,#41182,#41183,#41184,#41185,#41186,#41187,#41188,#41189,
#41190,#41191,#41192,#41193,#41194,#41195,#41196,#41197,#41198)),
 .UNSPECIFIED.,.F.,.F.,.F.,(4,4),(4,1,1,1,1,1,1,1,1,1,1,1,1,1,1,1,1,1,1,
1,1,1,1,1,1,1,1,1,1,1,1,1,1,1,1,1,1,1,1,1,1,1,1,1,1,1,1,1,1,1,1,1,1,1,1,
1,1,1,1,1,1,1,1,1,1,1,1,1,1,1,1,1,1,1,1,1,1,1,1,1,1,1,1,1,1,1,1,1,1,1,1,
1,1,1,1,1,1,1,1,1,1,1,1,1,1,1,1,1,1,1,1,1,1,1,1,1,1,1,1,1,1,1,1,1,1,1,1,
1,1,1,1,1,1,1,1,1,1,1,1,1,1,1,1,1,1,1,1,1,1,1,1,1,1,1,1,1,1,1,1,1,1,1,1,
1,1,1,1,1,1,1,1,1,1,1,1,1,1,1,1,1,1,1,1,1,1,1,1,1,1,1,1,1,1,1,1,1,1,1,1,
1,1,1,1,1,1,1,4),(0.,0.0824167509268187),(8.58761471263784,9.08568424559332,
9.58375377854879,10.0818233115043,10.5798928444598,11.0779623774152,11.5760319103707,
12.0741014433262,12.5721709762817,13.0702405092372,13.5683100421926,14.0663795751481,
14.5644491081036,15.0625186410591,15.5605881740146,16.05865770697,16.5567272399255,
17.054796772881,17.5528663058365,18.0509358387919,18.5490053717474,19.0470749047029,
19.5451444376584,20.0432139706139,20.5412835035693,21.0393530365248,21.5374225694803,
22.0354921024358,22.5335616353913,23.0316311683467,23.5297007013022,24.0277702342577,
24.5258397672132,25.0239093001687,25.5219788331241,26.0200483660796,26.5181178990351,
27.0161874319906,27.5142569649461,28.0123264979015,28.510396030857,29.0084655638125,
29.506535096768,30.0046046297235,30.5026741626789,31.0007436956344,31.4988132285899,
31.9968827615454,32.4949522945009,32.9930218274563,33.4910913604118,33.9891608933673,
34.4872304263228,34.9852999592783,35.4833694922337,35.9814390251892,36.4795085581447,
36.9775780911002,37.4756476240557,37.9737171570111,38.4717866899666,38.9698562229221,
39.4679257558776,39.9659952888331,40.4640648217885,40.962134354744,41.4602038876995,
41.958273420655,42.4563429536105,42.9544124865659,43.4524820195214,43.9505515524769,
44.4486210854324,44.9466906183878,45.4447601513433,45.9428296842988,46.4408992172543,
46.9389687502098,47.4370382831653,47.9351078161207,48.4331773490762,48.9312468820317,
49.4293164149872,49.9273859479427,50.4254554808981,50.9235250138536,51.4215945468091,
51.9196640797646,52.41773361272,52.9158031456755,53.413872678631,53.9119422115865,
54.410011744542,54.9080812774974,55.4061508104529,55.9042203434084,56.4022898763639,
56.9003594093194,57.3984289422748,57.8964984752303,58.3945680081858,58.8926375411413,
59.3907070740968,59.8887766070523,60.3868461400077,60.8849156729632,61.3829852059187,
61.8810547388742,62.3791242718296,62.8771938047851,63.3752633377406,63.8733328706961,
64.3714024036516,64.869471936607,65.3675414695625,65.865611002518,66.3636805354735,
66.861750068429,67.3598196013844,67.8578891343399,68.3559586672954,68.8540282002509,
69.3520977332063,69.8501672661618,70.3482367991173,70.8463063320728,71.3443758650283,
71.8424453979838,72.3405149309392,72.8385844638947,73.3366539968502,73.8347235298057,
74.3327930627611,74.8308625957166,75.3289321286721,75.8270016616276,76.3250711945831,
76.8231407275385,77.321210260494,77.8192797934495,78.317349326405,78.8154188593605,
79.3134883923159,79.8115579252714,80.3096274582269,80.8076969911824,81.3057665241379,
81.8038360570933,82.3019055900488,82.7999751230043,83.2980446559598,83.7961141889153,
84.2941837218707,84.7922532548262,85.2903227877817,85.7883923207372,86.2864618536927,
86.7845313866481,87.2826009196036,87.7806704525591,88.2787399855146,88.7768095184701,
89.2748790514255,89.772948584381,90.2710181173365,90.769087650292,91.2671571832475,
91.7652267162029,92.2632962491584,92.7613657821139,93.2594353150694,93.7575048480249,
94.2555743809803,94.7536439139358,95.2517134468913,95.7497829798468,96.2478525128023,
96.7459220457577,97.2439915787132,97.7420611116687,98.2401306446242,98.7382001775796,
99.2362697105351,99.7343392434906,100.232408776446,100.730478309402,101.228547842357,
101.726617375313,102.224686908268,102.722756441223,103.220825974179,103.718895507134,
104.21696504009,104.715034573045,105.213104106001,105.711173638956,106.209243171912,
106.707312704867,107.205382237823,107.703451770778,108.201521303734,108.699590836689,
109.197660369645,109.6957299026,110.193799435556,110.691868968511,111.189938501467),
 .UNSPECIFIED.);
#837=B_SPLINE_SURFACE_WITH_KNOTS('',3,3,((#41493,#41494,#41495,#41496,#41497,
#41498,#41499,#41500,#41501,#41502,#41503,#41504,#41505,#41506,#41507,#41508,
#41509,#41510,#41511,#41512,#41513,#41514,#41515,#41516,#41517,#41518,#41519,
#41520,#41521,#41522,#41523,#41524,#41525,#41526,#41527,#41528,#41529,#41530,
#41531,#41532,#41533,#41534,#41535,#41536,#41537,#41538,#41539,#41540,#41541,
#41542,#41543,#41544,#41545,#41546,#41547,#41548,#41549,#41550,#41551,#41552,
#41553,#41554,#41555,#41556,#41557,#41558,#41559,#41560,#41561,#41562,#41563,
#41564,#41565,#41566,#41567,#41568,#41569,#41570,#41571,#41572,#41573,#41574,
#41575,#41576,#41577,#41578,#41579,#41580,#41581,#41582,#41583,#41584,#41585,
#41586,#41587,#41588,#41589,#41590,#41591,#41592,#41593,#41594,#41595,#41596,
#41597,#41598,#41599,#41600,#41601,#41602,#41603,#41604,#41605,#41606,#41607,
#41608,#41609,#41610,#41611,#41612,#41613,#41614,#41615,#41616,#41617,#41618,
#41619,#41620,#41621,#41622,#41623,#41624,#41625,#41626,#41627,#41628,#41629,
#41630,#41631,#41632,#41633,#41634,#41635,#41636,#41637,#41638,#41639,#41640,
#41641,#41642,#41643,#41644,#41645,#41646,#41647,#41648,#41649,#41650,#41651,
#41652,#41653,#41654,#41655,#41656,#41657,#41658,#41659,#41660,#41661,#41662,
#41663,#41664,#41665,#41666,#41667,#41668,#41669,#41670,#41671,#41672,#41673,
#41674,#41675,#41676,#41677,#41678,#41679,#41680,#41681,#41682,#41683,#41684,
#41685,#41686,#41687,#41688,#41689,#41690,#41691,#41692,#41693,#41694,#41695,
#41696,#41697,#41698,#41699,#41700,#41701),(#41702,#41703,#41704,#41705,
#41706,#41707,#41708,#41709,#41710,#41711,#41712,#41713,#41714,#41715,#41716,
#41717,#41718,#41719,#41720,#41721,#41722,#41723,#41724,#41725,#41726,#41727,
#41728,#41729,#41730,#41731,#41732,#41733,#41734,#41735,#41736,#41737,#41738,
#41739,#41740,#41741,#41742,#41743,#41744,#41745,#41746,#41747,#41748,#41749,
#41750,#41751,#41752,#41753,#41754,#41755,#41756,#41757,#41758,#41759,#41760,
#41761,#41762,#41763,#41764,#41765,#41766,#41767,#41768,#41769,#41770,#41771,
#41772,#41773,#41774,#41775,#41776,#41777,#41778,#41779,#41780,#41781,#41782,
#41783,#41784,#41785,#41786,#41787,#41788,#41789,#41790,#41791,#41792,#41793,
#41794,#41795,#41796,#41797,#41798,#41799,#41800,#41801,#41802,#41803,#41804,
#41805,#41806,#41807,#41808,#41809,#41810,#41811,#41812,#41813,#41814,#41815,
#41816,#41817,#41818,#41819,#41820,#41821,#41822,#41823,#41824,#41825,#41826,
#41827,#41828,#41829,#41830,#41831,#41832,#41833,#41834,#41835,#41836,#41837,
#41838,#41839,#41840,#41841,#41842,#41843,#41844,#41845,#41846,#41847,#41848,
#41849,#41850,#41851,#41852,#41853,#41854,#41855,#41856,#41857,#41858,#41859,
#41860,#41861,#41862,#41863,#41864,#41865,#41866,#41867,#41868,#41869,#41870,
#41871,#41872,#41873,#41874,#41875,#41876,#41877,#41878,#41879,#41880,#41881,
#41882,#41883,#41884,#41885,#41886,#41887,#41888,#41889,#41890,#41891,#41892,
#41893,#41894,#41895,#41896,#41897,#41898,#41899,#41900,#41901,#41902,#41903,
#41904,#41905,#41906,#41907,#41908,#41909,#41910),(#41911,#41912,#41913,
#41914,#41915,#41916,#41917,#41918,#41919,#41920,#41921,#41922,#41923,#41924,
#41925,#41926,#41927,#41928,#41929,#41930,#41931,#41932,#41933,#41934,#41935,
#41936,#41937,#41938,#41939,#41940,#41941,#41942,#41943,#41944,#41945,#41946,
#41947,#41948,#41949,#41950,#41951,#41952,#41953,#41954,#41955,#41956,#41957,
#41958,#41959,#41960,#41961,#41962,#41963,#41964,#41965,#41966,#41967,#41968,
#41969,#41970,#41971,#41972,#41973,#41974,#41975,#41976,#41977,#41978,#41979,
#41980,#41981,#41982,#41983,#41984,#41985,#41986,#41987,#41988,#41989,#41990,
#41991,#41992,#41993,#41994,#41995,#41996,#41997,#41998,#41999,#42000,#42001,
#42002,#42003,#42004,#42005,#42006,#42007,#42008,#42009,#42010,#42011,#42012,
#42013,#42014,#42015,#42016,#42017,#42018,#42019,#42020,#42021,#42022,#42023,
#42024,#42025,#42026,#42027,#42028,#42029,#42030,#42031,#42032,#42033,#42034,
#42035,#42036,#42037,#42038,#42039,#42040,#42041,#42042,#42043,#42044,#42045,
#42046,#42047,#42048,#42049,#42050,#42051,#42052,#42053,#42054,#42055,#42056,
#42057,#42058,#42059,#42060,#42061,#42062,#42063,#42064,#42065,#42066,#42067,
#42068,#42069,#42070,#42071,#42072,#42073,#42074,#42075,#42076,#42077,#42078,
#42079,#42080,#42081,#42082,#42083,#42084,#42085,#42086,#42087,#42088,#42089,
#42090,#42091,#42092,#42093,#42094,#42095,#42096,#42097,#42098,#42099,#42100,
#42101,#42102,#42103,#42104,#42105,#42106,#42107,#42108,#42109,#42110,#42111,
#42112,#42113,#42114,#42115,#42116,#42117,#42118,#42119),(#42120,#42121,
#42122,#42123,#42124,#42125,#42126,#42127,#42128,#42129,#42130,#42131,#42132,
#42133,#42134,#42135,#42136,#42137,#42138,#42139,#42140,#42141,#42142,#42143,
#42144,#42145,#42146,#42147,#42148,#42149,#42150,#42151,#42152,#42153,#42154,
#42155,#42156,#42157,#42158,#42159,#42160,#42161,#42162,#42163,#42164,#42165,
#42166,#42167,#42168,#42169,#42170,#42171,#42172,#42173,#42174,#42175,#42176,
#42177,#42178,#42179,#42180,#42181,#42182,#42183,#42184,#42185,#42186,#42187,
#42188,#42189,#42190,#42191,#42192,#42193,#42194,#42195,#42196,#42197,#42198,
#42199,#42200,#42201,#42202,#42203,#42204,#42205,#42206,#42207,#42208,#42209,
#42210,#42211,#42212,#42213,#42214,#42215,#42216,#42217,#42218,#42219,#42220,
#42221,#42222,#42223,#42224,#42225,#42226,#42227,#42228,#42229,#42230,#42231,
#42232,#42233,#42234,#42235,#42236,#42237,#42238,#42239,#42240,#42241,#42242,
#42243,#42244,#42245,#42246,#42247,#42248,#42249,#42250,#42251,#42252,#42253,
#42254,#42255,#42256,#42257,#42258,#42259,#42260,#42261,#42262,#42263,#42264,
#42265,#42266,#42267,#42268,#42269,#42270,#42271,#42272,#42273,#42274,#42275,
#42276,#42277,#42278,#42279,#42280,#42281,#42282,#42283,#42284,#42285,#42286,
#42287,#42288,#42289,#42290,#42291,#42292,#42293,#42294,#42295,#42296,#42297,
#42298,#42299,#42300,#42301,#42302,#42303,#42304,#42305,#42306,#42307,#42308,
#42309,#42310,#42311,#42312,#42313,#42314,#42315,#42316,#42317,#42318,#42319,
#42320,#42321,#42322,#42323,#42324,#42325,#42326,#42327,#42328)),
 .UNSPECIFIED.,.F.,.F.,.F.,(4,4),(4,1,1,1,1,1,1,1,1,1,1,1,1,1,1,1,1,1,1,
1,1,1,1,1,1,1,1,1,1,1,1,1,1,1,1,1,1,1,1,1,1,1,1,1,1,1,1,1,1,1,1,1,1,1,1,
1,1,1,1,1,1,1,1,1,1,1,1,1,1,1,1,1,1,1,1,1,1,1,1,1,1,1,1,1,1,1,1,1,1,1,1,
1,1,1,1,1,1,1,1,1,1,1,1,1,1,1,1,1,1,1,1,1,1,1,1,1,1,1,1,1,1,1,1,1,1,1,1,
1,1,1,1,1,1,1,1,1,1,1,1,1,1,1,1,1,1,1,1,1,1,1,1,1,1,1,1,1,1,1,1,1,1,1,1,
1,1,1,1,1,1,1,1,1,1,1,1,1,1,1,1,1,1,1,1,1,1,1,1,1,1,1,1,1,1,1,1,1,1,1,1,
1,1,1,1,1,1,1,4),(0.,0.0824167509268187),(11.897963259076,12.3960327920314,
12.8941023249869,13.3921718579424,13.8902413908979,14.3883109238534,14.8863804568088,
15.3844499897643,15.8825195227198,16.3805890556753,16.8786585886308,17.3767281215862,
17.8747976545417,18.3728671874972,18.8709367204527,19.3690062534082,19.8670757863636,
20.3651453193191,20.8632148522746,21.3612843852301,21.8593539181856,22.357423451141,
22.8554929840965,23.353562517052,23.8516320500075,24.349701582963,24.8477711159184,
25.3458406488739,25.8439101818294,26.3419797147849,26.8400492477403,27.3381187806958,
27.8361883136513,28.3342578466068,28.8323273795623,29.3303969125177,29.8284664454732,
30.3265359784287,30.8246055113842,31.3226750443397,31.8207445772951,32.3188141102506,
32.8168836432061,33.3149531761616,33.8130227091171,34.3110922420725,34.809161775028,
35.3072313079835,35.805300840939,36.3033703738945,36.8014399068499,37.2995094398054,
37.7975789727609,38.2956485057164,38.7937180386719,39.2917875716273,39.7898571045828,
40.2879266375383,40.7859961704938,41.2840657034493,41.7821352364047,42.2802047693602,
42.7782743023157,43.2763438352712,43.7744133682266,44.2724829011821,44.7705524341376,
45.2686219670931,45.7666915000486,46.264761033004,46.7628305659595,47.260900098915,
47.7589696318705,48.257039164826,48.7551086977815,49.2531782307369,49.7512477636924,
50.2493172966479,50.7473868296034,51.2454563625588,51.7435258955143,52.2415954284698,
52.7396649614253,53.2377344943808,53.7358040273362,54.2338735602917,54.7319430932472,
55.2300126262027,55.7280821591582,56.2261516921136,56.7242212250691,57.2222907580246,
57.7203602909801,58.2184298239356,58.716499356891,59.2145688898465,59.712638422802,
60.2107079557575,60.708777488713,61.2068470216684,61.7049165546239,62.2029860875794,
62.7010556205349,63.1991251534903,63.6971946864458,64.1952642194013,64.6933337523568,
65.1914032853123,65.6894728182677,66.1875423512232,66.6856118841787,67.1836814171342,
67.6817509500897,68.1798204830451,68.6778900160006,69.1759595489561,69.6740290819116,
70.1720986148671,70.6701681478225,71.168237680778,71.6663072137335,72.164376746689,
72.6624462796445,73.1605158125999,73.6585853455554,74.1566548785109,74.6547244114664,
75.1527939444219,75.6508634773773,76.1489330103328,76.6470025432883,77.1450720762438,
77.6431416091993,78.1412111421547,78.6392806751102,79.1373502080657,79.6354197410212,
80.1334892739767,80.6315588069321,81.1296283398876,81.6276978728431,82.1257674057986,
82.6238369387541,83.1219064717095,83.619976004665,84.1180455376205,84.616115070576,
85.1141846035315,85.6122541364869,86.1103236694424,86.6083932023979,87.1064627353534,
87.6045322683088,88.1026018012643,88.6006713342198,89.0987408671753,89.5968104001308,
90.0948799330862,90.5929494660417,91.0910189989972,91.5890885319527,92.0871580649082,
92.5852275978636,93.0832971308191,93.5813666637746,94.0794361967301,94.5775057296856,
95.0755752626411,95.5736447955965,96.071714328552,96.5697838615075,97.067853394463,
97.5659229274184,98.0639924603739,98.5620619933294,99.0601315262849,99.5582010592404,
100.056270592196,100.554340125151,101.052409658107,101.550479191062,102.048548724018,
102.546618256973,103.044687789929,103.542757322884,104.04082685584,104.538896388795,
105.036965921751,105.535035454706,106.033104987662,106.531174520617,107.029244053573,
107.527313586528,108.025383119484,108.523452652439,109.021522185394,109.51959171835,
110.017661251305,110.515730784261,111.013800317216,111.511869850172,112.009939383127,
112.508008916083,113.006078449038,113.504147981994,114.002217514949,114.500287047905),
 .UNSPECIFIED.);
#838=B_SPLINE_SURFACE_WITH_KNOTS('',3,3,((#48066,#48067,#48068,#48069),
(#48070,#48071,#48072,#48073),(#48074,#48075,#48076,#48077),(#48078,#48079,
#48080,#48081),(#48082,#48083,#48084,#48085),(#48086,#48087,#48088,#48089),
(#48090,#48091,#48092,#48093)),.UNSPECIFIED.,.F.,.F.,.F.,(4,1,1,1,4),(4,
4),(0.,0.285714285714286,0.571428571428571,0.857142857142857,1.),(0.363335998515663,
0.499634934734419),.UNSPECIFIED.);
#839=B_SPLINE_SURFACE_WITH_KNOTS('',3,3,((#48278,#48279,#48280,#48281),
(#48282,#48283,#48284,#48285),(#48286,#48287,#48288,#48289),(#48290,#48291,
#48292,#48293),(#48294,#48295,#48296,#48297),(#48298,#48299,#48300,#48301),
(#48302,#48303,#48304,#48305)),.UNSPECIFIED.,.F.,.F.,.F.,(4,1,1,1,4),(4,
4),(0.,0.285714285714286,0.571428571428571,0.857142857142857,1.),(0.,0.136299039595008),
 .UNSPECIFIED.);
#840=B_SPLINE_SURFACE_WITH_KNOTS('',3,3,((#48415,#48416,#48417,#48418),
(#48419,#48420,#48421,#48422),(#48423,#48424,#48425,#48426),(#48427,#48428,
#48429,#48430)),.UNSPECIFIED.,.F.,.F.,.F.,(4,4),(4,4),(0.,1.),(0.,0.0923903836946144),
 .UNSPECIFIED.);
#841=B_SPLINE_SURFACE_WITH_KNOTS('',3,3,((#48482,#48483,#48484,#48485),
(#48486,#48487,#48488,#48489),(#48490,#48491,#48492,#48493),(#48494,#48495,
#48496,#48497)),.UNSPECIFIED.,.F.,.F.,.F.,(4,4),(4,4),(0.,1.),(0.,0.0923903843306348),
 .UNSPECIFIED.);
#842=B_SPLINE_SURFACE_WITH_KNOTS('',3,3,((#48548,#48549,#48550,#48551),
(#48552,#48553,#48554,#48555),(#48556,#48557,#48558,#48559),(#48560,#48561,
#48562,#48563),(#48564,#48565,#48566,#48567),(#48568,#48569,#48570,#48571),
(#48572,#48573,#48574,#48575)),.UNSPECIFIED.,.F.,.F.,.F.,(4,1,1,1,4),(4,
4),(0.,0.285714285714286,0.571428571428571,0.857142857142857,1.),(0.,0.136298877173929),
 .UNSPECIFIED.);
#843=B_SPLINE_SURFACE_WITH_KNOTS('',3,3,((#62685,#62686,#62687,#62688,#62689,
#62690,#62691,#62692,#62693,#62694,#62695,#62696,#62697,#62698,#62699,#62700,
#62701,#62702,#62703,#62704,#62705,#62706,#62707,#62708,#62709,#62710,#62711,
#62712,#62713,#62714,#62715,#62716,#62717,#62718,#62719,#62720,#62721,#62722,
#62723,#62724,#62725,#62726,#62727,#62728,#62729,#62730,#62731,#62732,#62733,
#62734,#62735,#62736,#62737,#62738,#62739,#62740,#62741,#62742,#62743,#62744,
#62745,#62746,#62747,#62748,#62749,#62750,#62751,#62752,#62753,#62754,#62755,
#62756,#62757,#62758,#62759,#62760),(#62761,#62762,#62763,#62764,#62765,
#62766,#62767,#62768,#62769,#62770,#62771,#62772,#62773,#62774,#62775,#62776,
#62777,#62778,#62779,#62780,#62781,#62782,#62783,#62784,#62785,#62786,#62787,
#62788,#62789,#62790,#62791,#62792,#62793,#62794,#62795,#62796,#62797,#62798,
#62799,#62800,#62801,#62802,#62803,#62804,#62805,#62806,#62807,#62808,#62809,
#62810,#62811,#62812,#62813,#62814,#62815,#62816,#62817,#62818,#62819,#62820,
#62821,#62822,#62823,#62824,#62825,#62826,#62827,#62828,#62829,#62830,#62831,
#62832,#62833,#62834,#62835,#62836),(#62837,#62838,#62839,#62840,#62841,
#62842,#62843,#62844,#62845,#62846,#62847,#62848,#62849,#62850,#62851,#62852,
#62853,#62854,#62855,#62856,#62857,#62858,#62859,#62860,#62861,#62862,#62863,
#62864,#62865,#62866,#62867,#62868,#62869,#62870,#62871,#62872,#62873,#62874,
#62875,#62876,#62877,#62878,#62879,#62880,#62881,#62882,#62883,#62884,#62885,
#62886,#62887,#62888,#62889,#62890,#62891,#62892,#62893,#62894,#62895,#62896,
#62897,#62898,#62899,#62900,#62901,#62902,#62903,#62904,#62905,#62906,#62907,
#62908,#62909,#62910,#62911,#62912),(#62913,#62914,#62915,#62916,#62917,
#62918,#62919,#62920,#62921,#62922,#62923,#62924,#62925,#62926,#62927,#62928,
#62929,#62930,#62931,#62932,#62933,#62934,#62935,#62936,#62937,#62938,#62939,
#62940,#62941,#62942,#62943,#62944,#62945,#62946,#62947,#62948,#62949,#62950,
#62951,#62952,#62953,#62954,#62955,#62956,#62957,#62958,#62959,#62960,#62961,
#62962,#62963,#62964,#62965,#62966,#62967,#62968,#62969,#62970,#62971,#62972,
#62973,#62974,#62975,#62976,#62977,#62978,#62979,#62980,#62981,#62982,#62983,
#62984,#62985,#62986,#62987,#62988),(#62989,#62990,#62991,#62992,#62993,
#62994,#62995,#62996,#62997,#62998,#62999,#63000,#63001,#63002,#63003,#63004,
#63005,#63006,#63007,#63008,#63009,#63010,#63011,#63012,#63013,#63014,#63015,
#63016,#63017,#63018,#63019,#63020,#63021,#63022,#63023,#63024,#63025,#63026,
#63027,#63028,#63029,#63030,#63031,#63032,#63033,#63034,#63035,#63036,#63037,
#63038,#63039,#63040,#63041,#63042,#63043,#63044,#63045,#63046,#63047,#63048,
#63049,#63050,#63051,#63052,#63053,#63054,#63055,#63056,#63057,#63058,#63059,
#63060,#63061,#63062,#63063,#63064),(#63065,#63066,#63067,#63068,#63069,
#63070,#63071,#63072,#63073,#63074,#63075,#63076,#63077,#63078,#63079,#63080,
#63081,#63082,#63083,#63084,#63085,#63086,#63087,#63088,#63089,#63090,#63091,
#63092,#63093,#63094,#63095,#63096,#63097,#63098,#63099,#63100,#63101,#63102,
#63103,#63104,#63105,#63106,#63107,#63108,#63109,#63110,#63111,#63112,#63113,
#63114,#63115,#63116,#63117,#63118,#63119,#63120,#63121,#63122,#63123,#63124,
#63125,#63126,#63127,#63128,#63129,#63130,#63131,#63132,#63133,#63134,#63135,
#63136,#63137,#63138,#63139,#63140),(#63141,#63142,#63143,#63144,#63145,
#63146,#63147,#63148,#63149,#63150,#63151,#63152,#63153,#63154,#63155,#63156,
#63157,#63158,#63159,#63160,#63161,#63162,#63163,#63164,#63165,#63166,#63167,
#63168,#63169,#63170,#63171,#63172,#63173,#63174,#63175,#63176,#63177,#63178,
#63179,#63180,#63181,#63182,#63183,#63184,#63185,#63186,#63187,#63188,#63189,
#63190,#63191,#63192,#63193,#63194,#63195,#63196,#63197,#63198,#63199,#63200,
#63201,#63202,#63203,#63204,#63205,#63206,#63207,#63208,#63209,#63210,#63211,
#63212,#63213,#63214,#63215,#63216),(#63217,#63218,#63219,#63220,#63221,
#63222,#63223,#63224,#63225,#63226,#63227,#63228,#63229,#63230,#63231,#63232,
#63233,#63234,#63235,#63236,#63237,#63238,#63239,#63240,#63241,#63242,#63243,
#63244,#63245,#63246,#63247,#63248,#63249,#63250,#63251,#63252,#63253,#63254,
#63255,#63256,#63257,#63258,#63259,#63260,#63261,#63262,#63263,#63264,#63265,
#63266,#63267,#63268,#63269,#63270,#63271,#63272,#63273,#63274,#63275,#63276,
#63277,#63278,#63279,#63280,#63281,#63282,#63283,#63284,#63285,#63286,#63287,
#63288,#63289,#63290,#63291,#63292),(#63293,#63294,#63295,#63296,#63297,
#63298,#63299,#63300,#63301,#63302,#63303,#63304,#63305,#63306,#63307,#63308,
#63309,#63310,#63311,#63312,#63313,#63314,#63315,#63316,#63317,#63318,#63319,
#63320,#63321,#63322,#63323,#63324,#63325,#63326,#63327,#63328,#63329,#63330,
#63331,#63332,#63333,#63334,#63335,#63336,#63337,#63338,#63339,#63340,#63341,
#63342,#63343,#63344,#63345,#63346,#63347,#63348,#63349,#63350,#63351,#63352,
#63353,#63354,#63355,#63356,#63357,#63358,#63359,#63360,#63361,#63362,#63363,
#63364,#63365,#63366,#63367,#63368),(#63369,#63370,#63371,#63372,#63373,
#63374,#63375,#63376,#63377,#63378,#63379,#63380,#63381,#63382,#63383,#63384,
#63385,#63386,#63387,#63388,#63389,#63390,#63391,#63392,#63393,#63394,#63395,
#63396,#63397,#63398,#63399,#63400,#63401,#63402,#63403,#63404,#63405,#63406,
#63407,#63408,#63409,#63410,#63411,#63412,#63413,#63414,#63415,#63416,#63417,
#63418,#63419,#63420,#63421,#63422,#63423,#63424,#63425,#63426,#63427,#63428,
#63429,#63430,#63431,#63432,#63433,#63434,#63435,#63436,#63437,#63438,#63439,
#63440,#63441,#63442,#63443,#63444)),.UNSPECIFIED.,.T.,.F.,.F.,(4,1,1,1,
1,1,1,4),(4,1,1,1,1,1,1,1,1,1,1,1,1,1,1,1,1,1,1,1,1,1,1,1,1,1,1,1,1,1,1,
1,1,1,1,1,1,1,1,1,1,1,1,1,1,1,1,1,1,1,1,1,1,1,1,1,1,1,1,1,1,1,1,1,1,1,1,
1,1,1,1,1,1,4),(-3.14159265358979,-2.24399475256414,-1.34639685153848,-0.448798950512828,
0.448798950512828,1.34639685153848,2.24399475256414,3.14159265358979),(0.,
0.00892857142857143,0.0178571428571429,0.0357142857142857,0.0535714285714286,
0.0714285714285714,0.0892857142857143,0.107142857142857,0.125,0.142857142857143,
0.158730158730159,0.174603174603175,0.182539682539683,0.186507936507937,
0.19047619047619,0.202380952380952,0.214285714285714,0.226190476190476,
0.238095238095238,0.25,0.261904761904762,0.273809523809524,0.279761904761905,
0.285714285714286,0.297619047619048,0.30952380952381,0.321428571428571,
0.333333333333333,0.349206349206349,0.365079365079365,0.380952380952381,
0.396825396825397,0.412698412698413,0.428571428571429,0.436507936507937,
0.452380952380952,0.464285714285714,0.476190476190476,0.488095238095238,
0.5,0.517857142857143,0.535714285714286,0.553571428571429,0.571428571428571,
0.589285714285714,0.607142857142857,0.625,0.642857142857143,0.651785714285714,
0.660714285714286,0.678571428571428,0.696428571428571,0.714285714285714,
0.726190476190476,0.738095238095238,0.75,0.761904761904762,0.773809523809524,
0.785714285714286,0.797619047619047,0.809523809523809,0.821428571428571,
0.833333333333333,0.845238095238095,0.857142857142857,0.875,0.892857142857143,
0.910714285714286,0.928571428571429,0.946428571428571,0.964285714285714,
0.982142857142857,0.991071428571429,1.),.UNSPECIFIED.);
#844=B_SPLINE_SURFACE_WITH_KNOTS('',3,3,((#63712,#63713,#63714,#63715),
(#63716,#63717,#63718,#63719),(#63720,#63721,#63722,#63723),(#63724,#63725,
#63726,#63727),(#63728,#63729,#63730,#63731),(#63732,#63733,#63734,#63735)),
 .UNSPECIFIED.,.F.,.F.,.F.,(4,1,1,4),(4,4),(0.,0.285714285714286,0.571428571428571,
1.),(0.143091562311917,0.172672323717935),.UNSPECIFIED.);
#845=B_SPLINE_SURFACE_WITH_KNOTS('',3,3,((#63754,#63755,#63756,#63757),
(#63758,#63759,#63760,#63761),(#63762,#63763,#63764,#63765),(#63766,#63767,
#63768,#63769),(#63770,#63771,#63772,#63773),(#63774,#63775,#63776,#63777)),
 .UNSPECIFIED.,.F.,.F.,.F.,(4,1,1,4),(4,4),(0.,0.285714285714286,0.571428571428571,
1.),(0.144052021996696,0.173632784471181),.UNSPECIFIED.);
#846=B_SPLINE_SURFACE_WITH_KNOTS('',3,3,((#63891,#63892,#63893,#63894),
(#63895,#63896,#63897,#63898),(#63899,#63900,#63901,#63902),(#63903,#63904,
#63905,#63906),(#63907,#63908,#63909,#63910),(#63911,#63912,#63913,#63914)),
 .UNSPECIFIED.,.F.,.F.,.F.,(4,1,1,4),(4,4),(0.,0.285714285714286,0.571428571428571,
1.),(0.357860307352845,0.38744106972591),.UNSPECIFIED.);
#847=B_SPLINE_SURFACE_WITH_KNOTS('',3,3,((#63991,#63992,#63993,#63994),
(#63995,#63996,#63997,#63998),(#63999,#64000,#64001,#64002),(#64003,#64004,
#64005,#64006),(#64007,#64008,#64009,#64010),(#64011,#64012,#64013,#64014)),
 .UNSPECIFIED.,.F.,.F.,.F.,(4,1,1,4),(4,4),(0.,0.285714285714286,0.571428571428571,
1.),(2.06363027950495E-16,0.0295807623344723),.UNSPECIFIED.);
#848=B_SPLINE_SURFACE_WITH_KNOTS('',3,3,((#64023,#64024,#64025,#64026),
(#64027,#64028,#64029,#64030),(#64031,#64032,#64033,#64034),(#64035,#64036,
#64037,#64038),(#64039,#64040,#64041,#64042),(#64043,#64044,#64045,#64046)),
 .UNSPECIFIED.,.F.,.F.,.F.,(4,1,1,4),(4,4),(0.,0.285714285714286,0.571428571428571,
1.),(6.08201692644882E-19,0.0295807623160019),.UNSPECIFIED.);
#849=B_SPLINE_SURFACE_WITH_KNOTS('',3,3,((#64167,#64168,#64169,#64170),
(#64171,#64172,#64173,#64174),(#64175,#64176,#64177,#64178),(#64179,#64180,
#64181,#64182),(#64183,#64184,#64185,#64186),(#64187,#64188,#64189,#64190)),
 .UNSPECIFIED.,.F.,.F.,.F.,(4,1,1,4),(4,4),(0.,0.285714285714286,0.571428571428571,
1.),(2.15031488595949E-16,0.0295807575131674),.UNSPECIFIED.);
#850=B_SPLINE_SURFACE_WITH_KNOTS('',3,3,((#65115,#65116,#65117,#65118),
(#65119,#65120,#65121,#65122),(#65123,#65124,#65125,#65126),(#65127,#65128,
#65129,#65130),(#65131,#65132,#65133,#65134),(#65135,#65136,#65137,#65138),
(#65139,#65140,#65141,#65142)),.UNSPECIFIED.,.F.,.F.,.F.,(4,1,1,1,4),(4,
4),(0.,0.285714285714286,0.571428571428571,0.857142857142857,1.),(0.82916884759973,
1.33025671401017),.UNSPECIFIED.);
#851=B_SPLINE_SURFACE_WITH_KNOTS('',3,3,((#65237,#65238,#65239,#65240),
(#65241,#65242,#65243,#65244),(#65245,#65246,#65247,#65248),(#65249,#65250,
#65251,#65252),(#65253,#65254,#65255,#65256),(#65257,#65258,#65259,#65260),
(#65261,#65262,#65263,#65264)),.UNSPECIFIED.,.F.,.F.,.F.,(4,1,1,1,4),(4,
4),(0.,0.285714285714286,0.571428571428571,0.857142857142857,1.),(0.829183372221167,
1.33027123863146),.UNSPECIFIED.);
#852=B_SPLINE_SURFACE_WITH_KNOTS('',3,3,((#65276,#65277,#65278,#65279),
(#65280,#65281,#65282,#65283),(#65284,#65285,#65286,#65287),(#65288,#65289,
#65290,#65291),(#65292,#65293,#65294,#65295),(#65296,#65297,#65298,#65299),
(#65300,#65301,#65302,#65303)),.UNSPECIFIED.,.F.,.F.,.F.,(4,1,1,1,4),(4,
4),(0.,0.285714285714286,0.571428571428571,0.857142857142857,1.),(0.829168847599735,
1.33025671401018),.UNSPECIFIED.);
#853=PLANE('',#20315);
#854=PLANE('',#20316);
#855=PLANE('',#20317);
#856=PLANE('',#20318);
#857=PLANE('',#20319);
#858=PLANE('',#20322);
#859=PLANE('',#20325);
#860=PLANE('',#20328);
#861=PLANE('',#20333);
#862=PLANE('',#20338);
#863=PLANE('',#20350);
#864=PLANE('',#20355);
#865=PLANE('',#20364);
#866=PLANE('',#20369);
#867=PLANE('',#20378);
#868=PLANE('',#20383);
#869=PLANE('',#20392);
#870=PLANE('',#20397);
#871=PLANE('',#20406);
#872=PLANE('',#20411);
#873=PLANE('',#20420);
#874=PLANE('',#20425);
#875=PLANE('',#20434);
#876=PLANE('',#20440);
#877=PLANE('',#20450);
#878=PLANE('',#20455);
#879=PLANE('',#20464);
#880=PLANE('',#20469);
#881=PLANE('',#20478);
#882=PLANE('',#20483);
#883=PLANE('',#20492);
#884=PLANE('',#20497);
#885=PLANE('',#20506);
#886=PLANE('',#20511);
#887=PLANE('',#20520);
#888=PLANE('',#20525);
#889=PLANE('',#20534);
#890=PLANE('',#20539);
#891=PLANE('',#20545);
#892=PLANE('',#20554);
#893=PLANE('',#20585);
#894=PLANE('',#20588);
#895=PLANE('',#20591);
#896=PLANE('',#20597);
#897=PLANE('',#20600);
#898=PLANE('',#20607);
#899=PLANE('',#20616);
#900=PLANE('',#20633);
#901=PLANE('',#20636);
#902=PLANE('',#20640);
#903=PLANE('',#20650);
#904=PLANE('',#20651);
#905=PLANE('',#20658);
#906=PLANE('',#20669);
#907=PLANE('',#20670);
#908=PLANE('',#20687);
#909=PLANE('',#20690);
#910=PLANE('',#20693);
#911=PLANE('',#20704);
#912=PLANE('',#20707);
#913=PLANE('',#20711);
#914=PLANE('',#20727);
#915=PLANE('',#20728);
#916=PLANE('',#20736);
#917=PLANE('',#20750);
#918=PLANE('',#20754);
#919=PLANE('',#20778);
#920=PLANE('',#20794);
#921=PLANE('',#20797);
#922=PLANE('',#20802);
#923=PLANE('',#20805);
#924=PLANE('',#20813);
#925=PLANE('',#20815);
#926=PLANE('',#20816);
#927=PLANE('',#20820);
#928=PLANE('',#20831);
#929=PLANE('',#20842);
#930=PLANE('',#20858);
#931=PLANE('',#20877);
#932=PLANE('',#20907);
#933=PLANE('',#20923);
#934=PLANE('',#20928);
#935=PLANE('',#20931);
#936=PLANE('',#20940);
#937=PLANE('',#20958);
#938=PLANE('',#20977);
#939=PLANE('',#20978);
#940=PLANE('',#20997);
#941=PLANE('',#21008);
#942=PLANE('',#21015);
#943=PLANE('',#21016);
#944=PLANE('',#21022);
#945=PLANE('',#21048);
#946=PLANE('',#21055);
#947=PLANE('',#21058);
#948=PLANE('',#21067);
#949=PLANE('',#21078);
#950=PLANE('',#21083);
#951=PLANE('',#21089);
#952=PLANE('',#21094);
#953=PLANE('',#21114);
#954=PLANE('',#21156);
#955=PLANE('',#21164);
#956=PLANE('',#21172);
#957=PLANE('',#21180);
#958=PLANE('',#21198);
#959=PLANE('',#21256);
#960=PLANE('',#21280);
#961=PLANE('',#21284);
#962=PLANE('',#21285);
#963=PLANE('',#21286);
#964=PLANE('',#21287);
#965=PLANE('',#21288);
#966=PLANE('',#21289);
#967=PLANE('',#21290);
#968=PLANE('',#21291);
#969=PLANE('',#21292);
#970=PLANE('',#21293);
#971=PLANE('',#21306);
#972=PLANE('',#21337);
#973=PLANE('',#21396);
#974=PLANE('',#21682);
#975=PLANE('',#21700);
#976=PLANE('',#21716);
#977=PLANE('',#21717);
#978=PLANE('',#21731);
#979=PLANE('',#21741);
#980=PLANE('',#21751);
#981=PLANE('',#21769);
#982=PLANE('',#21775);
#983=PLANE('',#21776);
#984=PLANE('',#21804);
#985=PLANE('',#21805);
#986=PLANE('',#21814);
#987=PLANE('',#21815);
#988=PLANE('',#21838);
#989=PLANE('',#21852);
#990=PLANE('',#21853);
#991=PLANE('',#21869);
#992=PLANE('',#21885);
#993=PLANE('',#21886);
#994=PLANE('',#21888);
#995=PLANE('',#21902);
#996=PLANE('',#21917);
#997=PLANE('',#21926);
#998=PLANE('',#21927);
#999=PLANE('',#21944);
#1000=PLANE('',#21947);
#1001=PLANE('',#21950);
#1002=PLANE('',#21969);
#1003=PLANE('',#21978);
#1004=PLANE('',#21981);
#1005=PLANE('',#22000);
#1006=PLANE('',#22003);
#1007=PLANE('',#22004);
#1008=PLANE('',#22005);
#1009=PLANE('',#22006);
#1010=PLANE('',#22007);
#1011=PLANE('',#22008);
#1012=PLANE('',#22010);
#1013=PLANE('',#22011);
#1014=PLANE('',#22012);
#1015=PLANE('',#22013);
#1016=PLANE('',#22014);
#1017=PLANE('',#22015);
#1018=PLANE('',#22016);
#1019=PLANE('',#22017);
#1020=PLANE('',#22018);
#1021=PLANE('',#22019);
#1022=PLANE('',#22020);
#1023=PLANE('',#22021);
#1024=PLANE('',#22022);
#1025=PLANE('',#22023);
#1026=PLANE('',#22024);
#1027=PLANE('',#22025);
#1028=PLANE('',#22026);
#1029=PLANE('',#22027);
#1030=PLANE('',#22028);
#1031=PLANE('',#22029);
#1032=PLANE('',#22030);
#1033=PLANE('',#22031);
#1034=PLANE('',#22032);
#1035=PLANE('',#22033);
#1036=PLANE('',#22034);
#1037=PLANE('',#22035);
#1038=PLANE('',#22039);
#1039=PLANE('',#22040);
#1040=PLANE('',#22050);
#1041=PLANE('',#22067);
#1042=PLANE('',#22077);
#1043=PLANE('',#22084);
#1044=PLANE('',#22091);
#1045=PLANE('',#22117);
#1046=PLANE('',#22123);
#1047=PLANE('',#22159);
#1048=PLANE('',#22183);
#1049=PLANE('',#22188);
#1050=PLANE('',#22197);
#1051=PLANE('',#22210);
#1052=PLANE('',#22213);
#1053=PLANE('',#22222);
#1054=PLANE('',#22250);
#1055=PLANE('',#22254);
#1056=PLANE('',#22267);
#1057=PLANE('',#22274);
#1058=PLANE('',#22278);
#1059=PLANE('',#22291);
#1060=PLANE('',#22292);
#1061=PLANE('',#22296);
#1062=PLANE('',#22298);
#1063=PLANE('',#22301);
#1064=PLANE('',#22312);
#1065=PLANE('',#22314);
#1066=PLANE('',#22316);
#1067=PLANE('',#22328);
#1068=PLANE('',#22330);
#1069=PLANE('',#22333);
#1070=PLANE('',#22337);
#1071=PLANE('',#22340);
#1072=PLANE('',#22344);
#1073=PLANE('',#22345);
#1074=PLANE('',#22358);
#1075=PLANE('',#22363);
#1076=PLANE('',#22366);
#1077=PLANE('',#22368);
#1078=PLANE('',#22374);
#1079=PLANE('',#22375);
#1080=PLANE('',#22376);
#1081=PLANE('',#22379);
#1082=FACE_BOUND('',#2313,.T.);
#1083=FACE_BOUND('',#2757,.T.);
#1084=FACE_BOUND('',#2765,.T.);
#1085=FACE_BOUND('',#2804,.T.);
#1086=FACE_BOUND('',#2834,.T.);
#1087=FACE_BOUND('',#2854,.T.);
#1088=FACE_BOUND('',#2859,.T.);
#1089=FACE_BOUND('',#2862,.T.);
#1090=FACE_BOUND('',#2876,.T.);
#1091=FACE_BOUND('',#2877,.T.);
#1092=FACE_BOUND('',#2878,.T.);
#1093=FACE_BOUND('',#2879,.T.);
#1094=FACE_BOUND('',#2880,.T.);
#1095=FACE_BOUND('',#2881,.T.);
#1096=FACE_BOUND('',#2882,.T.);
#1097=FACE_BOUND('',#2883,.T.);
#1098=FACE_BOUND('',#2884,.T.);
#1099=FACE_BOUND('',#2885,.T.);
#1100=FACE_BOUND('',#2886,.T.);
#1101=FACE_BOUND('',#2900,.T.);
#1102=FACE_BOUND('',#2904,.T.);
#1103=FACE_BOUND('',#2908,.T.);
#1104=FACE_BOUND('',#2919,.T.);
#1105=FACE_BOUND('',#2920,.T.);
#1106=FACE_BOUND('',#2921,.T.);
#1107=FACE_BOUND('',#2922,.T.);
#1108=FACE_BOUND('',#2923,.T.);
#1109=FACE_BOUND('',#2924,.T.);
#1110=FACE_BOUND('',#2925,.T.);
#1111=FACE_BOUND('',#2941,.T.);
#1112=FACE_BOUND('',#2942,.T.);
#1113=FACE_BOUND('',#2943,.T.);
#1114=FACE_BOUND('',#2944,.T.);
#1115=FACE_BOUND('',#2974,.T.);
#1116=FACE_BOUND('',#2977,.T.);
#1117=FACE_BOUND('',#2987,.T.);
#1118=FACE_BOUND('',#3216,.T.);
#1119=FACE_BOUND('',#3223,.T.);
#1120=FACE_BOUND('',#3296,.T.);
#1121=FACE_BOUND('',#3301,.T.);
#1122=FACE_BOUND('',#3326,.T.);
#1123=FACE_BOUND('',#3342,.T.);
#1124=FACE_BOUND('',#3382,.T.);
#1125=FACE_BOUND('',#3385,.T.);
#1126=FACE_OUTER_BOUND('',#2312,.T.);
#1127=FACE_OUTER_BOUND('',#2314,.T.);
#1128=FACE_OUTER_BOUND('',#2315,.T.);
#1129=FACE_OUTER_BOUND('',#2316,.T.);
#1130=FACE_OUTER_BOUND('',#2317,.T.);
#1131=FACE_OUTER_BOUND('',#2318,.T.);
#1132=FACE_OUTER_BOUND('',#2319,.T.);
#1133=FACE_OUTER_BOUND('',#2320,.T.);
#1134=FACE_OUTER_BOUND('',#2321,.T.);
#1135=FACE_OUTER_BOUND('',#2322,.T.);
#1136=FACE_OUTER_BOUND('',#2323,.T.);
#1137=FACE_OUTER_BOUND('',#2324,.T.);
#1138=FACE_OUTER_BOUND('',#2325,.T.);
#1139=FACE_OUTER_BOUND('',#2326,.T.);
#1140=FACE_OUTER_BOUND('',#2327,.T.);
#1141=FACE_OUTER_BOUND('',#2328,.T.);
#1142=FACE_OUTER_BOUND('',#2329,.T.);
#1143=FACE_OUTER_BOUND('',#2330,.T.);
#1144=FACE_OUTER_BOUND('',#2331,.T.);
#1145=FACE_OUTER_BOUND('',#2332,.T.);
#1146=FACE_OUTER_BOUND('',#2333,.T.);
#1147=FACE_OUTER_BOUND('',#2334,.T.);
#1148=FACE_OUTER_BOUND('',#2335,.T.);
#1149=FACE_OUTER_BOUND('',#2336,.T.);
#1150=FACE_OUTER_BOUND('',#2337,.T.);
#1151=FACE_OUTER_BOUND('',#2338,.T.);
#1152=FACE_OUTER_BOUND('',#2339,.T.);
#1153=FACE_OUTER_BOUND('',#2340,.T.);
#1154=FACE_OUTER_BOUND('',#2341,.T.);
#1155=FACE_OUTER_BOUND('',#2342,.T.);
#1156=FACE_OUTER_BOUND('',#2343,.T.);
#1157=FACE_OUTER_BOUND('',#2344,.T.);
#1158=FACE_OUTER_BOUND('',#2345,.T.);
#1159=FACE_OUTER_BOUND('',#2346,.T.);
#1160=FACE_OUTER_BOUND('',#2347,.T.);
#1161=FACE_OUTER_BOUND('',#2348,.T.);
#1162=FACE_OUTER_BOUND('',#2349,.T.);
#1163=FACE_OUTER_BOUND('',#2350,.T.);
#1164=FACE_OUTER_BOUND('',#2351,.T.);
#1165=FACE_OUTER_BOUND('',#2352,.T.);
#1166=FACE_OUTER_BOUND('',#2353,.T.);
#1167=FACE_OUTER_BOUND('',#2354,.T.);
#1168=FACE_OUTER_BOUND('',#2355,.T.);
#1169=FACE_OUTER_BOUND('',#2356,.T.);
#1170=FACE_OUTER_BOUND('',#2357,.T.);
#1171=FACE_OUTER_BOUND('',#2358,.T.);
#1172=FACE_OUTER_BOUND('',#2359,.T.);
#1173=FACE_OUTER_BOUND('',#2360,.T.);
#1174=FACE_OUTER_BOUND('',#2361,.T.);
#1175=FACE_OUTER_BOUND('',#2362,.T.);
#1176=FACE_OUTER_BOUND('',#2363,.T.);
#1177=FACE_OUTER_BOUND('',#2364,.T.);
#1178=FACE_OUTER_BOUND('',#2365,.T.);
#1179=FACE_OUTER_BOUND('',#2366,.T.);
#1180=FACE_OUTER_BOUND('',#2367,.T.);
#1181=FACE_OUTER_BOUND('',#2368,.T.);
#1182=FACE_OUTER_BOUND('',#2369,.T.);
#1183=FACE_OUTER_BOUND('',#2370,.T.);
#1184=FACE_OUTER_BOUND('',#2371,.T.);
#1185=FACE_OUTER_BOUND('',#2372,.T.);
#1186=FACE_OUTER_BOUND('',#2373,.T.);
#1187=FACE_OUTER_BOUND('',#2374,.T.);
#1188=FACE_OUTER_BOUND('',#2375,.T.);
#1189=FACE_OUTER_BOUND('',#2376,.T.);
#1190=FACE_OUTER_BOUND('',#2377,.T.);
#1191=FACE_OUTER_BOUND('',#2378,.T.);
#1192=FACE_OUTER_BOUND('',#2379,.T.);
#1193=FACE_OUTER_BOUND('',#2380,.T.);
#1194=FACE_OUTER_BOUND('',#2381,.T.);
#1195=FACE_OUTER_BOUND('',#2382,.T.);
#1196=FACE_OUTER_BOUND('',#2383,.T.);
#1197=FACE_OUTER_BOUND('',#2384,.T.);
#1198=FACE_OUTER_BOUND('',#2385,.T.);
#1199=FACE_OUTER_BOUND('',#2386,.T.);
#1200=FACE_OUTER_BOUND('',#2387,.T.);
#1201=FACE_OUTER_BOUND('',#2388,.T.);
#1202=FACE_OUTER_BOUND('',#2389,.T.);
#1203=FACE_OUTER_BOUND('',#2390,.T.);
#1204=FACE_OUTER_BOUND('',#2391,.T.);
#1205=FACE_OUTER_BOUND('',#2392,.T.);
#1206=FACE_OUTER_BOUND('',#2393,.T.);
#1207=FACE_OUTER_BOUND('',#2394,.T.);
#1208=FACE_OUTER_BOUND('',#2395,.T.);
#1209=FACE_OUTER_BOUND('',#2396,.T.);
#1210=FACE_OUTER_BOUND('',#2397,.T.);
#1211=FACE_OUTER_BOUND('',#2398,.T.);
#1212=FACE_OUTER_BOUND('',#2399,.T.);
#1213=FACE_OUTER_BOUND('',#2400,.T.);
#1214=FACE_OUTER_BOUND('',#2401,.T.);
#1215=FACE_OUTER_BOUND('',#2402,.T.);
#1216=FACE_OUTER_BOUND('',#2403,.T.);
#1217=FACE_OUTER_BOUND('',#2404,.T.);
#1218=FACE_OUTER_BOUND('',#2405,.T.);
#1219=FACE_OUTER_BOUND('',#2406,.T.);
#1220=FACE_OUTER_BOUND('',#2407,.T.);
#1221=FACE_OUTER_BOUND('',#2408,.T.);
#1222=FACE_OUTER_BOUND('',#2409,.T.);
#1223=FACE_OUTER_BOUND('',#2410,.T.);
#1224=FACE_OUTER_BOUND('',#2411,.T.);
#1225=FACE_OUTER_BOUND('',#2412,.T.);
#1226=FACE_OUTER_BOUND('',#2413,.T.);
#1227=FACE_OUTER_BOUND('',#2414,.T.);
#1228=FACE_OUTER_BOUND('',#2415,.T.);
#1229=FACE_OUTER_BOUND('',#2416,.T.);
#1230=FACE_OUTER_BOUND('',#2417,.T.);
#1231=FACE_OUTER_BOUND('',#2418,.T.);
#1232=FACE_OUTER_BOUND('',#2419,.T.);
#1233=FACE_OUTER_BOUND('',#2420,.T.);
#1234=FACE_OUTER_BOUND('',#2421,.T.);
#1235=FACE_OUTER_BOUND('',#2422,.T.);
#1236=FACE_OUTER_BOUND('',#2423,.T.);
#1237=FACE_OUTER_BOUND('',#2424,.T.);
#1238=FACE_OUTER_BOUND('',#2425,.T.);
#1239=FACE_OUTER_BOUND('',#2426,.T.);
#1240=FACE_OUTER_BOUND('',#2427,.T.);
#1241=FACE_OUTER_BOUND('',#2428,.T.);
#1242=FACE_OUTER_BOUND('',#2429,.T.);
#1243=FACE_OUTER_BOUND('',#2430,.T.);
#1244=FACE_OUTER_BOUND('',#2431,.T.);
#1245=FACE_OUTER_BOUND('',#2432,.T.);
#1246=FACE_OUTER_BOUND('',#2433,.T.);
#1247=FACE_OUTER_BOUND('',#2434,.T.);
#1248=FACE_OUTER_BOUND('',#2435,.T.);
#1249=FACE_OUTER_BOUND('',#2436,.T.);
#1250=FACE_OUTER_BOUND('',#2437,.T.);
#1251=FACE_OUTER_BOUND('',#2438,.T.);
#1252=FACE_OUTER_BOUND('',#2439,.T.);
#1253=FACE_OUTER_BOUND('',#2440,.T.);
#1254=FACE_OUTER_BOUND('',#2441,.T.);
#1255=FACE_OUTER_BOUND('',#2442,.T.);
#1256=FACE_OUTER_BOUND('',#2443,.T.);
#1257=FACE_OUTER_BOUND('',#2444,.T.);
#1258=FACE_OUTER_BOUND('',#2445,.T.);
#1259=FACE_OUTER_BOUND('',#2446,.T.);
#1260=FACE_OUTER_BOUND('',#2447,.T.);
#1261=FACE_OUTER_BOUND('',#2448,.T.);
#1262=FACE_OUTER_BOUND('',#2449,.T.);
#1263=FACE_OUTER_BOUND('',#2450,.T.);
#1264=FACE_OUTER_BOUND('',#2451,.T.);
#1265=FACE_OUTER_BOUND('',#2452,.T.);
#1266=FACE_OUTER_BOUND('',#2453,.T.);
#1267=FACE_OUTER_BOUND('',#2454,.T.);
#1268=FACE_OUTER_BOUND('',#2455,.T.);
#1269=FACE_OUTER_BOUND('',#2456,.T.);
#1270=FACE_OUTER_BOUND('',#2457,.T.);
#1271=FACE_OUTER_BOUND('',#2458,.T.);
#1272=FACE_OUTER_BOUND('',#2459,.T.);
#1273=FACE_OUTER_BOUND('',#2460,.T.);
#1274=FACE_OUTER_BOUND('',#2461,.T.);
#1275=FACE_OUTER_BOUND('',#2462,.T.);
#1276=FACE_OUTER_BOUND('',#2463,.T.);
#1277=FACE_OUTER_BOUND('',#2464,.T.);
#1278=FACE_OUTER_BOUND('',#2465,.T.);
#1279=FACE_OUTER_BOUND('',#2466,.T.);
#1280=FACE_OUTER_BOUND('',#2467,.T.);
#1281=FACE_OUTER_BOUND('',#2468,.T.);
#1282=FACE_OUTER_BOUND('',#2469,.T.);
#1283=FACE_OUTER_BOUND('',#2470,.T.);
#1284=FACE_OUTER_BOUND('',#2471,.T.);
#1285=FACE_OUTER_BOUND('',#2472,.T.);
#1286=FACE_OUTER_BOUND('',#2473,.T.);
#1287=FACE_OUTER_BOUND('',#2474,.T.);
#1288=FACE_OUTER_BOUND('',#2475,.T.);
#1289=FACE_OUTER_BOUND('',#2476,.T.);
#1290=FACE_OUTER_BOUND('',#2477,.T.);
#1291=FACE_OUTER_BOUND('',#2478,.T.);
#1292=FACE_OUTER_BOUND('',#2479,.T.);
#1293=FACE_OUTER_BOUND('',#2480,.T.);
#1294=FACE_OUTER_BOUND('',#2481,.T.);
#1295=FACE_OUTER_BOUND('',#2482,.T.);
#1296=FACE_OUTER_BOUND('',#2483,.T.);
#1297=FACE_OUTER_BOUND('',#2484,.T.);
#1298=FACE_OUTER_BOUND('',#2485,.T.);
#1299=FACE_OUTER_BOUND('',#2486,.T.);
#1300=FACE_OUTER_BOUND('',#2487,.T.);
#1301=FACE_OUTER_BOUND('',#2488,.T.);
#1302=FACE_OUTER_BOUND('',#2489,.T.);
#1303=FACE_OUTER_BOUND('',#2490,.T.);
#1304=FACE_OUTER_BOUND('',#2491,.T.);
#1305=FACE_OUTER_BOUND('',#2492,.T.);
#1306=FACE_OUTER_BOUND('',#2493,.T.);
#1307=FACE_OUTER_BOUND('',#2494,.T.);
#1308=FACE_OUTER_BOUND('',#2495,.T.);
#1309=FACE_OUTER_BOUND('',#2496,.T.);
#1310=FACE_OUTER_BOUND('',#2497,.T.);
#1311=FACE_OUTER_BOUND('',#2498,.T.);
#1312=FACE_OUTER_BOUND('',#2499,.T.);
#1313=FACE_OUTER_BOUND('',#2500,.T.);
#1314=FACE_OUTER_BOUND('',#2501,.T.);
#1315=FACE_OUTER_BOUND('',#2502,.T.);
#1316=FACE_OUTER_BOUND('',#2503,.T.);
#1317=FACE_OUTER_BOUND('',#2504,.T.);
#1318=FACE_OUTER_BOUND('',#2505,.T.);
#1319=FACE_OUTER_BOUND('',#2506,.T.);
#1320=FACE_OUTER_BOUND('',#2507,.T.);
#1321=FACE_OUTER_BOUND('',#2508,.T.);
#1322=FACE_OUTER_BOUND('',#2509,.T.);
#1323=FACE_OUTER_BOUND('',#2510,.T.);
#1324=FACE_OUTER_BOUND('',#2511,.T.);
#1325=FACE_OUTER_BOUND('',#2512,.T.);
#1326=FACE_OUTER_BOUND('',#2513,.T.);
#1327=FACE_OUTER_BOUND('',#2514,.T.);
#1328=FACE_OUTER_BOUND('',#2515,.T.);
#1329=FACE_OUTER_BOUND('',#2516,.T.);
#1330=FACE_OUTER_BOUND('',#2517,.T.);
#1331=FACE_OUTER_BOUND('',#2518,.T.);
#1332=FACE_OUTER_BOUND('',#2519,.T.);
#1333=FACE_OUTER_BOUND('',#2520,.T.);
#1334=FACE_OUTER_BOUND('',#2521,.T.);
#1335=FACE_OUTER_BOUND('',#2522,.T.);
#1336=FACE_OUTER_BOUND('',#2523,.T.);
#1337=FACE_OUTER_BOUND('',#2524,.T.);
#1338=FACE_OUTER_BOUND('',#2525,.T.);
#1339=FACE_OUTER_BOUND('',#2526,.T.);
#1340=FACE_OUTER_BOUND('',#2527,.T.);
#1341=FACE_OUTER_BOUND('',#2528,.T.);
#1342=FACE_OUTER_BOUND('',#2529,.T.);
#1343=FACE_OUTER_BOUND('',#2530,.T.);
#1344=FACE_OUTER_BOUND('',#2531,.T.);
#1345=FACE_OUTER_BOUND('',#2532,.T.);
#1346=FACE_OUTER_BOUND('',#2533,.T.);
#1347=FACE_OUTER_BOUND('',#2534,.T.);
#1348=FACE_OUTER_BOUND('',#2535,.T.);
#1349=FACE_OUTER_BOUND('',#2536,.T.);
#1350=FACE_OUTER_BOUND('',#2537,.T.);
#1351=FACE_OUTER_BOUND('',#2538,.T.);
#1352=FACE_OUTER_BOUND('',#2539,.T.);
#1353=FACE_OUTER_BOUND('',#2540,.T.);
#1354=FACE_OUTER_BOUND('',#2541,.T.);
#1355=FACE_OUTER_BOUND('',#2542,.T.);
#1356=FACE_OUTER_BOUND('',#2543,.T.);
#1357=FACE_OUTER_BOUND('',#2544,.T.);
#1358=FACE_OUTER_BOUND('',#2545,.T.);
#1359=FACE_OUTER_BOUND('',#2546,.T.);
#1360=FACE_OUTER_BOUND('',#2547,.T.);
#1361=FACE_OUTER_BOUND('',#2548,.T.);
#1362=FACE_OUTER_BOUND('',#2549,.T.);
#1363=FACE_OUTER_BOUND('',#2550,.T.);
#1364=FACE_OUTER_BOUND('',#2551,.T.);
#1365=FACE_OUTER_BOUND('',#2552,.T.);
#1366=FACE_OUTER_BOUND('',#2553,.T.);
#1367=FACE_OUTER_BOUND('',#2554,.T.);
#1368=FACE_OUTER_BOUND('',#2555,.T.);
#1369=FACE_OUTER_BOUND('',#2556,.T.);
#1370=FACE_OUTER_BOUND('',#2557,.T.);
#1371=FACE_OUTER_BOUND('',#2558,.T.);
#1372=FACE_OUTER_BOUND('',#2559,.T.);
#1373=FACE_OUTER_BOUND('',#2560,.T.);
#1374=FACE_OUTER_BOUND('',#2561,.T.);
#1375=FACE_OUTER_BOUND('',#2562,.T.);
#1376=FACE_OUTER_BOUND('',#2563,.T.);
#1377=FACE_OUTER_BOUND('',#2564,.T.);
#1378=FACE_OUTER_BOUND('',#2565,.T.);
#1379=FACE_OUTER_BOUND('',#2566,.T.);
#1380=FACE_OUTER_BOUND('',#2567,.T.);
#1381=FACE_OUTER_BOUND('',#2568,.T.);
#1382=FACE_OUTER_BOUND('',#2569,.T.);
#1383=FACE_OUTER_BOUND('',#2570,.T.);
#1384=FACE_OUTER_BOUND('',#2571,.T.);
#1385=FACE_OUTER_BOUND('',#2572,.T.);
#1386=FACE_OUTER_BOUND('',#2573,.T.);
#1387=FACE_OUTER_BOUND('',#2574,.T.);
#1388=FACE_OUTER_BOUND('',#2575,.T.);
#1389=FACE_OUTER_BOUND('',#2576,.T.);
#1390=FACE_OUTER_BOUND('',#2577,.T.);
#1391=FACE_OUTER_BOUND('',#2578,.T.);
#1392=FACE_OUTER_BOUND('',#2579,.T.);
#1393=FACE_OUTER_BOUND('',#2580,.T.);
#1394=FACE_OUTER_BOUND('',#2581,.T.);
#1395=FACE_OUTER_BOUND('',#2582,.T.);
#1396=FACE_OUTER_BOUND('',#2583,.T.);
#1397=FACE_OUTER_BOUND('',#2584,.T.);
#1398=FACE_OUTER_BOUND('',#2585,.T.);
#1399=FACE_OUTER_BOUND('',#2586,.T.);
#1400=FACE_OUTER_BOUND('',#2587,.T.);
#1401=FACE_OUTER_BOUND('',#2588,.T.);
#1402=FACE_OUTER_BOUND('',#2589,.T.);
#1403=FACE_OUTER_BOUND('',#2590,.T.);
#1404=FACE_OUTER_BOUND('',#2591,.T.);
#1405=FACE_OUTER_BOUND('',#2592,.T.);
#1406=FACE_OUTER_BOUND('',#2593,.T.);
#1407=FACE_OUTER_BOUND('',#2594,.T.);
#1408=FACE_OUTER_BOUND('',#2595,.T.);
#1409=FACE_OUTER_BOUND('',#2596,.T.);
#1410=FACE_OUTER_BOUND('',#2597,.T.);
#1411=FACE_OUTER_BOUND('',#2598,.T.);
#1412=FACE_OUTER_BOUND('',#2599,.T.);
#1413=FACE_OUTER_BOUND('',#2600,.T.);
#1414=FACE_OUTER_BOUND('',#2601,.T.);
#1415=FACE_OUTER_BOUND('',#2602,.T.);
#1416=FACE_OUTER_BOUND('',#2603,.T.);
#1417=FACE_OUTER_BOUND('',#2604,.T.);
#1418=FACE_OUTER_BOUND('',#2605,.T.);
#1419=FACE_OUTER_BOUND('',#2606,.T.);
#1420=FACE_OUTER_BOUND('',#2607,.T.);
#1421=FACE_OUTER_BOUND('',#2608,.T.);
#1422=FACE_OUTER_BOUND('',#2609,.T.);
#1423=FACE_OUTER_BOUND('',#2610,.T.);
#1424=FACE_OUTER_BOUND('',#2611,.T.);
#1425=FACE_OUTER_BOUND('',#2612,.T.);
#1426=FACE_OUTER_BOUND('',#2613,.T.);
#1427=FACE_OUTER_BOUND('',#2614,.T.);
#1428=FACE_OUTER_BOUND('',#2615,.T.);
#1429=FACE_OUTER_BOUND('',#2616,.T.);
#1430=FACE_OUTER_BOUND('',#2617,.T.);
#1431=FACE_OUTER_BOUND('',#2618,.T.);
#1432=FACE_OUTER_BOUND('',#2619,.T.);
#1433=FACE_OUTER_BOUND('',#2620,.T.);
#1434=FACE_OUTER_BOUND('',#2621,.T.);
#1435=FACE_OUTER_BOUND('',#2622,.T.);
#1436=FACE_OUTER_BOUND('',#2623,.T.);
#1437=FACE_OUTER_BOUND('',#2624,.T.);
#1438=FACE_OUTER_BOUND('',#2625,.T.);
#1439=FACE_OUTER_BOUND('',#2626,.T.);
#1440=FACE_OUTER_BOUND('',#2627,.T.);
#1441=FACE_OUTER_BOUND('',#2628,.T.);
#1442=FACE_OUTER_BOUND('',#2629,.T.);
#1443=FACE_OUTER_BOUND('',#2630,.T.);
#1444=FACE_OUTER_BOUND('',#2631,.T.);
#1445=FACE_OUTER_BOUND('',#2632,.T.);
#1446=FACE_OUTER_BOUND('',#2633,.T.);
#1447=FACE_OUTER_BOUND('',#2634,.T.);
#1448=FACE_OUTER_BOUND('',#2635,.T.);
#1449=FACE_OUTER_BOUND('',#2636,.T.);
#1450=FACE_OUTER_BOUND('',#2637,.T.);
#1451=FACE_OUTER_BOUND('',#2638,.T.);
#1452=FACE_OUTER_BOUND('',#2639,.T.);
#1453=FACE_OUTER_BOUND('',#2640,.T.);
#1454=FACE_OUTER_BOUND('',#2641,.T.);
#1455=FACE_OUTER_BOUND('',#2642,.T.);
#1456=FACE_OUTER_BOUND('',#2643,.T.);
#1457=FACE_OUTER_BOUND('',#2644,.T.);
#1458=FACE_OUTER_BOUND('',#2645,.T.);
#1459=FACE_OUTER_BOUND('',#2646,.T.);
#1460=FACE_OUTER_BOUND('',#2647,.T.);
#1461=FACE_OUTER_BOUND('',#2648,.T.);
#1462=FACE_OUTER_BOUND('',#2649,.T.);
#1463=FACE_OUTER_BOUND('',#2650,.T.);
#1464=FACE_OUTER_BOUND('',#2651,.T.);
#1465=FACE_OUTER_BOUND('',#2652,.T.);
#1466=FACE_OUTER_BOUND('',#2653,.T.);
#1467=FACE_OUTER_BOUND('',#2654,.T.);
#1468=FACE_OUTER_BOUND('',#2655,.T.);
#1469=FACE_OUTER_BOUND('',#2656,.T.);
#1470=FACE_OUTER_BOUND('',#2657,.T.);
#1471=FACE_OUTER_BOUND('',#2658,.T.);
#1472=FACE_OUTER_BOUND('',#2659,.T.);
#1473=FACE_OUTER_BOUND('',#2660,.T.);
#1474=FACE_OUTER_BOUND('',#2661,.T.);
#1475=FACE_OUTER_BOUND('',#2662,.T.);
#1476=FACE_OUTER_BOUND('',#2663,.T.);
#1477=FACE_OUTER_BOUND('',#2664,.T.);
#1478=FACE_OUTER_BOUND('',#2665,.T.);
#1479=FACE_OUTER_BOUND('',#2666,.T.);
#1480=FACE_OUTER_BOUND('',#2667,.T.);
#1481=FACE_OUTER_BOUND('',#2668,.T.);
#1482=FACE_OUTER_BOUND('',#2669,.T.);
#1483=FACE_OUTER_BOUND('',#2670,.T.);
#1484=FACE_OUTER_BOUND('',#2671,.T.);
#1485=FACE_OUTER_BOUND('',#2672,.T.);
#1486=FACE_OUTER_BOUND('',#2673,.T.);
#1487=FACE_OUTER_BOUND('',#2674,.T.);
#1488=FACE_OUTER_BOUND('',#2675,.T.);
#1489=FACE_OUTER_BOUND('',#2676,.T.);
#1490=FACE_OUTER_BOUND('',#2677,.T.);
#1491=FACE_OUTER_BOUND('',#2678,.T.);
#1492=FACE_OUTER_BOUND('',#2679,.T.);
#1493=FACE_OUTER_BOUND('',#2680,.T.);
#1494=FACE_OUTER_BOUND('',#2681,.T.);
#1495=FACE_OUTER_BOUND('',#2682,.T.);
#1496=FACE_OUTER_BOUND('',#2683,.T.);
#1497=FACE_OUTER_BOUND('',#2684,.T.);
#1498=FACE_OUTER_BOUND('',#2685,.T.);
#1499=FACE_OUTER_BOUND('',#2686,.T.);
#1500=FACE_OUTER_BOUND('',#2687,.T.);
#1501=FACE_OUTER_BOUND('',#2688,.T.);
#1502=FACE_OUTER_BOUND('',#2689,.T.);
#1503=FACE_OUTER_BOUND('',#2690,.T.);
#1504=FACE_OUTER_BOUND('',#2691,.T.);
#1505=FACE_OUTER_BOUND('',#2692,.T.);
#1506=FACE_OUTER_BOUND('',#2693,.T.);
#1507=FACE_OUTER_BOUND('',#2694,.T.);
#1508=FACE_OUTER_BOUND('',#2695,.T.);
#1509=FACE_OUTER_BOUND('',#2696,.T.);
#1510=FACE_OUTER_BOUND('',#2697,.T.);
#1511=FACE_OUTER_BOUND('',#2698,.T.);
#1512=FACE_OUTER_BOUND('',#2699,.T.);
#1513=FACE_OUTER_BOUND('',#2700,.T.);
#1514=FACE_OUTER_BOUND('',#2701,.T.);
#1515=FACE_OUTER_BOUND('',#2702,.T.);
#1516=FACE_OUTER_BOUND('',#2703,.T.);
#1517=FACE_OUTER_BOUND('',#2704,.T.);
#1518=FACE_OUTER_BOUND('',#2705,.T.);
#1519=FACE_OUTER_BOUND('',#2706,.T.);
#1520=FACE_OUTER_BOUND('',#2707,.T.);
#1521=FACE_OUTER_BOUND('',#2708,.T.);
#1522=FACE_OUTER_BOUND('',#2709,.T.);
#1523=FACE_OUTER_BOUND('',#2710,.T.);
#1524=FACE_OUTER_BOUND('',#2711,.T.);
#1525=FACE_OUTER_BOUND('',#2712,.T.);
#1526=FACE_OUTER_BOUND('',#2713,.T.);
#1527=FACE_OUTER_BOUND('',#2714,.T.);
#1528=FACE_OUTER_BOUND('',#2715,.T.);
#1529=FACE_OUTER_BOUND('',#2716,.T.);
#1530=FACE_OUTER_BOUND('',#2717,.T.);
#1531=FACE_OUTER_BOUND('',#2718,.T.);
#1532=FACE_OUTER_BOUND('',#2719,.T.);
#1533=FACE_OUTER_BOUND('',#2720,.T.);
#1534=FACE_OUTER_BOUND('',#2721,.T.);
#1535=FACE_OUTER_BOUND('',#2722,.T.);
#1536=FACE_OUTER_BOUND('',#2723,.T.);
#1537=FACE_OUTER_BOUND('',#2724,.T.);
#1538=FACE_OUTER_BOUND('',#2725,.T.);
#1539=FACE_OUTER_BOUND('',#2726,.T.);
#1540=FACE_OUTER_BOUND('',#2727,.T.);
#1541=FACE_OUTER_BOUND('',#2728,.T.);
#1542=FACE_OUTER_BOUND('',#2729,.T.);
#1543=FACE_OUTER_BOUND('',#2730,.T.);
#1544=FACE_OUTER_BOUND('',#2731,.T.);
#1545=FACE_OUTER_BOUND('',#2732,.T.);
#1546=FACE_OUTER_BOUND('',#2733,.T.);
#1547=FACE_OUTER_BOUND('',#2734,.T.);
#1548=FACE_OUTER_BOUND('',#2735,.T.);
#1549=FACE_OUTER_BOUND('',#2736,.T.);
#1550=FACE_OUTER_BOUND('',#2737,.T.);
#1551=FACE_OUTER_BOUND('',#2738,.T.);
#1552=FACE_OUTER_BOUND('',#2739,.T.);
#1553=FACE_OUTER_BOUND('',#2740,.T.);
#1554=FACE_OUTER_BOUND('',#2741,.T.);
#1555=FACE_OUTER_BOUND('',#2742,.T.);
#1556=FACE_OUTER_BOUND('',#2743,.T.);
#1557=FACE_OUTER_BOUND('',#2744,.T.);
#1558=FACE_OUTER_BOUND('',#2745,.T.);
#1559=FACE_OUTER_BOUND('',#2746,.T.);
#1560=FACE_OUTER_BOUND('',#2747,.T.);
#1561=FACE_OUTER_BOUND('',#2748,.T.);
#1562=FACE_OUTER_BOUND('',#2749,.T.);
#1563=FACE_OUTER_BOUND('',#2750,.T.);
#1564=FACE_OUTER_BOUND('',#2751,.T.);
#1565=FACE_OUTER_BOUND('',#2752,.T.);
#1566=FACE_OUTER_BOUND('',#2753,.T.);
#1567=FACE_OUTER_BOUND('',#2754,.T.);
#1568=FACE_OUTER_BOUND('',#2755,.T.);
#1569=FACE_OUTER_BOUND('',#2756,.T.);
#1570=FACE_OUTER_BOUND('',#2758,.T.);
#1571=FACE_OUTER_BOUND('',#2759,.T.);
#1572=FACE_OUTER_BOUND('',#2760,.T.);
#1573=FACE_OUTER_BOUND('',#2761,.T.);
#1574=FACE_OUTER_BOUND('',#2762,.T.);
#1575=FACE_OUTER_BOUND('',#2763,.T.);
#1576=FACE_OUTER_BOUND('',#2764,.T.);
#1577=FACE_OUTER_BOUND('',#2766,.T.);
#1578=FACE_OUTER_BOUND('',#2767,.T.);
#1579=FACE_OUTER_BOUND('',#2768,.T.);
#1580=FACE_OUTER_BOUND('',#2769,.T.);
#1581=FACE_OUTER_BOUND('',#2770,.T.);
#1582=FACE_OUTER_BOUND('',#2771,.T.);
#1583=FACE_OUTER_BOUND('',#2772,.T.);
#1584=FACE_OUTER_BOUND('',#2773,.T.);
#1585=FACE_OUTER_BOUND('',#2774,.T.);
#1586=FACE_OUTER_BOUND('',#2775,.T.);
#1587=FACE_OUTER_BOUND('',#2776,.T.);
#1588=FACE_OUTER_BOUND('',#2777,.T.);
#1589=FACE_OUTER_BOUND('',#2778,.T.);
#1590=FACE_OUTER_BOUND('',#2779,.T.);
#1591=FACE_OUTER_BOUND('',#2780,.T.);
#1592=FACE_OUTER_BOUND('',#2781,.T.);
#1593=FACE_OUTER_BOUND('',#2782,.T.);
#1594=FACE_OUTER_BOUND('',#2783,.T.);
#1595=FACE_OUTER_BOUND('',#2784,.T.);
#1596=FACE_OUTER_BOUND('',#2785,.T.);
#1597=FACE_OUTER_BOUND('',#2786,.T.);
#1598=FACE_OUTER_BOUND('',#2787,.T.);
#1599=FACE_OUTER_BOUND('',#2788,.T.);
#1600=FACE_OUTER_BOUND('',#2789,.T.);
#1601=FACE_OUTER_BOUND('',#2790,.T.);
#1602=FACE_OUTER_BOUND('',#2791,.T.);
#1603=FACE_OUTER_BOUND('',#2792,.T.);
#1604=FACE_OUTER_BOUND('',#2793,.T.);
#1605=FACE_OUTER_BOUND('',#2794,.T.);
#1606=FACE_OUTER_BOUND('',#2795,.T.);
#1607=FACE_OUTER_BOUND('',#2796,.T.);
#1608=FACE_OUTER_BOUND('',#2797,.T.);
#1609=FACE_OUTER_BOUND('',#2798,.T.);
#1610=FACE_OUTER_BOUND('',#2799,.T.);
#1611=FACE_OUTER_BOUND('',#2800,.T.);
#1612=FACE_OUTER_BOUND('',#2801,.T.);
#1613=FACE_OUTER_BOUND('',#2802,.T.);
#1614=FACE_OUTER_BOUND('',#2803,.T.);
#1615=FACE_OUTER_BOUND('',#2805,.T.);
#1616=FACE_OUTER_BOUND('',#2806,.T.);
#1617=FACE_OUTER_BOUND('',#2807,.T.);
#1618=FACE_OUTER_BOUND('',#2808,.T.);
#1619=FACE_OUTER_BOUND('',#2809,.T.);
#1620=FACE_OUTER_BOUND('',#2810,.T.);
#1621=FACE_OUTER_BOUND('',#2811,.T.);
#1622=FACE_OUTER_BOUND('',#2812,.T.);
#1623=FACE_OUTER_BOUND('',#2813,.T.);
#1624=FACE_OUTER_BOUND('',#2814,.T.);
#1625=FACE_OUTER_BOUND('',#2815,.T.);
#1626=FACE_OUTER_BOUND('',#2816,.T.);
#1627=FACE_OUTER_BOUND('',#2817,.T.);
#1628=FACE_OUTER_BOUND('',#2818,.T.);
#1629=FACE_OUTER_BOUND('',#2819,.T.);
#1630=FACE_OUTER_BOUND('',#2820,.T.);
#1631=FACE_OUTER_BOUND('',#2821,.T.);
#1632=FACE_OUTER_BOUND('',#2822,.T.);
#1633=FACE_OUTER_BOUND('',#2823,.T.);
#1634=FACE_OUTER_BOUND('',#2824,.T.);
#1635=FACE_OUTER_BOUND('',#2825,.T.);
#1636=FACE_OUTER_BOUND('',#2826,.T.);
#1637=FACE_OUTER_BOUND('',#2827,.T.);
#1638=FACE_OUTER_BOUND('',#2828,.T.);
#1639=FACE_OUTER_BOUND('',#2829,.T.);
#1640=FACE_OUTER_BOUND('',#2830,.T.);
#1641=FACE_OUTER_BOUND('',#2831,.T.);
#1642=FACE_OUTER_BOUND('',#2832,.T.);
#1643=FACE_OUTER_BOUND('',#2833,.T.);
#1644=FACE_OUTER_BOUND('',#2835,.T.);
#1645=FACE_OUTER_BOUND('',#2836,.T.);
#1646=FACE_OUTER_BOUND('',#2837,.T.);
#1647=FACE_OUTER_BOUND('',#2838,.T.);
#1648=FACE_OUTER_BOUND('',#2839,.T.);
#1649=FACE_OUTER_BOUND('',#2840,.T.);
#1650=FACE_OUTER_BOUND('',#2841,.T.);
#1651=FACE_OUTER_BOUND('',#2842,.T.);
#1652=FACE_OUTER_BOUND('',#2843,.T.);
#1653=FACE_OUTER_BOUND('',#2844,.T.);
#1654=FACE_OUTER_BOUND('',#2845,.T.);
#1655=FACE_OUTER_BOUND('',#2846,.T.);
#1656=FACE_OUTER_BOUND('',#2847,.T.);
#1657=FACE_OUTER_BOUND('',#2848,.T.);
#1658=FACE_OUTER_BOUND('',#2849,.T.);
#1659=FACE_OUTER_BOUND('',#2850,.T.);
#1660=FACE_OUTER_BOUND('',#2851,.T.);
#1661=FACE_OUTER_BOUND('',#2852,.T.);
#1662=FACE_OUTER_BOUND('',#2853,.T.);
#1663=FACE_OUTER_BOUND('',#2855,.T.);
#1664=FACE_OUTER_BOUND('',#2856,.T.);
#1665=FACE_OUTER_BOUND('',#2857,.T.);
#1666=FACE_OUTER_BOUND('',#2858,.T.);
#1667=FACE_OUTER_BOUND('',#2860,.T.);
#1668=FACE_OUTER_BOUND('',#2861,.T.);
#1669=FACE_OUTER_BOUND('',#2863,.T.);
#1670=FACE_OUTER_BOUND('',#2864,.T.);
#1671=FACE_OUTER_BOUND('',#2865,.T.);
#1672=FACE_OUTER_BOUND('',#2866,.T.);
#1673=FACE_OUTER_BOUND('',#2867,.T.);
#1674=FACE_OUTER_BOUND('',#2868,.T.);
#1675=FACE_OUTER_BOUND('',#2869,.T.);
#1676=FACE_OUTER_BOUND('',#2870,.T.);
#1677=FACE_OUTER_BOUND('',#2871,.T.);
#1678=FACE_OUTER_BOUND('',#2872,.T.);
#1679=FACE_OUTER_BOUND('',#2873,.T.);
#1680=FACE_OUTER_BOUND('',#2874,.T.);
#1681=FACE_OUTER_BOUND('',#2875,.T.);
#1682=FACE_OUTER_BOUND('',#2887,.T.);
#1683=FACE_OUTER_BOUND('',#2888,.T.);
#1684=FACE_OUTER_BOUND('',#2889,.T.);
#1685=FACE_OUTER_BOUND('',#2890,.T.);
#1686=FACE_OUTER_BOUND('',#2891,.T.);
#1687=FACE_OUTER_BOUND('',#2892,.T.);
#1688=FACE_OUTER_BOUND('',#2893,.T.);
#1689=FACE_OUTER_BOUND('',#2894,.T.);
#1690=FACE_OUTER_BOUND('',#2895,.T.);
#1691=FACE_OUTER_BOUND('',#2896,.T.);
#1692=FACE_OUTER_BOUND('',#2897,.T.);
#1693=FACE_OUTER_BOUND('',#2898,.T.);
#1694=FACE_OUTER_BOUND('',#2899,.T.);
#1695=FACE_OUTER_BOUND('',#2901,.T.);
#1696=FACE_OUTER_BOUND('',#2902,.T.);
#1697=FACE_OUTER_BOUND('',#2903,.T.);
#1698=FACE_OUTER_BOUND('',#2905,.T.);
#1699=FACE_OUTER_BOUND('',#2906,.T.);
#1700=FACE_OUTER_BOUND('',#2907,.T.);
#1701=FACE_OUTER_BOUND('',#2909,.T.);
#1702=FACE_OUTER_BOUND('',#2910,.T.);
#1703=FACE_OUTER_BOUND('',#2911,.T.);
#1704=FACE_OUTER_BOUND('',#2912,.T.);
#1705=FACE_OUTER_BOUND('',#2913,.T.);
#1706=FACE_OUTER_BOUND('',#2914,.T.);
#1707=FACE_OUTER_BOUND('',#2915,.T.);
#1708=FACE_OUTER_BOUND('',#2916,.T.);
#1709=FACE_OUTER_BOUND('',#2917,.T.);
#1710=FACE_OUTER_BOUND('',#2918,.T.);
#1711=FACE_OUTER_BOUND('',#2926,.T.);
#1712=FACE_OUTER_BOUND('',#2927,.T.);
#1713=FACE_OUTER_BOUND('',#2928,.T.);
#1714=FACE_OUTER_BOUND('',#2929,.T.);
#1715=FACE_OUTER_BOUND('',#2930,.T.);
#1716=FACE_OUTER_BOUND('',#2931,.T.);
#1717=FACE_OUTER_BOUND('',#2932,.T.);
#1718=FACE_OUTER_BOUND('',#2933,.T.);
#1719=FACE_OUTER_BOUND('',#2934,.T.);
#1720=FACE_OUTER_BOUND('',#2935,.T.);
#1721=FACE_OUTER_BOUND('',#2936,.T.);
#1722=FACE_OUTER_BOUND('',#2937,.T.);
#1723=FACE_OUTER_BOUND('',#2938,.T.);
#1724=FACE_OUTER_BOUND('',#2939,.T.);
#1725=FACE_OUTER_BOUND('',#2940,.T.);
#1726=FACE_OUTER_BOUND('',#2945,.T.);
#1727=FACE_OUTER_BOUND('',#2946,.T.);
#1728=FACE_OUTER_BOUND('',#2947,.T.);
#1729=FACE_OUTER_BOUND('',#2948,.T.);
#1730=FACE_OUTER_BOUND('',#2949,.T.);
#1731=FACE_OUTER_BOUND('',#2950,.T.);
#1732=FACE_OUTER_BOUND('',#2951,.T.);
#1733=FACE_OUTER_BOUND('',#2952,.T.);
#1734=FACE_OUTER_BOUND('',#2953,.T.);
#1735=FACE_OUTER_BOUND('',#2954,.T.);
#1736=FACE_OUTER_BOUND('',#2955,.T.);
#1737=FACE_OUTER_BOUND('',#2956,.T.);
#1738=FACE_OUTER_BOUND('',#2957,.T.);
#1739=FACE_OUTER_BOUND('',#2958,.T.);
#1740=FACE_OUTER_BOUND('',#2959,.T.);
#1741=FACE_OUTER_BOUND('',#2960,.T.);
#1742=FACE_OUTER_BOUND('',#2961,.T.);
#1743=FACE_OUTER_BOUND('',#2962,.T.);
#1744=FACE_OUTER_BOUND('',#2963,.T.);
#1745=FACE_OUTER_BOUND('',#2964,.T.);
#1746=FACE_OUTER_BOUND('',#2965,.T.);
#1747=FACE_OUTER_BOUND('',#2966,.T.);
#1748=FACE_OUTER_BOUND('',#2967,.T.);
#1749=FACE_OUTER_BOUND('',#2968,.T.);
#1750=FACE_OUTER_BOUND('',#2969,.T.);
#1751=FACE_OUTER_BOUND('',#2970,.T.);
#1752=FACE_OUTER_BOUND('',#2971,.T.);
#1753=FACE_OUTER_BOUND('',#2972,.T.);
#1754=FACE_OUTER_BOUND('',#2973,.T.);
#1755=FACE_OUTER_BOUND('',#2975,.T.);
#1756=FACE_OUTER_BOUND('',#2976,.T.);
#1757=FACE_OUTER_BOUND('',#2978,.T.);
#1758=FACE_OUTER_BOUND('',#2979,.T.);
#1759=FACE_OUTER_BOUND('',#2980,.T.);
#1760=FACE_OUTER_BOUND('',#2981,.T.);
#1761=FACE_OUTER_BOUND('',#2982,.T.);
#1762=FACE_OUTER_BOUND('',#2983,.T.);
#1763=FACE_OUTER_BOUND('',#2984,.T.);
#1764=FACE_OUTER_BOUND('',#2985,.T.);
#1765=FACE_OUTER_BOUND('',#2986,.T.);
#1766=FACE_OUTER_BOUND('',#2988,.T.);
#1767=FACE_OUTER_BOUND('',#2989,.T.);
#1768=FACE_OUTER_BOUND('',#2990,.T.);
#1769=FACE_OUTER_BOUND('',#2991,.T.);
#1770=FACE_OUTER_BOUND('',#2992,.T.);
#1771=FACE_OUTER_BOUND('',#2993,.T.);
#1772=FACE_OUTER_BOUND('',#2994,.T.);
#1773=FACE_OUTER_BOUND('',#2995,.T.);
#1774=FACE_OUTER_BOUND('',#2996,.T.);
#1775=FACE_OUTER_BOUND('',#2997,.T.);
#1776=FACE_OUTER_BOUND('',#2998,.T.);
#1777=FACE_OUTER_BOUND('',#2999,.T.);
#1778=FACE_OUTER_BOUND('',#3000,.T.);
#1779=FACE_OUTER_BOUND('',#3001,.T.);
#1780=FACE_OUTER_BOUND('',#3002,.T.);
#1781=FACE_OUTER_BOUND('',#3003,.T.);
#1782=FACE_OUTER_BOUND('',#3004,.T.);
#1783=FACE_OUTER_BOUND('',#3005,.T.);
#1784=FACE_OUTER_BOUND('',#3006,.T.);
#1785=FACE_OUTER_BOUND('',#3007,.T.);
#1786=FACE_OUTER_BOUND('',#3008,.T.);
#1787=FACE_OUTER_BOUND('',#3009,.T.);
#1788=FACE_OUTER_BOUND('',#3010,.T.);
#1789=FACE_OUTER_BOUND('',#3011,.T.);
#1790=FACE_OUTER_BOUND('',#3012,.T.);
#1791=FACE_OUTER_BOUND('',#3013,.T.);
#1792=FACE_OUTER_BOUND('',#3014,.T.);
#1793=FACE_OUTER_BOUND('',#3015,.T.);
#1794=FACE_OUTER_BOUND('',#3016,.T.);
#1795=FACE_OUTER_BOUND('',#3017,.T.);
#1796=FACE_OUTER_BOUND('',#3018,.T.);
#1797=FACE_OUTER_BOUND('',#3019,.T.);
#1798=FACE_OUTER_BOUND('',#3020,.T.);
#1799=FACE_OUTER_BOUND('',#3021,.T.);
#1800=FACE_OUTER_BOUND('',#3022,.T.);
#1801=FACE_OUTER_BOUND('',#3023,.T.);
#1802=FACE_OUTER_BOUND('',#3024,.T.);
#1803=FACE_OUTER_BOUND('',#3025,.T.);
#1804=FACE_OUTER_BOUND('',#3026,.T.);
#1805=FACE_OUTER_BOUND('',#3027,.T.);
#1806=FACE_OUTER_BOUND('',#3028,.T.);
#1807=FACE_OUTER_BOUND('',#3029,.T.);
#1808=FACE_OUTER_BOUND('',#3030,.T.);
#1809=FACE_OUTER_BOUND('',#3031,.T.);
#1810=FACE_OUTER_BOUND('',#3032,.T.);
#1811=FACE_OUTER_BOUND('',#3033,.T.);
#1812=FACE_OUTER_BOUND('',#3034,.T.);
#1813=FACE_OUTER_BOUND('',#3035,.T.);
#1814=FACE_OUTER_BOUND('',#3036,.T.);
#1815=FACE_OUTER_BOUND('',#3037,.T.);
#1816=FACE_OUTER_BOUND('',#3038,.T.);
#1817=FACE_OUTER_BOUND('',#3039,.T.);
#1818=FACE_OUTER_BOUND('',#3040,.T.);
#1819=FACE_OUTER_BOUND('',#3041,.T.);
#1820=FACE_OUTER_BOUND('',#3042,.T.);
#1821=FACE_OUTER_BOUND('',#3043,.T.);
#1822=FACE_OUTER_BOUND('',#3044,.T.);
#1823=FACE_OUTER_BOUND('',#3045,.T.);
#1824=FACE_OUTER_BOUND('',#3046,.T.);
#1825=FACE_OUTER_BOUND('',#3047,.T.);
#1826=FACE_OUTER_BOUND('',#3048,.T.);
#1827=FACE_OUTER_BOUND('',#3049,.T.);
#1828=FACE_OUTER_BOUND('',#3050,.T.);
#1829=FACE_OUTER_BOUND('',#3051,.T.);
#1830=FACE_OUTER_BOUND('',#3052,.T.);
#1831=FACE_OUTER_BOUND('',#3053,.T.);
#1832=FACE_OUTER_BOUND('',#3054,.T.);
#1833=FACE_OUTER_BOUND('',#3055,.T.);
#1834=FACE_OUTER_BOUND('',#3056,.T.);
#1835=FACE_OUTER_BOUND('',#3057,.T.);
#1836=FACE_OUTER_BOUND('',#3058,.T.);
#1837=FACE_OUTER_BOUND('',#3059,.T.);
#1838=FACE_OUTER_BOUND('',#3060,.T.);
#1839=FACE_OUTER_BOUND('',#3061,.T.);
#1840=FACE_OUTER_BOUND('',#3062,.T.);
#1841=FACE_OUTER_BOUND('',#3063,.T.);
#1842=FACE_OUTER_BOUND('',#3064,.T.);
#1843=FACE_OUTER_BOUND('',#3065,.T.);
#1844=FACE_OUTER_BOUND('',#3066,.T.);
#1845=FACE_OUTER_BOUND('',#3067,.T.);
#1846=FACE_OUTER_BOUND('',#3068,.T.);
#1847=FACE_OUTER_BOUND('',#3069,.T.);
#1848=FACE_OUTER_BOUND('',#3070,.T.);
#1849=FACE_OUTER_BOUND('',#3071,.T.);
#1850=FACE_OUTER_BOUND('',#3072,.T.);
#1851=FACE_OUTER_BOUND('',#3073,.T.);
#1852=FACE_OUTER_BOUND('',#3074,.T.);
#1853=FACE_OUTER_BOUND('',#3075,.T.);
#1854=FACE_OUTER_BOUND('',#3076,.T.);
#1855=FACE_OUTER_BOUND('',#3077,.T.);
#1856=FACE_OUTER_BOUND('',#3078,.T.);
#1857=FACE_OUTER_BOUND('',#3079,.T.);
#1858=FACE_OUTER_BOUND('',#3080,.T.);
#1859=FACE_OUTER_BOUND('',#3081,.T.);
#1860=FACE_OUTER_BOUND('',#3082,.T.);
#1861=FACE_OUTER_BOUND('',#3083,.T.);
#1862=FACE_OUTER_BOUND('',#3084,.T.);
#1863=FACE_OUTER_BOUND('',#3085,.T.);
#1864=FACE_OUTER_BOUND('',#3086,.T.);
#1865=FACE_OUTER_BOUND('',#3087,.T.);
#1866=FACE_OUTER_BOUND('',#3088,.T.);
#1867=FACE_OUTER_BOUND('',#3089,.T.);
#1868=FACE_OUTER_BOUND('',#3090,.T.);
#1869=FACE_OUTER_BOUND('',#3091,.T.);
#1870=FACE_OUTER_BOUND('',#3092,.T.);
#1871=FACE_OUTER_BOUND('',#3093,.T.);
#1872=FACE_OUTER_BOUND('',#3094,.T.);
#1873=FACE_OUTER_BOUND('',#3095,.T.);
#1874=FACE_OUTER_BOUND('',#3096,.T.);
#1875=FACE_OUTER_BOUND('',#3097,.T.);
#1876=FACE_OUTER_BOUND('',#3098,.T.);
#1877=FACE_OUTER_BOUND('',#3099,.T.);
#1878=FACE_OUTER_BOUND('',#3100,.T.);
#1879=FACE_OUTER_BOUND('',#3101,.T.);
#1880=FACE_OUTER_BOUND('',#3102,.T.);
#1881=FACE_OUTER_BOUND('',#3103,.T.);
#1882=FACE_OUTER_BOUND('',#3104,.T.);
#1883=FACE_OUTER_BOUND('',#3105,.T.);
#1884=FACE_OUTER_BOUND('',#3106,.T.);
#1885=FACE_OUTER_BOUND('',#3107,.T.);
#1886=FACE_OUTER_BOUND('',#3108,.T.);
#1887=FACE_OUTER_BOUND('',#3109,.T.);
#1888=FACE_OUTER_BOUND('',#3110,.T.);
#1889=FACE_OUTER_BOUND('',#3111,.T.);
#1890=FACE_OUTER_BOUND('',#3112,.T.);
#1891=FACE_OUTER_BOUND('',#3113,.T.);
#1892=FACE_OUTER_BOUND('',#3114,.T.);
#1893=FACE_OUTER_BOUND('',#3115,.T.);
#1894=FACE_OUTER_BOUND('',#3116,.T.);
#1895=FACE_OUTER_BOUND('',#3117,.T.);
#1896=FACE_OUTER_BOUND('',#3118,.T.);
#1897=FACE_OUTER_BOUND('',#3119,.T.);
#1898=FACE_OUTER_BOUND('',#3120,.T.);
#1899=FACE_OUTER_BOUND('',#3121,.T.);
#1900=FACE_OUTER_BOUND('',#3122,.T.);
#1901=FACE_OUTER_BOUND('',#3123,.T.);
#1902=FACE_OUTER_BOUND('',#3124,.T.);
#1903=FACE_OUTER_BOUND('',#3125,.T.);
#1904=FACE_OUTER_BOUND('',#3126,.T.);
#1905=FACE_OUTER_BOUND('',#3127,.T.);
#1906=FACE_OUTER_BOUND('',#3128,.T.);
#1907=FACE_OUTER_BOUND('',#3129,.T.);
#1908=FACE_OUTER_BOUND('',#3130,.T.);
#1909=FACE_OUTER_BOUND('',#3131,.T.);
#1910=FACE_OUTER_BOUND('',#3132,.T.);
#1911=FACE_OUTER_BOUND('',#3133,.T.);
#1912=FACE_OUTER_BOUND('',#3134,.T.);
#1913=FACE_OUTER_BOUND('',#3135,.T.);
#1914=FACE_OUTER_BOUND('',#3136,.T.);
#1915=FACE_OUTER_BOUND('',#3137,.T.);
#1916=FACE_OUTER_BOUND('',#3138,.T.);
#1917=FACE_OUTER_BOUND('',#3139,.T.);
#1918=FACE_OUTER_BOUND('',#3140,.T.);
#1919=FACE_OUTER_BOUND('',#3141,.T.);
#1920=FACE_OUTER_BOUND('',#3142,.T.);
#1921=FACE_OUTER_BOUND('',#3143,.T.);
#1922=FACE_OUTER_BOUND('',#3144,.T.);
#1923=FACE_OUTER_BOUND('',#3145,.T.);
#1924=FACE_OUTER_BOUND('',#3146,.T.);
#1925=FACE_OUTER_BOUND('',#3147,.T.);
#1926=FACE_OUTER_BOUND('',#3148,.T.);
#1927=FACE_OUTER_BOUND('',#3149,.T.);
#1928=FACE_OUTER_BOUND('',#3150,.T.);
#1929=FACE_OUTER_BOUND('',#3151,.T.);
#1930=FACE_OUTER_BOUND('',#3152,.T.);
#1931=FACE_OUTER_BOUND('',#3153,.T.);
#1932=FACE_OUTER_BOUND('',#3154,.T.);
#1933=FACE_OUTER_BOUND('',#3155,.T.);
#1934=FACE_OUTER_BOUND('',#3156,.T.);
#1935=FACE_OUTER_BOUND('',#3157,.T.);
#1936=FACE_OUTER_BOUND('',#3158,.T.);
#1937=FACE_OUTER_BOUND('',#3159,.T.);
#1938=FACE_OUTER_BOUND('',#3160,.T.);
#1939=FACE_OUTER_BOUND('',#3161,.T.);
#1940=FACE_OUTER_BOUND('',#3162,.T.);
#1941=FACE_OUTER_BOUND('',#3163,.T.);
#1942=FACE_OUTER_BOUND('',#3164,.T.);
#1943=FACE_OUTER_BOUND('',#3165,.T.);
#1944=FACE_OUTER_BOUND('',#3166,.T.);
#1945=FACE_OUTER_BOUND('',#3167,.T.);
#1946=FACE_OUTER_BOUND('',#3168,.T.);
#1947=FACE_OUTER_BOUND('',#3169,.T.);
#1948=FACE_OUTER_BOUND('',#3170,.T.);
#1949=FACE_OUTER_BOUND('',#3171,.T.);
#1950=FACE_OUTER_BOUND('',#3172,.T.);
#1951=FACE_OUTER_BOUND('',#3173,.T.);
#1952=FACE_OUTER_BOUND('',#3174,.T.);
#1953=FACE_OUTER_BOUND('',#3175,.T.);
#1954=FACE_OUTER_BOUND('',#3176,.T.);
#1955=FACE_OUTER_BOUND('',#3177,.T.);
#1956=FACE_OUTER_BOUND('',#3178,.T.);
#1957=FACE_OUTER_BOUND('',#3179,.T.);
#1958=FACE_OUTER_BOUND('',#3180,.T.);
#1959=FACE_OUTER_BOUND('',#3181,.T.);
#1960=FACE_OUTER_BOUND('',#3182,.T.);
#1961=FACE_OUTER_BOUND('',#3183,.T.);
#1962=FACE_OUTER_BOUND('',#3184,.T.);
#1963=FACE_OUTER_BOUND('',#3185,.T.);
#1964=FACE_OUTER_BOUND('',#3186,.T.);
#1965=FACE_OUTER_BOUND('',#3187,.T.);
#1966=FACE_OUTER_BOUND('',#3188,.T.);
#1967=FACE_OUTER_BOUND('',#3189,.T.);
#1968=FACE_OUTER_BOUND('',#3190,.T.);
#1969=FACE_OUTER_BOUND('',#3191,.T.);
#1970=FACE_OUTER_BOUND('',#3192,.T.);
#1971=FACE_OUTER_BOUND('',#3193,.T.);
#1972=FACE_OUTER_BOUND('',#3194,.T.);
#1973=FACE_OUTER_BOUND('',#3195,.T.);
#1974=FACE_OUTER_BOUND('',#3196,.T.);
#1975=FACE_OUTER_BOUND('',#3197,.T.);
#1976=FACE_OUTER_BOUND('',#3198,.T.);
#1977=FACE_OUTER_BOUND('',#3199,.T.);
#1978=FACE_OUTER_BOUND('',#3200,.T.);
#1979=FACE_OUTER_BOUND('',#3201,.T.);
#1980=FACE_OUTER_BOUND('',#3202,.T.);
#1981=FACE_OUTER_BOUND('',#3203,.T.);
#1982=FACE_OUTER_BOUND('',#3204,.T.);
#1983=FACE_OUTER_BOUND('',#3205,.T.);
#1984=FACE_OUTER_BOUND('',#3206,.T.);
#1985=FACE_OUTER_BOUND('',#3207,.T.);
#1986=FACE_OUTER_BOUND('',#3208,.T.);
#1987=FACE_OUTER_BOUND('',#3209,.T.);
#1988=FACE_OUTER_BOUND('',#3210,.T.);
#1989=FACE_OUTER_BOUND('',#3211,.T.);
#1990=FACE_OUTER_BOUND('',#3212,.T.);
#1991=FACE_OUTER_BOUND('',#3213,.T.);
#1992=FACE_OUTER_BOUND('',#3214,.T.);
#1993=FACE_OUTER_BOUND('',#3215,.T.);
#1994=FACE_OUTER_BOUND('',#3217,.T.);
#1995=FACE_OUTER_BOUND('',#3218,.T.);
#1996=FACE_OUTER_BOUND('',#3219,.T.);
#1997=FACE_OUTER_BOUND('',#3220,.T.);
#1998=FACE_OUTER_BOUND('',#3221,.T.);
#1999=FACE_OUTER_BOUND('',#3222,.T.);
#2000=FACE_OUTER_BOUND('',#3224,.T.);
#2001=FACE_OUTER_BOUND('',#3225,.T.);
#2002=FACE_OUTER_BOUND('',#3226,.T.);
#2003=FACE_OUTER_BOUND('',#3227,.T.);
#2004=FACE_OUTER_BOUND('',#3228,.T.);
#2005=FACE_OUTER_BOUND('',#3229,.T.);
#2006=FACE_OUTER_BOUND('',#3230,.T.);
#2007=FACE_OUTER_BOUND('',#3231,.T.);
#2008=FACE_OUTER_BOUND('',#3232,.T.);
#2009=FACE_OUTER_BOUND('',#3233,.T.);
#2010=FACE_OUTER_BOUND('',#3234,.T.);
#2011=FACE_OUTER_BOUND('',#3235,.T.);
#2012=FACE_OUTER_BOUND('',#3236,.T.);
#2013=FACE_OUTER_BOUND('',#3237,.T.);
#2014=FACE_OUTER_BOUND('',#3238,.T.);
#2015=FACE_OUTER_BOUND('',#3239,.T.);
#2016=FACE_OUTER_BOUND('',#3240,.T.);
#2017=FACE_OUTER_BOUND('',#3241,.T.);
#2018=FACE_OUTER_BOUND('',#3242,.T.);
#2019=FACE_OUTER_BOUND('',#3243,.T.);
#2020=FACE_OUTER_BOUND('',#3244,.T.);
#2021=FACE_OUTER_BOUND('',#3245,.T.);
#2022=FACE_OUTER_BOUND('',#3246,.T.);
#2023=FACE_OUTER_BOUND('',#3247,.T.);
#2024=FACE_OUTER_BOUND('',#3248,.T.);
#2025=FACE_OUTER_BOUND('',#3249,.T.);
#2026=FACE_OUTER_BOUND('',#3250,.T.);
#2027=FACE_OUTER_BOUND('',#3251,.T.);
#2028=FACE_OUTER_BOUND('',#3252,.T.);
#2029=FACE_OUTER_BOUND('',#3253,.T.);
#2030=FACE_OUTER_BOUND('',#3254,.T.);
#2031=FACE_OUTER_BOUND('',#3255,.T.);
#2032=FACE_OUTER_BOUND('',#3256,.T.);
#2033=FACE_OUTER_BOUND('',#3257,.T.);
#2034=FACE_OUTER_BOUND('',#3258,.T.);
#2035=FACE_OUTER_BOUND('',#3259,.T.);
#2036=FACE_OUTER_BOUND('',#3260,.T.);
#2037=FACE_OUTER_BOUND('',#3261,.T.);
#2038=FACE_OUTER_BOUND('',#3262,.T.);
#2039=FACE_OUTER_BOUND('',#3263,.T.);
#2040=FACE_OUTER_BOUND('',#3264,.T.);
#2041=FACE_OUTER_BOUND('',#3265,.T.);
#2042=FACE_OUTER_BOUND('',#3266,.T.);
#2043=FACE_OUTER_BOUND('',#3267,.T.);
#2044=FACE_OUTER_BOUND('',#3268,.T.);
#2045=FACE_OUTER_BOUND('',#3269,.T.);
#2046=FACE_OUTER_BOUND('',#3270,.T.);
#2047=FACE_OUTER_BOUND('',#3271,.T.);
#2048=FACE_OUTER_BOUND('',#3272,.T.);
#2049=FACE_OUTER_BOUND('',#3273,.T.);
#2050=FACE_OUTER_BOUND('',#3274,.T.);
#2051=FACE_OUTER_BOUND('',#3275,.T.);
#2052=FACE_OUTER_BOUND('',#3276,.T.);
#2053=FACE_OUTER_BOUND('',#3277,.T.);
#2054=FACE_OUTER_BOUND('',#3278,.T.);
#2055=FACE_OUTER_BOUND('',#3279,.T.);
#2056=FACE_OUTER_BOUND('',#3280,.T.);
#2057=FACE_OUTER_BOUND('',#3281,.T.);
#2058=FACE_OUTER_BOUND('',#3282,.T.);
#2059=FACE_OUTER_BOUND('',#3283,.T.);
#2060=FACE_OUTER_BOUND('',#3284,.T.);
#2061=FACE_OUTER_BOUND('',#3285,.T.);
#2062=FACE_OUTER_BOUND('',#3286,.T.);
#2063=FACE_OUTER_BOUND('',#3287,.T.);
#2064=FACE_OUTER_BOUND('',#3288,.T.);
#2065=FACE_OUTER_BOUND('',#3289,.T.);
#2066=FACE_OUTER_BOUND('',#3290,.T.);
#2067=FACE_OUTER_BOUND('',#3291,.T.);
#2068=FACE_OUTER_BOUND('',#3292,.T.);
#2069=FACE_OUTER_BOUND('',#3293,.T.);
#2070=FACE_OUTER_BOUND('',#3294,.T.);
#2071=FACE_OUTER_BOUND('',#3295,.T.);
#2072=FACE_OUTER_BOUND('',#3297,.T.);
#2073=FACE_OUTER_BOUND('',#3298,.T.);
#2074=FACE_OUTER_BOUND('',#3299,.T.);
#2075=FACE_OUTER_BOUND('',#3300,.T.);
#2076=FACE_OUTER_BOUND('',#3302,.T.);
#2077=FACE_OUTER_BOUND('',#3303,.T.);
#2078=FACE_OUTER_BOUND('',#3304,.T.);
#2079=FACE_OUTER_BOUND('',#3305,.T.);
#2080=FACE_OUTER_BOUND('',#3306,.T.);
#2081=FACE_OUTER_BOUND('',#3307,.T.);
#2082=FACE_OUTER_BOUND('',#3308,.T.);
#2083=FACE_OUTER_BOUND('',#3309,.T.);
#2084=FACE_OUTER_BOUND('',#3310,.T.);
#2085=FACE_OUTER_BOUND('',#3311,.T.);
#2086=FACE_OUTER_BOUND('',#3312,.T.);
#2087=FACE_OUTER_BOUND('',#3313,.T.);
#2088=FACE_OUTER_BOUND('',#3314,.T.);
#2089=FACE_OUTER_BOUND('',#3315,.T.);
#2090=FACE_OUTER_BOUND('',#3316,.T.);
#2091=FACE_OUTER_BOUND('',#3317,.T.);
#2092=FACE_OUTER_BOUND('',#3318,.T.);
#2093=FACE_OUTER_BOUND('',#3319,.T.);
#2094=FACE_OUTER_BOUND('',#3320,.T.);
#2095=FACE_OUTER_BOUND('',#3321,.T.);
#2096=FACE_OUTER_BOUND('',#3322,.T.);
#2097=FACE_OUTER_BOUND('',#3323,.T.);
#2098=FACE_OUTER_BOUND('',#3324,.T.);
#2099=FACE_OUTER_BOUND('',#3325,.T.);
#2100=FACE_OUTER_BOUND('',#3327,.T.);
#2101=FACE_OUTER_BOUND('',#3328,.T.);
#2102=FACE_OUTER_BOUND('',#3329,.T.);
#2103=FACE_OUTER_BOUND('',#3330,.T.);
#2104=FACE_OUTER_BOUND('',#3331,.T.);
#2105=FACE_OUTER_BOUND('',#3332,.T.);
#2106=FACE_OUTER_BOUND('',#3333,.T.);
#2107=FACE_OUTER_BOUND('',#3334,.T.);
#2108=FACE_OUTER_BOUND('',#3335,.T.);
#2109=FACE_OUTER_BOUND('',#3336,.T.);
#2110=FACE_OUTER_BOUND('',#3337,.T.);
#2111=FACE_OUTER_BOUND('',#3338,.T.);
#2112=FACE_OUTER_BOUND('',#3339,.T.);
#2113=FACE_OUTER_BOUND('',#3340,.T.);
#2114=FACE_OUTER_BOUND('',#3341,.T.);
#2115=FACE_OUTER_BOUND('',#3343,.T.);
#2116=FACE_OUTER_BOUND('',#3344,.T.);
#2117=FACE_OUTER_BOUND('',#3345,.T.);
#2118=FACE_OUTER_BOUND('',#3346,.T.);
#2119=FACE_OUTER_BOUND('',#3347,.T.);
#2120=FACE_OUTER_BOUND('',#3348,.T.);
#2121=FACE_OUTER_BOUND('',#3349,.T.);
#2122=FACE_OUTER_BOUND('',#3350,.T.);
#2123=FACE_OUTER_BOUND('',#3351,.T.);
#2124=FACE_OUTER_BOUND('',#3352,.T.);
#2125=FACE_OUTER_BOUND('',#3353,.T.);
#2126=FACE_OUTER_BOUND('',#3354,.T.);
#2127=FACE_OUTER_BOUND('',#3355,.T.);
#2128=FACE_OUTER_BOUND('',#3356,.T.);
#2129=FACE_OUTER_BOUND('',#3357,.T.);
#2130=FACE_OUTER_BOUND('',#3358,.T.);
#2131=FACE_OUTER_BOUND('',#3359,.T.);
#2132=FACE_OUTER_BOUND('',#3360,.T.);
#2133=FACE_OUTER_BOUND('',#3361,.T.);
#2134=FACE_OUTER_BOUND('',#3362,.T.);
#2135=FACE_OUTER_BOUND('',#3363,.T.);
#2136=FACE_OUTER_BOUND('',#3364,.T.);
#2137=FACE_OUTER_BOUND('',#3365,.T.);
#2138=FACE_OUTER_BOUND('',#3366,.T.);
#2139=FACE_OUTER_BOUND('',#3367,.T.);
#2140=FACE_OUTER_BOUND('',#3368,.T.);
#2141=FACE_OUTER_BOUND('',#3369,.T.);
#2142=FACE_OUTER_BOUND('',#3370,.T.);
#2143=FACE_OUTER_BOUND('',#3371,.T.);
#2144=FACE_OUTER_BOUND('',#3372,.T.);
#2145=FACE_OUTER_BOUND('',#3373,.T.);
#2146=FACE_OUTER_BOUND('',#3374,.T.);
#2147=FACE_OUTER_BOUND('',#3375,.T.);
#2148=FACE_OUTER_BOUND('',#3376,.T.);
#2149=FACE_OUTER_BOUND('',#3377,.T.);
#2150=FACE_OUTER_BOUND('',#3378,.T.);
#2151=FACE_OUTER_BOUND('',#3379,.T.);
#2152=FACE_OUTER_BOUND('',#3380,.T.);
#2153=FACE_OUTER_BOUND('',#3381,.T.);
#2154=FACE_OUTER_BOUND('',#3383,.T.);
#2155=FACE_OUTER_BOUND('',#3384,.T.);
#2156=FACE_OUTER_BOUND('',#3386,.T.);
#2157=FACE_OUTER_BOUND('',#3387,.T.);
#2158=FACE_OUTER_BOUND('',#3388,.T.);
#2159=FACE_OUTER_BOUND('',#3389,.T.);
#2160=FACE_OUTER_BOUND('',#3390,.T.);
#2161=FACE_OUTER_BOUND('',#3391,.T.);
#2162=FACE_OUTER_BOUND('',#3392,.T.);
#2163=FACE_OUTER_BOUND('',#3393,.T.);
#2164=FACE_OUTER_BOUND('',#3394,.T.);
#2165=FACE_OUTER_BOUND('',#3395,.T.);
#2166=FACE_OUTER_BOUND('',#3396,.T.);
#2167=FACE_OUTER_BOUND('',#3397,.T.);
#2168=FACE_OUTER_BOUND('',#3398,.T.);
#2169=FACE_OUTER_BOUND('',#3399,.T.);
#2170=FACE_OUTER_BOUND('',#3400,.T.);
#2171=FACE_OUTER_BOUND('',#3401,.T.);
#2172=FACE_OUTER_BOUND('',#3402,.T.);
#2173=FACE_OUTER_BOUND('',#3403,.T.);
#2174=FACE_OUTER_BOUND('',#3404,.T.);
#2175=FACE_OUTER_BOUND('',#3405,.T.);
#2176=FACE_OUTER_BOUND('',#3406,.T.);
#2177=FACE_OUTER_BOUND('',#3407,.T.);
#2178=FACE_OUTER_BOUND('',#3408,.T.);
#2179=FACE_OUTER_BOUND('',#3409,.T.);
#2180=FACE_OUTER_BOUND('',#3410,.T.);
#2181=FACE_OUTER_BOUND('',#3411,.T.);
#2182=FACE_OUTER_BOUND('',#3412,.T.);
#2183=FACE_OUTER_BOUND('',#3413,.T.);
#2184=FACE_OUTER_BOUND('',#3414,.T.);
#2185=FACE_OUTER_BOUND('',#3415,.T.);
#2186=FACE_OUTER_BOUND('',#3416,.T.);
#2187=FACE_OUTER_BOUND('',#3417,.T.);
#2188=FACE_OUTER_BOUND('',#3418,.T.);
#2189=FACE_OUTER_BOUND('',#3419,.T.);
#2190=FACE_OUTER_BOUND('',#3420,.T.);
#2191=FACE_OUTER_BOUND('',#3421,.T.);
#2192=FACE_OUTER_BOUND('',#3422,.T.);
#2193=FACE_OUTER_BOUND('',#3423,.T.);
#2194=FACE_OUTER_BOUND('',#3424,.T.);
#2195=FACE_OUTER_BOUND('',#3425,.T.);
#2196=FACE_OUTER_BOUND('',#3426,.T.);
#2197=FACE_OUTER_BOUND('',#3427,.T.);
#2198=FACE_OUTER_BOUND('',#3428,.T.);
#2199=FACE_OUTER_BOUND('',#3429,.T.);
#2200=FACE_OUTER_BOUND('',#3430,.T.);
#2201=FACE_OUTER_BOUND('',#3431,.T.);
#2202=FACE_OUTER_BOUND('',#3432,.T.);
#2203=FACE_OUTER_BOUND('',#3433,.T.);
#2204=FACE_OUTER_BOUND('',#3434,.T.);
#2205=FACE_OUTER_BOUND('',#3435,.T.);
#2206=FACE_OUTER_BOUND('',#3436,.T.);
#2207=FACE_OUTER_BOUND('',#3437,.T.);
#2208=FACE_OUTER_BOUND('',#3438,.T.);
#2209=FACE_OUTER_BOUND('',#3439,.T.);
#2210=FACE_OUTER_BOUND('',#3440,.T.);
#2211=FACE_OUTER_BOUND('',#3441,.T.);
#2212=FACE_OUTER_BOUND('',#3442,.T.);
#2213=FACE_OUTER_BOUND('',#3443,.T.);
#2214=FACE_OUTER_BOUND('',#3444,.T.);
#2215=FACE_OUTER_BOUND('',#3445,.T.);
#2216=FACE_OUTER_BOUND('',#3446,.T.);
#2217=FACE_OUTER_BOUND('',#3447,.T.);
#2218=FACE_OUTER_BOUND('',#3448,.T.);
#2219=FACE_OUTER_BOUND('',#3449,.T.);
#2220=FACE_OUTER_BOUND('',#3450,.T.);
#2221=FACE_OUTER_BOUND('',#3451,.T.);
#2222=FACE_OUTER_BOUND('',#3452,.T.);
#2223=FACE_OUTER_BOUND('',#3453,.T.);
#2224=FACE_OUTER_BOUND('',#3454,.T.);
#2225=FACE_OUTER_BOUND('',#3455,.T.);
#2226=FACE_OUTER_BOUND('',#3456,.T.);
#2227=FACE_OUTER_BOUND('',#3457,.T.);
#2228=FACE_OUTER_BOUND('',#3458,.T.);
#2229=FACE_OUTER_BOUND('',#3459,.T.);
#2230=FACE_OUTER_BOUND('',#3460,.T.);
#2231=FACE_OUTER_BOUND('',#3461,.T.);
#2232=FACE_OUTER_BOUND('',#3462,.T.);
#2233=FACE_OUTER_BOUND('',#3463,.T.);
#2234=FACE_OUTER_BOUND('',#3464,.T.);
#2235=FACE_OUTER_BOUND('',#3465,.T.);
#2236=FACE_OUTER_BOUND('',#3466,.T.);
#2237=FACE_OUTER_BOUND('',#3467,.T.);
#2238=FACE_OUTER_BOUND('',#3468,.T.);
#2239=FACE_OUTER_BOUND('',#3469,.T.);
#2240=FACE_OUTER_BOUND('',#3470,.T.);
#2241=FACE_OUTER_BOUND('',#3471,.T.);
#2242=FACE_OUTER_BOUND('',#3472,.T.);
#2243=FACE_OUTER_BOUND('',#3473,.T.);
#2244=FACE_OUTER_BOUND('',#3474,.T.);
#2245=FACE_OUTER_BOUND('',#3475,.T.);
#2246=FACE_OUTER_BOUND('',#3476,.T.);
#2247=FACE_OUTER_BOUND('',#3477,.T.);
#2248=FACE_OUTER_BOUND('',#3478,.T.);
#2249=FACE_OUTER_BOUND('',#3479,.T.);
#2250=FACE_OUTER_BOUND('',#3480,.T.);
#2251=FACE_OUTER_BOUND('',#3481,.T.);
#2252=FACE_OUTER_BOUND('',#3482,.T.);
#2253=FACE_OUTER_BOUND('',#3483,.T.);
#2254=FACE_OUTER_BOUND('',#3484,.T.);
#2255=FACE_OUTER_BOUND('',#3485,.T.);
#2256=FACE_OUTER_BOUND('',#3486,.T.);
#2257=FACE_OUTER_BOUND('',#3487,.T.);
#2258=FACE_OUTER_BOUND('',#3488,.T.);
#2259=FACE_OUTER_BOUND('',#3489,.T.);
#2260=FACE_OUTER_BOUND('',#3490,.T.);
#2261=FACE_OUTER_BOUND('',#3491,.T.);
#2262=FACE_OUTER_BOUND('',#3492,.T.);
#2263=FACE_OUTER_BOUND('',#3493,.T.);
#2264=FACE_OUTER_BOUND('',#3494,.T.);
#2265=FACE_OUTER_BOUND('',#3495,.T.);
#2266=FACE_OUTER_BOUND('',#3496,.T.);
#2267=FACE_OUTER_BOUND('',#3497,.T.);
#2268=FACE_OUTER_BOUND('',#3498,.T.);
#2269=FACE_OUTER_BOUND('',#3499,.T.);
#2270=FACE_OUTER_BOUND('',#3500,.T.);
#2271=FACE_OUTER_BOUND('',#3501,.T.);
#2272=FACE_OUTER_BOUND('',#3502,.T.);
#2273=FACE_OUTER_BOUND('',#3503,.T.);
#2274=FACE_OUTER_BOUND('',#3504,.T.);
#2275=FACE_OUTER_BOUND('',#3505,.T.);
#2276=FACE_OUTER_BOUND('',#3506,.T.);
#2277=FACE_OUTER_BOUND('',#3507,.T.);
#2278=FACE_OUTER_BOUND('',#3508,.T.);
#2279=FACE_OUTER_BOUND('',#3509,.T.);
#2280=FACE_OUTER_BOUND('',#3510,.T.);
#2281=FACE_OUTER_BOUND('',#3511,.T.);
#2282=FACE_OUTER_BOUND('',#3512,.T.);
#2283=FACE_OUTER_BOUND('',#3513,.T.);
#2284=FACE_OUTER_BOUND('',#3514,.T.);
#2285=FACE_OUTER_BOUND('',#3515,.T.);
#2286=FACE_OUTER_BOUND('',#3516,.T.);
#2287=FACE_OUTER_BOUND('',#3517,.T.);
#2288=FACE_OUTER_BOUND('',#3518,.T.);
#2289=FACE_OUTER_BOUND('',#3519,.T.);
#2290=FACE_OUTER_BOUND('',#3520,.T.);
#2291=FACE_OUTER_BOUND('',#3521,.T.);
#2292=FACE_OUTER_BOUND('',#3522,.T.);
#2293=FACE_OUTER_BOUND('',#3523,.T.);
#2294=FACE_OUTER_BOUND('',#3524,.T.);
#2295=FACE_OUTER_BOUND('',#3525,.T.);
#2296=FACE_OUTER_BOUND('',#3526,.T.);
#2297=FACE_OUTER_BOUND('',#3527,.T.);
#2298=FACE_OUTER_BOUND('',#3528,.T.);
#2299=FACE_OUTER_BOUND('',#3529,.T.);
#2300=FACE_OUTER_BOUND('',#3530,.T.);
#2301=FACE_OUTER_BOUND('',#3531,.T.);
#2302=FACE_OUTER_BOUND('',#3532,.T.);
#2303=FACE_OUTER_BOUND('',#3533,.T.);
#2304=FACE_OUTER_BOUND('',#3534,.T.);
#2305=FACE_OUTER_BOUND('',#3535,.T.);
#2306=FACE_OUTER_BOUND('',#3536,.T.);
#2307=FACE_OUTER_BOUND('',#3537,.T.);
#2308=FACE_OUTER_BOUND('',#3538,.T.);
#2309=FACE_OUTER_BOUND('',#3539,.T.);
#2310=FACE_OUTER_BOUND('',#3540,.T.);
#2311=FACE_OUTER_BOUND('',#3541,.T.);
#2312=EDGE_LOOP('',(#12188,#12189,#12190,#12191,#12192,#12193,#12194,#12195,
#12196,#12197,#12198,#12199,#12200,#12201,#12202,#12203));
#2313=EDGE_LOOP('',(#12204,#12205,#12206,#12207));
#2314=EDGE_LOOP('',(#12208,#12209,#12210,#12211));
#2315=EDGE_LOOP('',(#12212,#12213,#12214,#12215));
#2316=EDGE_LOOP('',(#12216,#12217,#12218,#12219));
#2317=EDGE_LOOP('',(#12220,#12221,#12222,#12223));
#2318=EDGE_LOOP('',(#12224,#12225,#12226,#12227));
#2319=EDGE_LOOP('',(#12228,#12229,#12230,#12231));
#2320=EDGE_LOOP('',(#12232,#12233,#12234,#12235));
#2321=EDGE_LOOP('',(#12236,#12237,#12238,#12239));
#2322=EDGE_LOOP('',(#12240,#12241,#12242,#12243));
#2323=EDGE_LOOP('',(#12244,#12245,#12246,#12247));
#2324=EDGE_LOOP('',(#12248,#12249,#12250,#12251));
#2325=EDGE_LOOP('',(#12252,#12253,#12254,#12255));
#2326=EDGE_LOOP('',(#12256,#12257,#12258,#12259));
#2327=EDGE_LOOP('',(#12260,#12261,#12262,#12263));
#2328=EDGE_LOOP('',(#12264,#12265,#12266,#12267));
#2329=EDGE_LOOP('',(#12268,#12269,#12270,#12271));
#2330=EDGE_LOOP('',(#12272,#12273,#12274,#12275));
#2331=EDGE_LOOP('',(#12276,#12277,#12278,#12279));
#2332=EDGE_LOOP('',(#12280,#12281,#12282,#12283));
#2333=EDGE_LOOP('',(#12284,#12285,#12286,#12287));
#2334=EDGE_LOOP('',(#12288,#12289,#12290,#12291));
#2335=EDGE_LOOP('',(#12292,#12293,#12294,#12295));
#2336=EDGE_LOOP('',(#12296,#12297,#12298,#12299));
#2337=EDGE_LOOP('',(#12300,#12301,#12302,#12303));
#2338=EDGE_LOOP('',(#12304,#12305,#12306,#12307));
#2339=EDGE_LOOP('',(#12308,#12309,#12310,#12311));
#2340=EDGE_LOOP('',(#12312,#12313,#12314,#12315));
#2341=EDGE_LOOP('',(#12316,#12317,#12318,#12319));
#2342=EDGE_LOOP('',(#12320,#12321,#12322,#12323));
#2343=EDGE_LOOP('',(#12324,#12325,#12326,#12327));
#2344=EDGE_LOOP('',(#12328,#12329,#12330,#12331));
#2345=EDGE_LOOP('',(#12332,#12333,#12334,#12335));
#2346=EDGE_LOOP('',(#12336,#12337,#12338,#12339));
#2347=EDGE_LOOP('',(#12340,#12341,#12342,#12343));
#2348=EDGE_LOOP('',(#12344,#12345,#12346,#12347));
#2349=EDGE_LOOP('',(#12348,#12349,#12350,#12351));
#2350=EDGE_LOOP('',(#12352,#12353,#12354,#12355));
#2351=EDGE_LOOP('',(#12356,#12357,#12358,#12359));
#2352=EDGE_LOOP('',(#12360,#12361,#12362,#12363));
#2353=EDGE_LOOP('',(#12364,#12365,#12366,#12367));
#2354=EDGE_LOOP('',(#12368,#12369,#12370,#12371));
#2355=EDGE_LOOP('',(#12372,#12373,#12374,#12375));
#2356=EDGE_LOOP('',(#12376,#12377,#12378,#12379));
#2357=EDGE_LOOP('',(#12380,#12381,#12382,#12383));
#2358=EDGE_LOOP('',(#12384,#12385,#12386,#12387));
#2359=EDGE_LOOP('',(#12388,#12389,#12390,#12391));
#2360=EDGE_LOOP('',(#12392,#12393,#12394,#12395));
#2361=EDGE_LOOP('',(#12396,#12397,#12398,#12399));
#2362=EDGE_LOOP('',(#12400,#12401,#12402,#12403));
#2363=EDGE_LOOP('',(#12404,#12405,#12406,#12407));
#2364=EDGE_LOOP('',(#12408,#12409,#12410,#12411));
#2365=EDGE_LOOP('',(#12412,#12413,#12414,#12415));
#2366=EDGE_LOOP('',(#12416,#12417,#12418,#12419));
#2367=EDGE_LOOP('',(#12420,#12421,#12422,#12423));
#2368=EDGE_LOOP('',(#12424,#12425,#12426,#12427));
#2369=EDGE_LOOP('',(#12428,#12429,#12430,#12431));
#2370=EDGE_LOOP('',(#12432,#12433,#12434,#12435));
#2371=EDGE_LOOP('',(#12436,#12437,#12438,#12439));
#2372=EDGE_LOOP('',(#12440,#12441,#12442,#12443));
#2373=EDGE_LOOP('',(#12444,#12445,#12446,#12447));
#2374=EDGE_LOOP('',(#12448,#12449,#12450,#12451));
#2375=EDGE_LOOP('',(#12452,#12453,#12454,#12455,#12456,#12457,#12458,#12459));
#2376=EDGE_LOOP('',(#12460,#12461,#12462,#12463));
#2377=EDGE_LOOP('',(#12464,#12465,#12466,#12467));
#2378=EDGE_LOOP('',(#12468,#12469,#12470,#12471));
#2379=EDGE_LOOP('',(#12472,#12473,#12474,#12475));
#2380=EDGE_LOOP('',(#12476,#12477,#12478,#12479));
#2381=EDGE_LOOP('',(#12480,#12481,#12482,#12483));
#2382=EDGE_LOOP('',(#12484,#12485,#12486,#12487));
#2383=EDGE_LOOP('',(#12488,#12489,#12490,#12491));
#2384=EDGE_LOOP('',(#12492,#12493,#12494,#12495));
#2385=EDGE_LOOP('',(#12496,#12497,#12498,#12499));
#2386=EDGE_LOOP('',(#12500,#12501,#12502,#12503));
#2387=EDGE_LOOP('',(#12504,#12505,#12506,#12507));
#2388=EDGE_LOOP('',(#12508,#12509,#12510,#12511));
#2389=EDGE_LOOP('',(#12512,#12513,#12514,#12515));
#2390=EDGE_LOOP('',(#12516,#12517,#12518,#12519));
#2391=EDGE_LOOP('',(#12520,#12521,#12522,#12523));
#2392=EDGE_LOOP('',(#12524,#12525,#12526,#12527));
#2393=EDGE_LOOP('',(#12528,#12529,#12530,#12531));
#2394=EDGE_LOOP('',(#12532,#12533,#12534,#12535));
#2395=EDGE_LOOP('',(#12536,#12537,#12538,#12539));
#2396=EDGE_LOOP('',(#12540,#12541,#12542,#12543));
#2397=EDGE_LOOP('',(#12544,#12545,#12546,#12547));
#2398=EDGE_LOOP('',(#12548,#12549,#12550,#12551));
#2399=EDGE_LOOP('',(#12552,#12553,#12554,#12555));
#2400=EDGE_LOOP('',(#12556,#12557,#12558,#12559));
#2401=EDGE_LOOP('',(#12560,#12561,#12562,#12563));
#2402=EDGE_LOOP('',(#12564,#12565,#12566,#12567));
#2403=EDGE_LOOP('',(#12568,#12569,#12570,#12571));
#2404=EDGE_LOOP('',(#12572,#12573,#12574,#12575));
#2405=EDGE_LOOP('',(#12576,#12577,#12578,#12579));
#2406=EDGE_LOOP('',(#12580,#12581,#12582,#12583));
#2407=EDGE_LOOP('',(#12584,#12585,#12586));
#2408=EDGE_LOOP('',(#12587,#12588,#12589,#12590,#12591));
#2409=EDGE_LOOP('',(#12592,#12593,#12594,#12595));
#2410=EDGE_LOOP('',(#12596,#12597,#12598,#12599));
#2411=EDGE_LOOP('',(#12600,#12601,#12602,#12603));
#2412=EDGE_LOOP('',(#12604,#12605,#12606,#12607));
#2413=EDGE_LOOP('',(#12608,#12609,#12610,#12611));
#2414=EDGE_LOOP('',(#12612,#12613,#12614,#12615));
#2415=EDGE_LOOP('',(#12616,#12617,#12618,#12619));
#2416=EDGE_LOOP('',(#12620,#12621,#12622,#12623));
#2417=EDGE_LOOP('',(#12624,#12625,#12626,#12627));
#2418=EDGE_LOOP('',(#12628,#12629,#12630,#12631));
#2419=EDGE_LOOP('',(#12632,#12633,#12634,#12635));
#2420=EDGE_LOOP('',(#12636,#12637,#12638,#12639));
#2421=EDGE_LOOP('',(#12640,#12641,#12642,#12643));
#2422=EDGE_LOOP('',(#12644,#12645,#12646,#12647));
#2423=EDGE_LOOP('',(#12648,#12649,#12650,#12651));
#2424=EDGE_LOOP('',(#12652,#12653,#12654,#12655));
#2425=EDGE_LOOP('',(#12656,#12657,#12658,#12659));
#2426=EDGE_LOOP('',(#12660,#12661,#12662,#12663));
#2427=EDGE_LOOP('',(#12664,#12665,#12666,#12667));
#2428=EDGE_LOOP('',(#12668,#12669,#12670,#12671));
#2429=EDGE_LOOP('',(#12672,#12673,#12674,#12675));
#2430=EDGE_LOOP('',(#12676,#12677,#12678,#12679));
#2431=EDGE_LOOP('',(#12680,#12681,#12682,#12683));
#2432=EDGE_LOOP('',(#12684,#12685,#12686,#12687));
#2433=EDGE_LOOP('',(#12688,#12689,#12690,#12691));
#2434=EDGE_LOOP('',(#12692,#12693,#12694,#12695));
#2435=EDGE_LOOP('',(#12696,#12697,#12698,#12699));
#2436=EDGE_LOOP('',(#12700,#12701,#12702,#12703));
#2437=EDGE_LOOP('',(#12704,#12705,#12706,#12707));
#2438=EDGE_LOOP('',(#12708,#12709,#12710,#12711));
#2439=EDGE_LOOP('',(#12712,#12713,#12714,#12715));
#2440=EDGE_LOOP('',(#12716,#12717,#12718,#12719));
#2441=EDGE_LOOP('',(#12720,#12721,#12722,#12723));
#2442=EDGE_LOOP('',(#12724,#12725,#12726,#12727));
#2443=EDGE_LOOP('',(#12728,#12729,#12730,#12731));
#2444=EDGE_LOOP('',(#12732,#12733,#12734,#12735));
#2445=EDGE_LOOP('',(#12736,#12737,#12738,#12739));
#2446=EDGE_LOOP('',(#12740,#12741,#12742,#12743));
#2447=EDGE_LOOP('',(#12744,#12745,#12746,#12747));
#2448=EDGE_LOOP('',(#12748,#12749,#12750,#12751));
#2449=EDGE_LOOP('',(#12752,#12753,#12754,#12755));
#2450=EDGE_LOOP('',(#12756,#12757,#12758,#12759));
#2451=EDGE_LOOP('',(#12760,#12761,#12762,#12763));
#2452=EDGE_LOOP('',(#12764,#12765,#12766,#12767));
#2453=EDGE_LOOP('',(#12768,#12769,#12770,#12771));
#2454=EDGE_LOOP('',(#12772,#12773,#12774,#12775));
#2455=EDGE_LOOP('',(#12776,#12777,#12778,#12779));
#2456=EDGE_LOOP('',(#12780,#12781,#12782,#12783));
#2457=EDGE_LOOP('',(#12784,#12785,#12786,#12787));
#2458=EDGE_LOOP('',(#12788,#12789,#12790,#12791));
#2459=EDGE_LOOP('',(#12792,#12793,#12794,#12795));
#2460=EDGE_LOOP('',(#12796,#12797,#12798,#12799));
#2461=EDGE_LOOP('',(#12800,#12801,#12802,#12803));
#2462=EDGE_LOOP('',(#12804,#12805,#12806,#12807));
#2463=EDGE_LOOP('',(#12808,#12809,#12810,#12811));
#2464=EDGE_LOOP('',(#12812,#12813,#12814,#12815));
#2465=EDGE_LOOP('',(#12816,#12817,#12818,#12819));
#2466=EDGE_LOOP('',(#12820,#12821,#12822,#12823));
#2467=EDGE_LOOP('',(#12824,#12825,#12826,#12827));
#2468=EDGE_LOOP('',(#12828,#12829,#12830,#12831));
#2469=EDGE_LOOP('',(#12832,#12833,#12834,#12835));
#2470=EDGE_LOOP('',(#12836,#12837,#12838,#12839));
#2471=EDGE_LOOP('',(#12840,#12841,#12842,#12843,#12844));
#2472=EDGE_LOOP('',(#12845,#12846,#12847,#12848));
#2473=EDGE_LOOP('',(#12849,#12850,#12851,#12852,#12853));
#2474=EDGE_LOOP('',(#12854,#12855,#12856,#12857,#12858,#12859));
#2475=EDGE_LOOP('',(#12860,#12861,#12862,#12863,#12864,#12865,#12866,#12867,
#12868,#12869,#12870,#12871,#12872,#12873,#12874,#12875,#12876,#12877,#12878,
#12879,#12880,#12881,#12882,#12883,#12884,#12885,#12886,#12887,#12888,#12889,
#12890,#12891,#12892,#12893,#12894,#12895,#12896,#12897,#12898,#12899,#12900,
#12901,#12902,#12903,#12904,#12905,#12906,#12907,#12908,#12909,#12910,#12911,
#12912,#12913,#12914,#12915,#12916,#12917,#12918,#12919,#12920,#12921,#12922,
#12923,#12924,#12925,#12926,#12927,#12928,#12929,#12930,#12931,#12932,#12933,
#12934,#12935,#12936,#12937,#12938,#12939,#12940,#12941,#12942,#12943,#12944,
#12945,#12946,#12947,#12948,#12949,#12950,#12951,#12952,#12953,#12954,#12955,
#12956,#12957,#12958,#12959,#12960,#12961,#12962,#12963,#12964,#12965,#12966,
#12967,#12968,#12969,#12970,#12971,#12972,#12973,#12974,#12975,#12976,#12977,
#12978,#12979,#12980,#12981,#12982,#12983,#12984,#12985,#12986,#12987));
#2476=EDGE_LOOP('',(#12988,#12989,#12990,#12991,#12992));
#2477=EDGE_LOOP('',(#12993,#12994,#12995,#12996));
#2478=EDGE_LOOP('',(#12997,#12998,#12999,#13000,#13001,#13002,#13003,#13004,
#13005,#13006,#13007,#13008,#13009,#13010,#13011,#13012,#13013,#13014,#13015,
#13016,#13017,#13018,#13019,#13020,#13021,#13022,#13023,#13024,#13025,#13026,
#13027,#13028,#13029,#13030,#13031,#13032,#13033,#13034,#13035,#13036,#13037,
#13038,#13039,#13040,#13041,#13042,#13043,#13044,#13045,#13046,#13047,#13048,
#13049,#13050,#13051,#13052,#13053,#13054,#13055,#13056,#13057,#13058,#13059,
#13060,#13061,#13062,#13063,#13064,#13065,#13066,#13067,#13068,#13069,#13070,
#13071,#13072,#13073,#13074,#13075,#13076,#13077,#13078,#13079,#13080,#13081,
#13082,#13083,#13084,#13085,#13086,#13087,#13088,#13089,#13090,#13091,#13092,
#13093,#13094,#13095,#13096,#13097,#13098,#13099,#13100,#13101,#13102,#13103,
#13104,#13105,#13106,#13107,#13108,#13109,#13110,#13111,#13112,#13113,#13114,
#13115,#13116,#13117,#13118,#13119,#13120,#13121,#13122,#13123,#13124,#13125));
#2479=EDGE_LOOP('',(#13126,#13127,#13128,#13129,#13130));
#2480=EDGE_LOOP('',(#13131,#13132,#13133,#13134,#13135,#13136,#13137,#13138,
#13139,#13140,#13141,#13142,#13143,#13144,#13145,#13146,#13147,#13148,#13149,
#13150,#13151,#13152,#13153,#13154,#13155,#13156,#13157,#13158,#13159,#13160,
#13161,#13162,#13163,#13164,#13165,#13166));
#2481=EDGE_LOOP('',(#13167,#13168,#13169,#13170,#13171));
#2482=EDGE_LOOP('',(#13172,#13173,#13174,#13175));
#2483=EDGE_LOOP('',(#13176,#13177,#13178,#13179,#13180,#13181,#13182,#13183,
#13184,#13185,#13186,#13187,#13188,#13189,#13190,#13191,#13192,#13193,#13194,
#13195,#13196,#13197,#13198,#13199,#13200,#13201,#13202,#13203,#13204,#13205,
#13206,#13207,#13208,#13209,#13210,#13211));
#2484=EDGE_LOOP('',(#13212,#13213,#13214,#13215));
#2485=EDGE_LOOP('',(#13216,#13217,#13218,#13219));
#2486=EDGE_LOOP('',(#13220,#13221,#13222,#13223,#13224,#13225));
#2487=EDGE_LOOP('',(#13226,#13227,#13228,#13229));
#2488=EDGE_LOOP('',(#13230,#13231,#13232,#13233,#13234,#13235));
#2489=EDGE_LOOP('',(#13236,#13237,#13238,#13239));
#2490=EDGE_LOOP('',(#13240,#13241,#13242,#13243));
#2491=EDGE_LOOP('',(#13244,#13245,#13246,#13247));
#2492=EDGE_LOOP('',(#13248,#13249,#13250,#13251));
#2493=EDGE_LOOP('',(#13252,#13253,#13254,#13255));
#2494=EDGE_LOOP('',(#13256,#13257,#13258,#13259));
#2495=EDGE_LOOP('',(#13260,#13261,#13262,#13263,#13264,#13265));
#2496=EDGE_LOOP('',(#13266,#13267,#13268,#13269));
#2497=EDGE_LOOP('',(#13270,#13271,#13272,#13273,#13274,#13275));
#2498=EDGE_LOOP('',(#13276,#13277,#13278,#13279));
#2499=EDGE_LOOP('',(#13280,#13281,#13282,#13283));
#2500=EDGE_LOOP('',(#13284,#13285,#13286,#13287));
#2501=EDGE_LOOP('',(#13288,#13289,#13290,#13291));
#2502=EDGE_LOOP('',(#13292,#13293,#13294,#13295));
#2503=EDGE_LOOP('',(#13296,#13297,#13298,#13299,#13300,#13301));
#2504=EDGE_LOOP('',(#13302,#13303,#13304,#13305));
#2505=EDGE_LOOP('',(#13306,#13307,#13308,#13309,#13310,#13311));
#2506=EDGE_LOOP('',(#13312,#13313,#13314,#13315));
#2507=EDGE_LOOP('',(#13316,#13317,#13318,#13319));
#2508=EDGE_LOOP('',(#13320,#13321,#13322,#13323));
#2509=EDGE_LOOP('',(#13324,#13325,#13326,#13327));
#2510=EDGE_LOOP('',(#13328,#13329,#13330,#13331));
#2511=EDGE_LOOP('',(#13332,#13333,#13334,#13335,#13336,#13337));
#2512=EDGE_LOOP('',(#13338,#13339,#13340,#13341));
#2513=EDGE_LOOP('',(#13342,#13343,#13344,#13345,#13346,#13347));
#2514=EDGE_LOOP('',(#13348,#13349,#13350,#13351));
#2515=EDGE_LOOP('',(#13352,#13353,#13354,#13355));
#2516=EDGE_LOOP('',(#13356,#13357,#13358,#13359));
#2517=EDGE_LOOP('',(#13360,#13361,#13362,#13363));
#2518=EDGE_LOOP('',(#13364,#13365,#13366,#13367));
#2519=EDGE_LOOP('',(#13368,#13369,#13370,#13371,#13372,#13373));
#2520=EDGE_LOOP('',(#13374,#13375,#13376,#13377));
#2521=EDGE_LOOP('',(#13378,#13379,#13380,#13381,#13382,#13383));
#2522=EDGE_LOOP('',(#13384,#13385,#13386,#13387));
#2523=EDGE_LOOP('',(#13388,#13389,#13390,#13391));
#2524=EDGE_LOOP('',(#13392,#13393,#13394,#13395));
#2525=EDGE_LOOP('',(#13396,#13397,#13398,#13399));
#2526=EDGE_LOOP('',(#13400,#13401,#13402,#13403));
#2527=EDGE_LOOP('',(#13404,#13405,#13406,#13407,#13408,#13409));
#2528=EDGE_LOOP('',(#13410,#13411,#13412,#13413));
#2529=EDGE_LOOP('',(#13414,#13415,#13416,#13417,#13418,#13419));
#2530=EDGE_LOOP('',(#13420,#13421,#13422,#13423));
#2531=EDGE_LOOP('',(#13424,#13425,#13426,#13427));
#2532=EDGE_LOOP('',(#13428,#13429,#13430,#13431));
#2533=EDGE_LOOP('',(#13432,#13433,#13434,#13435));
#2534=EDGE_LOOP('',(#13436,#13437,#13438,#13439));
#2535=EDGE_LOOP('',(#13440,#13441,#13442,#13443,#13444,#13445));
#2536=EDGE_LOOP('',(#13446,#13447,#13448,#13449));
#2537=EDGE_LOOP('',(#13450,#13451,#13452,#13453,#13454,#13455));
#2538=EDGE_LOOP('',(#13456,#13457,#13458,#13459));
#2539=EDGE_LOOP('',(#13460,#13461,#13462,#13463));
#2540=EDGE_LOOP('',(#13464,#13465,#13466,#13467));
#2541=EDGE_LOOP('',(#13468,#13469,#13470,#13471));
#2542=EDGE_LOOP('',(#13472,#13473,#13474,#13475,#13476));
#2543=EDGE_LOOP('',(#13477,#13478,#13479,#13480,#13481,#13482));
#2544=EDGE_LOOP('',(#13483,#13484,#13485,#13486));
#2545=EDGE_LOOP('',(#13487,#13488,#13489,#13490,#13491,#13492));
#2546=EDGE_LOOP('',(#13493,#13494,#13495,#13496,#13497));
#2547=EDGE_LOOP('',(#13498,#13499,#13500,#13501));
#2548=EDGE_LOOP('',(#13502,#13503,#13504,#13505));
#2549=EDGE_LOOP('',(#13506,#13507,#13508,#13509));
#2550=EDGE_LOOP('',(#13510,#13511,#13512,#13513));
#2551=EDGE_LOOP('',(#13514,#13515,#13516,#13517,#13518,#13519));
#2552=EDGE_LOOP('',(#13520,#13521,#13522,#13523));
#2553=EDGE_LOOP('',(#13524,#13525,#13526,#13527,#13528,#13529));
#2554=EDGE_LOOP('',(#13530,#13531,#13532,#13533));
#2555=EDGE_LOOP('',(#13534,#13535,#13536,#13537));
#2556=EDGE_LOOP('',(#13538,#13539,#13540,#13541));
#2557=EDGE_LOOP('',(#13542,#13543,#13544,#13545));
#2558=EDGE_LOOP('',(#13546,#13547,#13548,#13549));
#2559=EDGE_LOOP('',(#13550,#13551,#13552,#13553,#13554,#13555));
#2560=EDGE_LOOP('',(#13556,#13557,#13558,#13559));
#2561=EDGE_LOOP('',(#13560,#13561,#13562,#13563,#13564,#13565));
#2562=EDGE_LOOP('',(#13566,#13567,#13568,#13569));
#2563=EDGE_LOOP('',(#13570,#13571,#13572,#13573));
#2564=EDGE_LOOP('',(#13574,#13575,#13576,#13577));
#2565=EDGE_LOOP('',(#13578,#13579,#13580,#13581));
#2566=EDGE_LOOP('',(#13582,#13583,#13584,#13585));
#2567=EDGE_LOOP('',(#13586,#13587,#13588,#13589,#13590,#13591));
#2568=EDGE_LOOP('',(#13592,#13593,#13594,#13595));
#2569=EDGE_LOOP('',(#13596,#13597,#13598,#13599,#13600,#13601));
#2570=EDGE_LOOP('',(#13602,#13603,#13604,#13605));
#2571=EDGE_LOOP('',(#13606,#13607,#13608,#13609));
#2572=EDGE_LOOP('',(#13610,#13611,#13612,#13613));
#2573=EDGE_LOOP('',(#13614,#13615,#13616,#13617));
#2574=EDGE_LOOP('',(#13618,#13619,#13620,#13621));
#2575=EDGE_LOOP('',(#13622,#13623,#13624,#13625,#13626,#13627));
#2576=EDGE_LOOP('',(#13628,#13629,#13630,#13631));
#2577=EDGE_LOOP('',(#13632,#13633,#13634,#13635,#13636,#13637));
#2578=EDGE_LOOP('',(#13638,#13639,#13640,#13641));
#2579=EDGE_LOOP('',(#13642,#13643,#13644,#13645));
#2580=EDGE_LOOP('',(#13646,#13647,#13648,#13649));
#2581=EDGE_LOOP('',(#13650,#13651,#13652,#13653));
#2582=EDGE_LOOP('',(#13654,#13655,#13656,#13657));
#2583=EDGE_LOOP('',(#13658,#13659,#13660,#13661,#13662,#13663));
#2584=EDGE_LOOP('',(#13664,#13665,#13666,#13667));
#2585=EDGE_LOOP('',(#13668,#13669,#13670,#13671,#13672,#13673));
#2586=EDGE_LOOP('',(#13674,#13675,#13676,#13677));
#2587=EDGE_LOOP('',(#13678,#13679,#13680,#13681));
#2588=EDGE_LOOP('',(#13682,#13683,#13684,#13685));
#2589=EDGE_LOOP('',(#13686,#13687,#13688,#13689));
#2590=EDGE_LOOP('',(#13690,#13691,#13692,#13693));
#2591=EDGE_LOOP('',(#13694,#13695,#13696,#13697,#13698,#13699));
#2592=EDGE_LOOP('',(#13700,#13701,#13702,#13703));
#2593=EDGE_LOOP('',(#13704,#13705,#13706,#13707,#13708,#13709));
#2594=EDGE_LOOP('',(#13710,#13711,#13712,#13713));
#2595=EDGE_LOOP('',(#13714,#13715,#13716,#13717));
#2596=EDGE_LOOP('',(#13718,#13719,#13720,#13721));
#2597=EDGE_LOOP('',(#13722,#13723,#13724,#13725));
#2598=EDGE_LOOP('',(#13726,#13727,#13728,#13729,#13730,#13731));
#2599=EDGE_LOOP('',(#13732,#13733,#13734,#13735));
#2600=EDGE_LOOP('',(#13736,#13737,#13738,#13739));
#2601=EDGE_LOOP('',(#13740,#13741,#13742,#13743,#13744,#13745));
#2602=EDGE_LOOP('',(#13746,#13747,#13748,#13749));
#2603=EDGE_LOOP('',(#13750,#13751,#13752,#13753));
#2604=EDGE_LOOP('',(#13754,#13755,#13756,#13757));
#2605=EDGE_LOOP('',(#13758));
#2606=EDGE_LOOP('',(#13759,#13760,#13761,#13762));
#2607=EDGE_LOOP('',(#13763,#13764,#13765,#13766,#13767,#13768,#13769,#13770,
#13771,#13772,#13773,#13774,#13775,#13776,#13777,#13778,#13779,#13780,#13781,
#13782,#13783,#13784,#13785,#13786,#13787,#13788,#13789,#13790,#13791,#13792,
#13793,#13794,#13795,#13796,#13797,#13798));
#2608=EDGE_LOOP('',(#13799,#13800,#13801,#13802,#13803,#13804,#13805,#13806,
#13807,#13808,#13809,#13810,#13811,#13812,#13813,#13814,#13815,#13816,#13817,
#13818,#13819,#13820,#13821,#13822,#13823,#13824,#13825,#13826,#13827,#13828,
#13829,#13830,#13831,#13832));
#2609=EDGE_LOOP('',(#13833,#13834,#13835,#13836));
#2610=EDGE_LOOP('',(#13837,#13838,#13839,#13840,#13841,#13842));
#2611=EDGE_LOOP('',(#13843));
#2612=EDGE_LOOP('',(#13844,#13845,#13846,#13847));
#2613=EDGE_LOOP('',(#13848,#13849,#13850,#13851));
#2614=EDGE_LOOP('',(#13852,#13853,#13854,#13855));
#2615=EDGE_LOOP('',(#13856,#13857,#13858,#13859));
#2616=EDGE_LOOP('',(#13860,#13861,#13862));
#2617=EDGE_LOOP('',(#13863,#13864,#13865,#13866));
#2618=EDGE_LOOP('',(#13867,#13868,#13869,#13870));
#2619=EDGE_LOOP('',(#13871,#13872,#13873,#13874));
#2620=EDGE_LOOP('',(#13875,#13876,#13877));
#2621=EDGE_LOOP('',(#13878,#13879,#13880,#13881));
#2622=EDGE_LOOP('',(#13882,#13883,#13884,#13885));
#2623=EDGE_LOOP('',(#13886,#13887,#13888,#13889));
#2624=EDGE_LOOP('',(#13890,#13891,#13892,#13893));
#2625=EDGE_LOOP('',(#13894,#13895,#13896,#13897));
#2626=EDGE_LOOP('',(#13898,#13899,#13900,#13901));
#2627=EDGE_LOOP('',(#13902,#13903,#13904,#13905));
#2628=EDGE_LOOP('',(#13906,#13907,#13908,#13909));
#2629=EDGE_LOOP('',(#13910,#13911,#13912));
#2630=EDGE_LOOP('',(#13913,#13914,#13915,#13916));
#2631=EDGE_LOOP('',(#13917,#13918,#13919,#13920));
#2632=EDGE_LOOP('',(#13921,#13922,#13923,#13924));
#2633=EDGE_LOOP('',(#13925,#13926,#13927,#13928,#13929,#13930));
#2634=EDGE_LOOP('',(#13931,#13932,#13933,#13934));
#2635=EDGE_LOOP('',(#13935,#13936,#13937,#13938,#13939,#13940));
#2636=EDGE_LOOP('',(#13941,#13942,#13943,#13944));
#2637=EDGE_LOOP('',(#13945,#13946,#13947,#13948));
#2638=EDGE_LOOP('',(#13949,#13950,#13951,#13952));
#2639=EDGE_LOOP('',(#13953,#13954,#13955,#13956,#13957,#13958));
#2640=EDGE_LOOP('',(#13959,#13960,#13961,#13962));
#2641=EDGE_LOOP('',(#13963,#13964,#13965,#13966));
#2642=EDGE_LOOP('',(#13967,#13968,#13969,#13970,#13971));
#2643=EDGE_LOOP('',(#13972,#13973,#13974,#13975));
#2644=EDGE_LOOP('',(#13976,#13977,#13978,#13979));
#2645=EDGE_LOOP('',(#13980,#13981,#13982,#13983,#13984));
#2646=EDGE_LOOP('',(#13985,#13986,#13987));
#2647=EDGE_LOOP('',(#13988,#13989,#13990,#13991));
#2648=EDGE_LOOP('',(#13992,#13993,#13994,#13995));
#2649=EDGE_LOOP('',(#13996,#13997,#13998,#13999));
#2650=EDGE_LOOP('',(#14000,#14001,#14002));
#2651=EDGE_LOOP('',(#14003,#14004,#14005,#14006));
#2652=EDGE_LOOP('',(#14007,#14008,#14009,#14010,#14011,#14012));
#2653=EDGE_LOOP('',(#14013,#14014,#14015,#14016,#14017,#14018));
#2654=EDGE_LOOP('',(#14019,#14020,#14021,#14022,#14023));
#2655=EDGE_LOOP('',(#14024,#14025,#14026));
#2656=EDGE_LOOP('',(#14027,#14028,#14029,#14030));
#2657=EDGE_LOOP('',(#14031,#14032,#14033,#14034,#14035,#14036));
#2658=EDGE_LOOP('',(#14037,#14038,#14039,#14040));
#2659=EDGE_LOOP('',(#14041,#14042,#14043,#14044));
#2660=EDGE_LOOP('',(#14045,#14046,#14047,#14048));
#2661=EDGE_LOOP('',(#14049,#14050,#14051,#14052,#14053));
#2662=EDGE_LOOP('',(#14054,#14055,#14056,#14057));
#2663=EDGE_LOOP('',(#14058,#14059,#14060,#14061));
#2664=EDGE_LOOP('',(#14062,#14063,#14064,#14065));
#2665=EDGE_LOOP('',(#14066,#14067,#14068,#14069));
#2666=EDGE_LOOP('',(#14070,#14071,#14072,#14073));
#2667=EDGE_LOOP('',(#14074,#14075,#14076,#14077));
#2668=EDGE_LOOP('',(#14078,#14079,#14080,#14081));
#2669=EDGE_LOOP('',(#14082,#14083,#14084,#14085));
#2670=EDGE_LOOP('',(#14086,#14087,#14088,#14089));
#2671=EDGE_LOOP('',(#14090,#14091,#14092));
#2672=EDGE_LOOP('',(#14093,#14094,#14095,#14096));
#2673=EDGE_LOOP('',(#14097,#14098,#14099));
#2674=EDGE_LOOP('',(#14100,#14101,#14102,#14103));
#2675=EDGE_LOOP('',(#14104,#14105,#14106,#14107));
#2676=EDGE_LOOP('',(#14108,#14109,#14110,#14111));
#2677=EDGE_LOOP('',(#14112,#14113,#14114,#14115));
#2678=EDGE_LOOP('',(#14116,#14117,#14118,#14119));
#2679=EDGE_LOOP('',(#14120,#14121,#14122,#14123));
#2680=EDGE_LOOP('',(#14124,#14125,#14126,#14127));
#2681=EDGE_LOOP('',(#14128,#14129,#14130,#14131));
#2682=EDGE_LOOP('',(#14132,#14133,#14134,#14135,#14136));
#2683=EDGE_LOOP('',(#14137,#14138,#14139));
#2684=EDGE_LOOP('',(#14140,#14141,#14142,#14143));
#2685=EDGE_LOOP('',(#14144,#14145,#14146,#14147));
#2686=EDGE_LOOP('',(#14148,#14149,#14150,#14151,#14152,#14153));
#2687=EDGE_LOOP('',(#14154,#14155,#14156));
#2688=EDGE_LOOP('',(#14157,#14158,#14159,#14160,#14161,#14162));
#2689=EDGE_LOOP('',(#14163,#14164,#14165,#14166,#14167));
#2690=EDGE_LOOP('',(#14168,#14169,#14170,#14171));
#2691=EDGE_LOOP('',(#14172,#14173,#14174,#14175));
#2692=EDGE_LOOP('',(#14176,#14177,#14178,#14179));
#2693=EDGE_LOOP('',(#14180,#14181,#14182));
#2694=EDGE_LOOP('',(#14183,#14184,#14185,#14186));
#2695=EDGE_LOOP('',(#14187,#14188,#14189));
#2696=EDGE_LOOP('',(#14190,#14191,#14192,#14193));
#2697=EDGE_LOOP('',(#14194,#14195,#14196,#14197));
#2698=EDGE_LOOP('',(#14198,#14199,#14200,#14201));
#2699=EDGE_LOOP('',(#14202,#14203,#14204,#14205));
#2700=EDGE_LOOP('',(#14206,#14207,#14208,#14209));
#2701=EDGE_LOOP('',(#14210,#14211,#14212,#14213));
#2702=EDGE_LOOP('',(#14214,#14215,#14216,#14217,#14218,#14219));
#2703=EDGE_LOOP('',(#14220,#14221,#14222,#14223));
#2704=EDGE_LOOP('',(#14224,#14225,#14226,#14227));
#2705=EDGE_LOOP('',(#14228,#14229,#14230,#14231,#14232));
#2706=EDGE_LOOP('',(#14233,#14234,#14235,#14236,#14237));
#2707=EDGE_LOOP('',(#14238,#14239,#14240));
#2708=EDGE_LOOP('',(#14241,#14242,#14243,#14244));
#2709=EDGE_LOOP('',(#14245,#14246,#14247,#14248,#14249));
#2710=EDGE_LOOP('',(#14250,#14251,#14252,#14253));
#2711=EDGE_LOOP('',(#14254,#14255,#14256,#14257,#14258));
#2712=EDGE_LOOP('',(#14259,#14260,#14261,#14262,#14263,#14264));
#2713=EDGE_LOOP('',(#14265,#14266,#14267,#14268));
#2714=EDGE_LOOP('',(#14269,#14270,#14271,#14272));
#2715=EDGE_LOOP('',(#14273,#14274,#14275,#14276));
#2716=EDGE_LOOP('',(#14277,#14278,#14279,#14280));
#2717=EDGE_LOOP('',(#14281,#14282,#14283,#14284));
#2718=EDGE_LOOP('',(#14285,#14286,#14287,#14288));
#2719=EDGE_LOOP('',(#14289,#14290,#14291,#14292));
#2720=EDGE_LOOP('',(#14293,#14294,#14295,#14296));
#2721=EDGE_LOOP('',(#14297,#14298,#14299,#14300));
#2722=EDGE_LOOP('',(#14301,#14302,#14303));
#2723=EDGE_LOOP('',(#14304,#14305,#14306));
#2724=EDGE_LOOP('',(#14307,#14308,#14309,#14310,#14311));
#2725=EDGE_LOOP('',(#14312,#14313,#14314,#14315));
#2726=EDGE_LOOP('',(#14316,#14317,#14318,#14319));
#2727=EDGE_LOOP('',(#14320,#14321,#14322,#14323));
#2728=EDGE_LOOP('',(#14324,#14325,#14326,#14327));
#2729=EDGE_LOOP('',(#14328,#14329,#14330));
#2730=EDGE_LOOP('',(#14331,#14332,#14333,#14334,#14335));
#2731=EDGE_LOOP('',(#14336,#14337,#14338,#14339));
#2732=EDGE_LOOP('',(#14340,#14341,#14342,#14343));
#2733=EDGE_LOOP('',(#14344,#14345,#14346,#14347));
#2734=EDGE_LOOP('',(#14348,#14349,#14350,#14351,#14352));
#2735=EDGE_LOOP('',(#14353,#14354,#14355));
#2736=EDGE_LOOP('',(#14356,#14357,#14358,#14359));
#2737=EDGE_LOOP('',(#14360,#14361,#14362,#14363,#14364,#14365));
#2738=EDGE_LOOP('',(#14366,#14367,#14368,#14369,#14370,#14371));
#2739=EDGE_LOOP('',(#14372,#14373,#14374,#14375,#14376));
#2740=EDGE_LOOP('',(#14377,#14378,#14379,#14380));
#2741=EDGE_LOOP('',(#14381,#14382,#14383,#14384,#14385,#14386));
#2742=EDGE_LOOP('',(#14387,#14388,#14389,#14390,#14391,#14392));
#2743=EDGE_LOOP('',(#14393,#14394,#14395));
#2744=EDGE_LOOP('',(#14396,#14397,#14398,#14399,#14400,#14401));
#2745=EDGE_LOOP('',(#14402,#14403,#14404));
#2746=EDGE_LOOP('',(#14405,#14406,#14407,#14408,#14409));
#2747=EDGE_LOOP('',(#14410,#14411,#14412,#14413));
#2748=EDGE_LOOP('',(#14414,#14415,#14416,#14417));
#2749=EDGE_LOOP('',(#14418,#14419,#14420,#14421));
#2750=EDGE_LOOP('',(#14422,#14423,#14424,#14425,#14426,#14427));
#2751=EDGE_LOOP('',(#14428,#14429,#14430,#14431));
#2752=EDGE_LOOP('',(#14432,#14433,#14434));
#2753=EDGE_LOOP('',(#14435,#14436,#14437,#14438));
#2754=EDGE_LOOP('',(#14439,#14440,#14441,#14442,#14443));
#2755=EDGE_LOOP('',(#14444,#14445,#14446,#14447,#14448,#14449,#14450,#14451,
#14452,#14453,#14454,#14455,#14456,#14457,#14458,#14459,#14460,#14461,#14462,
#14463,#14464));
#2756=EDGE_LOOP('',(#14465));
#2757=EDGE_LOOP('',(#14466));
#2758=EDGE_LOOP('',(#14467,#14468,#14469,#14470,#14471));
#2759=EDGE_LOOP('',(#14472,#14473,#14474,#14475));
#2760=EDGE_LOOP('',(#14476,#14477,#14478,#14479));
#2761=EDGE_LOOP('',(#14480,#14481,#14482));
#2762=EDGE_LOOP('',(#14483,#14484,#14485,#14486,#14487,#14488));
#2763=EDGE_LOOP('',(#14489,#14490,#14491,#14492));
#2764=EDGE_LOOP('',(#14493,#14494,#14495,#14496,#14497,#14498,#14499,#14500,
#14501,#14502,#14503,#14504,#14505,#14506,#14507,#14508));
#2765=EDGE_LOOP('',(#14509));
#2766=EDGE_LOOP('',(#14510,#14511,#14512,#14513));
#2767=EDGE_LOOP('',(#14514,#14515,#14516,#14517));
#2768=EDGE_LOOP('',(#14518,#14519,#14520,#14521));
#2769=EDGE_LOOP('',(#14522,#14523,#14524,#14525,#14526,#14527));
#2770=EDGE_LOOP('',(#14528,#14529,#14530,#14531,#14532));
#2771=EDGE_LOOP('',(#14533,#14534,#14535,#14536));
#2772=EDGE_LOOP('',(#14537,#14538,#14539,#14540,#14541));
#2773=EDGE_LOOP('',(#14542,#14543,#14544,#14545));
#2774=EDGE_LOOP('',(#14546,#14547,#14548,#14549,#14550));
#2775=EDGE_LOOP('',(#14551,#14552,#14553,#14554,#14555,#14556,#14557));
#2776=EDGE_LOOP('',(#14558,#14559,#14560,#14561,#14562));
#2777=EDGE_LOOP('',(#14563,#14564,#14565,#14566,#14567,#14568,#14569,#14570));
#2778=EDGE_LOOP('',(#14571,#14572,#14573,#14574));
#2779=EDGE_LOOP('',(#14575,#14576,#14577));
#2780=EDGE_LOOP('',(#14578,#14579,#14580,#14581,#14582,#14583));
#2781=EDGE_LOOP('',(#14584,#14585,#14586,#14587,#14588,#14589));
#2782=EDGE_LOOP('',(#14590,#14591,#14592,#14593,#14594,#14595,#14596));
#2783=EDGE_LOOP('',(#14597,#14598,#14599,#14600,#14601));
#2784=EDGE_LOOP('',(#14602,#14603,#14604,#14605,#14606,#14607));
#2785=EDGE_LOOP('',(#14608,#14609,#14610,#14611));
#2786=EDGE_LOOP('',(#14612,#14613,#14614,#14615));
#2787=EDGE_LOOP('',(#14616,#14617,#14618,#14619,#14620));
#2788=EDGE_LOOP('',(#14621,#14622,#14623,#14624));
#2789=EDGE_LOOP('',(#14625,#14626,#14627,#14628,#14629));
#2790=EDGE_LOOP('',(#14630,#14631,#14632,#14633));
#2791=EDGE_LOOP('',(#14634,#14635,#14636));
#2792=EDGE_LOOP('',(#14637,#14638,#14639));
#2793=EDGE_LOOP('',(#14640,#14641,#14642,#14643));
#2794=EDGE_LOOP('',(#14644,#14645,#14646,#14647,#14648,#14649));
#2795=EDGE_LOOP('',(#14650,#14651,#14652,#14653));
#2796=EDGE_LOOP('',(#14654,#14655,#14656,#14657));
#2797=EDGE_LOOP('',(#14658,#14659,#14660,#14661));
#2798=EDGE_LOOP('',(#14662,#14663,#14664));
#2799=EDGE_LOOP('',(#14665,#14666,#14667));
#2800=EDGE_LOOP('',(#14668,#14669,#14670,#14671));
#2801=EDGE_LOOP('',(#14672,#14673,#14674,#14675));
#2802=EDGE_LOOP('',(#14676,#14677,#14678,#14679,#14680));
#2803=EDGE_LOOP('',(#14681,#14682,#14683,#14684,#14685));
#2804=EDGE_LOOP('',(#14686));
#2805=EDGE_LOOP('',(#14687,#14688,#14689));
#2806=EDGE_LOOP('',(#14690,#14691,#14692,#14693));
#2807=EDGE_LOOP('',(#14694,#14695,#14696,#14697,#14698));
#2808=EDGE_LOOP('',(#14699,#14700,#14701,#14702));
#2809=EDGE_LOOP('',(#14703,#14704,#14705,#14706));
#2810=EDGE_LOOP('',(#14707,#14708,#14709,#14710));
#2811=EDGE_LOOP('',(#14711,#14712,#14713,#14714));
#2812=EDGE_LOOP('',(#14715,#14716,#14717));
#2813=EDGE_LOOP('',(#14718,#14719,#14720,#14721,#14722,#14723));
#2814=EDGE_LOOP('',(#14724,#14725,#14726,#14727,#14728));
#2815=EDGE_LOOP('',(#14729,#14730,#14731,#14732));
#2816=EDGE_LOOP('',(#14733,#14734,#14735,#14736));
#2817=EDGE_LOOP('',(#14737,#14738,#14739,#14740));
#2818=EDGE_LOOP('',(#14741,#14742,#14743,#14744));
#2819=EDGE_LOOP('',(#14745,#14746,#14747,#14748,#14749));
#2820=EDGE_LOOP('',(#14750,#14751,#14752));
#2821=EDGE_LOOP('',(#14753,#14754,#14755,#14756));
#2822=EDGE_LOOP('',(#14757,#14758,#14759,#14760,#14761,#14762));
#2823=EDGE_LOOP('',(#14763,#14764,#14765,#14766));
#2824=EDGE_LOOP('',(#14767,#14768,#14769,#14770,#14771,#14772));
#2825=EDGE_LOOP('',(#14773,#14774,#14775,#14776,#14777));
#2826=EDGE_LOOP('',(#14778,#14779,#14780,#14781));
#2827=EDGE_LOOP('',(#14782,#14783,#14784,#14785,#14786));
#2828=EDGE_LOOP('',(#14787,#14788,#14789,#14790));
#2829=EDGE_LOOP('',(#14791,#14792,#14793,#14794));
#2830=EDGE_LOOP('',(#14795,#14796,#14797,#14798));
#2831=EDGE_LOOP('',(#14799,#14800,#14801,#14802,#14803,#14804));
#2832=EDGE_LOOP('',(#14805,#14806,#14807,#14808,#14809));
#2833=EDGE_LOOP('',(#14810,#14811,#14812,#14813,#14814));
#2834=EDGE_LOOP('',(#14815));
#2835=EDGE_LOOP('',(#14816,#14817,#14818,#14819));
#2836=EDGE_LOOP('',(#14820,#14821,#14822,#14823,#14824));
#2837=EDGE_LOOP('',(#14825,#14826,#14827,#14828));
#2838=EDGE_LOOP('',(#14829,#14830,#14831,#14832));
#2839=EDGE_LOOP('',(#14833,#14834,#14835,#14836));
#2840=EDGE_LOOP('',(#14837,#14838,#14839,#14840));
#2841=EDGE_LOOP('',(#14841,#14842,#14843,#14844));
#2842=EDGE_LOOP('',(#14845,#14846,#14847,#14848));
#2843=EDGE_LOOP('',(#14849,#14850,#14851,#14852));
#2844=EDGE_LOOP('',(#14853,#14854,#14855,#14856));
#2845=EDGE_LOOP('',(#14857,#14858,#14859,#14860,#14861));
#2846=EDGE_LOOP('',(#14862,#14863,#14864,#14865));
#2847=EDGE_LOOP('',(#14866,#14867,#14868));
#2848=EDGE_LOOP('',(#14869,#14870,#14871,#14872));
#2849=EDGE_LOOP('',(#14873,#14874,#14875,#14876,#14877));
#2850=EDGE_LOOP('',(#14878,#14879,#14880,#14881));
#2851=EDGE_LOOP('',(#14882,#14883,#14884,#14885,#14886));
#2852=EDGE_LOOP('',(#14887,#14888,#14889,#14890,#14891,#14892));
#2853=EDGE_LOOP('',(#14893));
#2854=EDGE_LOOP('',(#14894));
#2855=EDGE_LOOP('',(#14895,#14896,#14897,#14898,#14899,#14900));
#2856=EDGE_LOOP('',(#14901,#14902,#14903,#14904,#14905,#14906));
#2857=EDGE_LOOP('',(#14907,#14908,#14909,#14910,#14911));
#2858=EDGE_LOOP('',(#14912,#14913,#14914,#14915,#14916));
#2859=EDGE_LOOP('',(#14917));
#2860=EDGE_LOOP('',(#14918,#14919,#14920,#14921,#14922));
#2861=EDGE_LOOP('',(#14923,#14924,#14925,#14926,#14927));
#2862=EDGE_LOOP('',(#14928));
#2863=EDGE_LOOP('',(#14929,#14930,#14931,#14932,#14933,#14934));
#2864=EDGE_LOOP('',(#14935,#14936,#14937,#14938));
#2865=EDGE_LOOP('',(#14939,#14940,#14941,#14942));
#2866=EDGE_LOOP('',(#14943,#14944,#14945,#14946));
#2867=EDGE_LOOP('',(#14947,#14948,#14949));
#2868=EDGE_LOOP('',(#14950,#14951,#14952,#14953,#14954,#14955));
#2869=EDGE_LOOP('',(#14956,#14957,#14958,#14959));
#2870=EDGE_LOOP('',(#14960,#14961,#14962,#14963));
#2871=EDGE_LOOP('',(#14964,#14965,#14966,#14967,#14968));
#2872=EDGE_LOOP('',(#14969,#14970,#14971,#14972));
#2873=EDGE_LOOP('',(#14973,#14974,#14975,#14976,#14977));
#2874=EDGE_LOOP('',(#14978,#14979,#14980,#14981,#14982));
#2875=EDGE_LOOP('',(#14983));
#2876=EDGE_LOOP('',(#14984));
#2877=EDGE_LOOP('',(#14985));
#2878=EDGE_LOOP('',(#14986));
#2879=EDGE_LOOP('',(#14987));
#2880=EDGE_LOOP('',(#14988));
#2881=EDGE_LOOP('',(#14989));
#2882=EDGE_LOOP('',(#14990));
#2883=EDGE_LOOP('',(#14991));
#2884=EDGE_LOOP('',(#14992));
#2885=EDGE_LOOP('',(#14993));
#2886=EDGE_LOOP('',(#14994));
#2887=EDGE_LOOP('',(#14995,#14996,#14997,#14998,#14999));
#2888=EDGE_LOOP('',(#15000,#15001,#15002,#15003,#15004));
#2889=EDGE_LOOP('',(#15005,#15006,#15007,#15008,#15009));
#2890=EDGE_LOOP('',(#15010,#15011,#15012,#15013,#15014));
#2891=EDGE_LOOP('',(#15015,#15016,#15017,#15018,#15019));
#2892=EDGE_LOOP('',(#15020,#15021,#15022,#15023,#15024));
#2893=EDGE_LOOP('',(#15025,#15026,#15027,#15028,#15029));
#2894=EDGE_LOOP('',(#15030,#15031,#15032,#15033,#15034));
#2895=EDGE_LOOP('',(#15035,#15036,#15037,#15038,#15039));
#2896=EDGE_LOOP('',(#15040,#15041,#15042,#15043,#15044));
#2897=EDGE_LOOP('',(#15045,#15046,#15047,#15048));
#2898=EDGE_LOOP('',(#15049,#15050,#15051,#15052));
#2899=EDGE_LOOP('',(#15053));
#2900=EDGE_LOOP('',(#15054));
#2901=EDGE_LOOP('',(#15055,#15056,#15057,#15058));
#2902=EDGE_LOOP('',(#15059,#15060,#15061,#15062));
#2903=EDGE_LOOP('',(#15063));
#2904=EDGE_LOOP('',(#15064));
#2905=EDGE_LOOP('',(#15065,#15066,#15067,#15068));
#2906=EDGE_LOOP('',(#15069,#15070,#15071,#15072));
#2907=EDGE_LOOP('',(#15073));
#2908=EDGE_LOOP('',(#15074));
#2909=EDGE_LOOP('',(#15075,#15076,#15077,#15078));
#2910=EDGE_LOOP('',(#15079,#15080,#15081,#15082));
#2911=EDGE_LOOP('',(#15083,#15084,#15085));
#2912=EDGE_LOOP('',(#15086,#15087,#15088,#15089,#15090,#15091,#15092,#15093));
#2913=EDGE_LOOP('',(#15094,#15095,#15096,#15097,#15098));
#2914=EDGE_LOOP('',(#15099,#15100,#15101,#15102,#15103,#15104));
#2915=EDGE_LOOP('',(#15105,#15106,#15107,#15108,#15109,#15110));
#2916=EDGE_LOOP('',(#15111,#15112,#15113,#15114,#15115,#15116));
#2917=EDGE_LOOP('',(#15117,#15118,#15119,#15120,#15121));
#2918=EDGE_LOOP('',(#15122));
#2919=EDGE_LOOP('',(#15123));
#2920=EDGE_LOOP('',(#15124));
#2921=EDGE_LOOP('',(#15125));
#2922=EDGE_LOOP('',(#15126));
#2923=EDGE_LOOP('',(#15127));
#2924=EDGE_LOOP('',(#15128));
#2925=EDGE_LOOP('',(#15129));
#2926=EDGE_LOOP('',(#15130,#15131,#15132,#15133));
#2927=EDGE_LOOP('',(#15134,#15135,#15136,#15137));
#2928=EDGE_LOOP('',(#15138,#15139,#15140,#15141));
#2929=EDGE_LOOP('',(#15142,#15143,#15144,#15145,#15146));
#2930=EDGE_LOOP('',(#15147,#15148,#15149,#15150,#15151,#15152));
#2931=EDGE_LOOP('',(#15153,#15154,#15155,#15156,#15157));
#2932=EDGE_LOOP('',(#15158,#15159,#15160,#15161,#15162,#15163));
#2933=EDGE_LOOP('',(#15164,#15165,#15166,#15167,#15168,#15169));
#2934=EDGE_LOOP('',(#15170,#15171,#15172,#15173,#15174));
#2935=EDGE_LOOP('',(#15175,#15176,#15177,#15178,#15179,#15180));
#2936=EDGE_LOOP('',(#15181,#15182,#15183,#15184,#15185,#15186));
#2937=EDGE_LOOP('',(#15187,#15188,#15189,#15190,#15191,#15192,#15193,#15194,
#15195));
#2938=EDGE_LOOP('',(#15196,#15197,#15198,#15199,#15200,#15201,#15202,#15203,
#15204,#15205,#15206,#15207,#15208,#15209,#15210,#15211,#15212,#15213,#15214,
#15215,#15216,#15217,#15218));
#2939=EDGE_LOOP('',(#15219,#15220,#15221,#15222,#15223));
#2940=EDGE_LOOP('',(#15224,#15225,#15226,#15227,#15228,#15229,#15230,#15231,
#15232,#15233,#15234,#15235,#15236,#15237,#15238,#15239,#15240,#15241,#15242,
#15243,#15244,#15245,#15246,#15247,#15248,#15249,#15250,#15251,#15252,#15253,
#15254,#15255,#15256,#15257));
#2941=EDGE_LOOP('',(#15258));
#2942=EDGE_LOOP('',(#15259));
#2943=EDGE_LOOP('',(#15260));
#2944=EDGE_LOOP('',(#15261));
#2945=EDGE_LOOP('',(#15262,#15263,#15264,#15265,#15266));
#2946=EDGE_LOOP('',(#15267,#15268,#15269,#15270,#15271));
#2947=EDGE_LOOP('',(#15272,#15273,#15274,#15275,#15276));
#2948=EDGE_LOOP('',(#15277,#15278,#15279,#15280,#15281));
#2949=EDGE_LOOP('',(#15282,#15283,#15284,#15285,#15286));
#2950=EDGE_LOOP('',(#15287,#15288,#15289,#15290,#15291,#15292));
#2951=EDGE_LOOP('',(#15293,#15294,#15295,#15296,#15297,#15298));
#2952=EDGE_LOOP('',(#15299,#15300,#15301,#15302,#15303));
#2953=EDGE_LOOP('',(#15304,#15305,#15306,#15307,#15308));
#2954=EDGE_LOOP('',(#15309,#15310,#15311,#15312));
#2955=EDGE_LOOP('',(#15313,#15314,#15315,#15316));
#2956=EDGE_LOOP('',(#15317,#15318,#15319,#15320));
#2957=EDGE_LOOP('',(#15321));
#2958=EDGE_LOOP('',(#15322));
#2959=EDGE_LOOP('',(#15323));
#2960=EDGE_LOOP('',(#15324,#15325,#15326,#15327,#15328,#15329,#15330,#15331));
#2961=EDGE_LOOP('',(#15332,#15333));
#2962=EDGE_LOOP('',(#15334,#15335));
#2963=EDGE_LOOP('',(#15336,#15337));
#2964=EDGE_LOOP('',(#15338,#15339,#15340,#15341));
#2965=EDGE_LOOP('',(#15342,#15343));
#2966=EDGE_LOOP('',(#15344,#15345,#15346,#15347));
#2967=EDGE_LOOP('',(#15348,#15349,#15350,#15351));
#2968=EDGE_LOOP('',(#15352,#15353,#15354,#15355));
#2969=EDGE_LOOP('',(#15356,#15357,#15358,#15359));
#2970=EDGE_LOOP('',(#15360,#15361,#15362,#15363));
#2971=EDGE_LOOP('',(#15364,#15365,#15366,#15367,#15368));
#2972=EDGE_LOOP('',(#15369,#15370,#15371,#15372,#15373,#15374));
#2973=EDGE_LOOP('',(#15375,#15376,#15377,#15378,#15379,#15380,#15381,#15382,
#15383,#15384,#15385,#15386,#15387,#15388,#15389,#15390,#15391,#15392,#15393,
#15394,#15395,#15396,#15397,#15398,#15399,#15400,#15401,#15402,#15403,#15404,
#15405,#15406,#15407,#15408,#15409,#15410,#15411,#15412,#15413,#15414,#15415,
#15416,#15417,#15418,#15419,#15420,#15421,#15422,#15423,#15424,#15425,#15426,
#15427,#15428,#15429,#15430));
#2974=EDGE_LOOP('',(#15431));
#2975=EDGE_LOOP('',(#15432,#15433,#15434,#15435,#15436));
#2976=EDGE_LOOP('',(#15437,#15438,#15439,#15440,#15441,#15442,#15443,#15444,
#15445,#15446,#15447,#15448,#15449,#15450,#15451,#15452,#15453,#15454,#15455,
#15456,#15457,#15458,#15459,#15460,#15461,#15462,#15463,#15464,#15465,#15466,
#15467,#15468,#15469,#15470,#15471,#15472,#15473,#15474,#15475,#15476,#15477,
#15478,#15479,#15480,#15481,#15482,#15483,#15484,#15485,#15486,#15487,#15488,
#15489,#15490,#15491,#15492,#15493,#15494,#15495,#15496,#15497,#15498,#15499,
#15500,#15501,#15502,#15503,#15504,#15505,#15506,#15507,#15508,#15509,#15510,
#15511,#15512,#15513,#15514,#15515,#15516,#15517,#15518,#15519,#15520,#15521,
#15522,#15523,#15524,#15525,#15526,#15527,#15528,#15529,#15530,#15531,#15532,
#15533,#15534,#15535,#15536));
#2977=EDGE_LOOP('',(#15537));
#2978=EDGE_LOOP('',(#15538,#15539,#15540,#15541,#15542));
#2979=EDGE_LOOP('',(#15543,#15544,#15545,#15546));
#2980=EDGE_LOOP('',(#15547,#15548,#15549,#15550,#15551));
#2981=EDGE_LOOP('',(#15552,#15553,#15554,#15555));
#2982=EDGE_LOOP('',(#15556,#15557,#15558,#15559));
#2983=EDGE_LOOP('',(#15560,#15561,#15562,#15563,#15564));
#2984=EDGE_LOOP('',(#15565,#15566,#15567,#15568));
#2985=EDGE_LOOP('',(#15569,#15570,#15571,#15572,#15573));
#2986=EDGE_LOOP('',(#15574,#15575,#15576,#15577,#15578,#15579,#15580,#15581,
#15582,#15583,#15584,#15585,#15586,#15587,#15588,#15589,#15590,#15591,#15592,
#15593,#15594,#15595,#15596,#15597,#15598,#15599,#15600,#15601,#15602,#15603,
#15604,#15605,#15606,#15607,#15608,#15609,#15610,#15611,#15612,#15613,#15614,
#15615,#15616,#15617,#15618,#15619,#15620,#15621,#15622,#15623,#15624,#15625,
#15626,#15627,#15628,#15629,#15630,#15631,#15632,#15633,#15634,#15635,#15636,
#15637,#15638,#15639,#15640,#15641,#15642,#15643,#15644,#15645,#15646,#15647,
#15648,#15649,#15650,#15651,#15652,#15653,#15654,#15655,#15656,#15657,#15658,
#15659,#15660,#15661,#15662,#15663,#15664,#15665,#15666,#15667,#15668,#15669,
#15670,#15671,#15672,#15673));
#2987=EDGE_LOOP('',(#15674,#15675,#15676,#15677,#15678,#15679,#15680,#15681,
#15682,#15683,#15684,#15685,#15686,#15687,#15688,#15689,#15690,#15691,#15692,
#15693,#15694,#15695,#15696,#15697,#15698,#15699,#15700,#15701,#15702,#15703,
#15704,#15705,#15706,#15707,#15708,#15709,#15710,#15711,#15712,#15713,#15714,
#15715,#15716,#15717,#15718,#15719,#15720,#15721,#15722,#15723,#15724,#15725,
#15726,#15727,#15728,#15729));
#2988=EDGE_LOOP('',(#15730,#15731,#15732,#15733));
#2989=EDGE_LOOP('',(#15734,#15735,#15736,#15737));
#2990=EDGE_LOOP('',(#15738,#15739,#15740,#15741,#15742));
#2991=EDGE_LOOP('',(#15743,#15744,#15745,#15746));
#2992=EDGE_LOOP('',(#15747,#15748,#15749,#15750,#15751));
#2993=EDGE_LOOP('',(#15752,#15753,#15754,#15755));
#2994=EDGE_LOOP('',(#15756,#15757,#15758,#15759));
#2995=EDGE_LOOP('',(#15760,#15761,#15762,#15763,#15764));
#2996=EDGE_LOOP('',(#15765,#15766,#15767,#15768));
#2997=EDGE_LOOP('',(#15769,#15770,#15771,#15772,#15773));
#2998=EDGE_LOOP('',(#15774,#15775,#15776,#15777));
#2999=EDGE_LOOP('',(#15778,#15779,#15780,#15781));
#3000=EDGE_LOOP('',(#15782,#15783,#15784,#15785,#15786));
#3001=EDGE_LOOP('',(#15787,#15788,#15789,#15790));
#3002=EDGE_LOOP('',(#15791,#15792,#15793,#15794,#15795));
#3003=EDGE_LOOP('',(#15796,#15797,#15798,#15799));
#3004=EDGE_LOOP('',(#15800,#15801,#15802,#15803));
#3005=EDGE_LOOP('',(#15804,#15805,#15806,#15807,#15808));
#3006=EDGE_LOOP('',(#15809,#15810,#15811,#15812));
#3007=EDGE_LOOP('',(#15813,#15814,#15815,#15816,#15817));
#3008=EDGE_LOOP('',(#15818,#15819,#15820,#15821));
#3009=EDGE_LOOP('',(#15822,#15823,#15824,#15825));
#3010=EDGE_LOOP('',(#15826,#15827,#15828,#15829,#15830));
#3011=EDGE_LOOP('',(#15831,#15832,#15833,#15834));
#3012=EDGE_LOOP('',(#15835,#15836,#15837,#15838,#15839));
#3013=EDGE_LOOP('',(#15840,#15841,#15842,#15843));
#3014=EDGE_LOOP('',(#15844,#15845,#15846,#15847));
#3015=EDGE_LOOP('',(#15848,#15849,#15850,#15851,#15852));
#3016=EDGE_LOOP('',(#15853,#15854,#15855,#15856));
#3017=EDGE_LOOP('',(#15857,#15858,#15859,#15860,#15861));
#3018=EDGE_LOOP('',(#15862,#15863,#15864,#15865));
#3019=EDGE_LOOP('',(#15866,#15867,#15868,#15869));
#3020=EDGE_LOOP('',(#15870,#15871,#15872,#15873,#15874));
#3021=EDGE_LOOP('',(#15875,#15876,#15877,#15878));
#3022=EDGE_LOOP('',(#15879,#15880,#15881,#15882,#15883));
#3023=EDGE_LOOP('',(#15884,#15885,#15886,#15887));
#3024=EDGE_LOOP('',(#15888,#15889,#15890,#15891));
#3025=EDGE_LOOP('',(#15892,#15893,#15894,#15895,#15896));
#3026=EDGE_LOOP('',(#15897,#15898,#15899,#15900));
#3027=EDGE_LOOP('',(#15901,#15902,#15903,#15904,#15905));
#3028=EDGE_LOOP('',(#15906,#15907,#15908,#15909));
#3029=EDGE_LOOP('',(#15910,#15911,#15912,#15913));
#3030=EDGE_LOOP('',(#15914,#15915,#15916,#15917,#15918));
#3031=EDGE_LOOP('',(#15919,#15920,#15921,#15922));
#3032=EDGE_LOOP('',(#15923,#15924,#15925,#15926,#15927));
#3033=EDGE_LOOP('',(#15928,#15929,#15930,#15931));
#3034=EDGE_LOOP('',(#15932,#15933,#15934,#15935));
#3035=EDGE_LOOP('',(#15936,#15937,#15938,#15939,#15940));
#3036=EDGE_LOOP('',(#15941,#15942,#15943,#15944));
#3037=EDGE_LOOP('',(#15945,#15946,#15947,#15948,#15949));
#3038=EDGE_LOOP('',(#15950,#15951,#15952,#15953));
#3039=EDGE_LOOP('',(#15954,#15955,#15956,#15957));
#3040=EDGE_LOOP('',(#15958,#15959,#15960,#15961,#15962));
#3041=EDGE_LOOP('',(#15963,#15964,#15965,#15966));
#3042=EDGE_LOOP('',(#15967,#15968,#15969,#15970,#15971));
#3043=EDGE_LOOP('',(#15972,#15973,#15974,#15975));
#3044=EDGE_LOOP('',(#15976,#15977,#15978,#15979));
#3045=EDGE_LOOP('',(#15980,#15981,#15982,#15983,#15984));
#3046=EDGE_LOOP('',(#15985,#15986,#15987,#15988));
#3047=EDGE_LOOP('',(#15989,#15990,#15991,#15992,#15993));
#3048=EDGE_LOOP('',(#15994,#15995,#15996,#15997,#15998,#15999));
#3049=EDGE_LOOP('',(#16000,#16001,#16002,#16003));
#3050=EDGE_LOOP('',(#16004,#16005,#16006,#16007,#16008,#16009));
#3051=EDGE_LOOP('',(#16010,#16011,#16012,#16013));
#3052=EDGE_LOOP('',(#16014,#16015,#16016,#16017));
#3053=EDGE_LOOP('',(#16018,#16019,#16020,#16021));
#3054=EDGE_LOOP('',(#16022,#16023,#16024,#16025,#16026,#16027));
#3055=EDGE_LOOP('',(#16028,#16029,#16030,#16031));
#3056=EDGE_LOOP('',(#16032,#16033,#16034,#16035,#16036,#16037));
#3057=EDGE_LOOP('',(#16038,#16039,#16040,#16041));
#3058=EDGE_LOOP('',(#16042,#16043,#16044,#16045));
#3059=EDGE_LOOP('',(#16046,#16047,#16048,#16049));
#3060=EDGE_LOOP('',(#16050,#16051,#16052,#16053,#16054,#16055));
#3061=EDGE_LOOP('',(#16056,#16057,#16058,#16059));
#3062=EDGE_LOOP('',(#16060,#16061,#16062,#16063,#16064,#16065));
#3063=EDGE_LOOP('',(#16066,#16067,#16068,#16069));
#3064=EDGE_LOOP('',(#16070,#16071,#16072,#16073));
#3065=EDGE_LOOP('',(#16074,#16075,#16076,#16077));
#3066=EDGE_LOOP('',(#16078,#16079,#16080,#16081,#16082,#16083));
#3067=EDGE_LOOP('',(#16084,#16085,#16086,#16087));
#3068=EDGE_LOOP('',(#16088,#16089,#16090,#16091,#16092,#16093));
#3069=EDGE_LOOP('',(#16094,#16095,#16096,#16097));
#3070=EDGE_LOOP('',(#16098,#16099,#16100,#16101));
#3071=EDGE_LOOP('',(#16102,#16103,#16104,#16105));
#3072=EDGE_LOOP('',(#16106,#16107,#16108,#16109,#16110,#16111));
#3073=EDGE_LOOP('',(#16112,#16113,#16114,#16115));
#3074=EDGE_LOOP('',(#16116,#16117,#16118,#16119,#16120,#16121));
#3075=EDGE_LOOP('',(#16122,#16123,#16124,#16125));
#3076=EDGE_LOOP('',(#16126,#16127,#16128,#16129));
#3077=EDGE_LOOP('',(#16130,#16131,#16132,#16133));
#3078=EDGE_LOOP('',(#16134,#16135,#16136,#16137,#16138,#16139));
#3079=EDGE_LOOP('',(#16140,#16141,#16142,#16143));
#3080=EDGE_LOOP('',(#16144,#16145,#16146,#16147,#16148,#16149));
#3081=EDGE_LOOP('',(#16150,#16151,#16152,#16153));
#3082=EDGE_LOOP('',(#16154,#16155,#16156,#16157));
#3083=EDGE_LOOP('',(#16158,#16159,#16160,#16161));
#3084=EDGE_LOOP('',(#16162,#16163,#16164,#16165,#16166,#16167));
#3085=EDGE_LOOP('',(#16168,#16169,#16170,#16171));
#3086=EDGE_LOOP('',(#16172,#16173,#16174,#16175,#16176,#16177));
#3087=EDGE_LOOP('',(#16178,#16179,#16180,#16181));
#3088=EDGE_LOOP('',(#16182,#16183,#16184,#16185));
#3089=EDGE_LOOP('',(#16186,#16187,#16188,#16189));
#3090=EDGE_LOOP('',(#16190,#16191,#16192,#16193,#16194,#16195));
#3091=EDGE_LOOP('',(#16196,#16197,#16198,#16199));
#3092=EDGE_LOOP('',(#16200,#16201,#16202,#16203,#16204,#16205));
#3093=EDGE_LOOP('',(#16206,#16207,#16208,#16209));
#3094=EDGE_LOOP('',(#16210,#16211,#16212,#16213));
#3095=EDGE_LOOP('',(#16214,#16215,#16216,#16217));
#3096=EDGE_LOOP('',(#16218,#16219,#16220,#16221,#16222,#16223));
#3097=EDGE_LOOP('',(#16224,#16225,#16226,#16227));
#3098=EDGE_LOOP('',(#16228,#16229,#16230,#16231,#16232,#16233));
#3099=EDGE_LOOP('',(#16234,#16235,#16236,#16237));
#3100=EDGE_LOOP('',(#16238,#16239,#16240,#16241));
#3101=EDGE_LOOP('',(#16242,#16243,#16244,#16245));
#3102=EDGE_LOOP('',(#16246,#16247,#16248,#16249,#16250,#16251));
#3103=EDGE_LOOP('',(#16252,#16253,#16254,#16255));
#3104=EDGE_LOOP('',(#16256,#16257,#16258,#16259,#16260,#16261));
#3105=EDGE_LOOP('',(#16262,#16263,#16264,#16265));
#3106=EDGE_LOOP('',(#16266,#16267,#16268,#16269));
#3107=EDGE_LOOP('',(#16270,#16271,#16272,#16273));
#3108=EDGE_LOOP('',(#16274,#16275,#16276,#16277,#16278,#16279));
#3109=EDGE_LOOP('',(#16280,#16281,#16282,#16283));
#3110=EDGE_LOOP('',(#16284,#16285,#16286,#16287,#16288,#16289));
#3111=EDGE_LOOP('',(#16290,#16291,#16292,#16293));
#3112=EDGE_LOOP('',(#16294,#16295,#16296,#16297));
#3113=EDGE_LOOP('',(#16298,#16299,#16300,#16301));
#3114=EDGE_LOOP('',(#16302,#16303,#16304,#16305,#16306,#16307));
#3115=EDGE_LOOP('',(#16308,#16309,#16310,#16311));
#3116=EDGE_LOOP('',(#16312,#16313,#16314,#16315,#16316,#16317));
#3117=EDGE_LOOP('',(#16318,#16319,#16320,#16321));
#3118=EDGE_LOOP('',(#16322,#16323,#16324,#16325));
#3119=EDGE_LOOP('',(#16326,#16327,#16328,#16329));
#3120=EDGE_LOOP('',(#16330,#16331,#16332,#16333,#16334,#16335));
#3121=EDGE_LOOP('',(#16336,#16337,#16338,#16339));
#3122=EDGE_LOOP('',(#16340,#16341,#16342,#16343,#16344,#16345));
#3123=EDGE_LOOP('',(#16346,#16347,#16348,#16349));
#3124=EDGE_LOOP('',(#16350,#16351,#16352,#16353));
#3125=EDGE_LOOP('',(#16354,#16355,#16356,#16357));
#3126=EDGE_LOOP('',(#16358,#16359,#16360,#16361,#16362,#16363));
#3127=EDGE_LOOP('',(#16364,#16365,#16366,#16367));
#3128=EDGE_LOOP('',(#16368,#16369,#16370,#16371,#16372,#16373));
#3129=EDGE_LOOP('',(#16374,#16375,#16376,#16377));
#3130=EDGE_LOOP('',(#16378,#16379,#16380,#16381));
#3131=EDGE_LOOP('',(#16382,#16383,#16384,#16385));
#3132=EDGE_LOOP('',(#16386,#16387,#16388,#16389,#16390,#16391));
#3133=EDGE_LOOP('',(#16392,#16393,#16394,#16395));
#3134=EDGE_LOOP('',(#16396,#16397,#16398,#16399,#16400,#16401));
#3135=EDGE_LOOP('',(#16402,#16403,#16404,#16405));
#3136=EDGE_LOOP('',(#16406,#16407,#16408,#16409));
#3137=EDGE_LOOP('',(#16410,#16411,#16412,#16413));
#3138=EDGE_LOOP('',(#16414,#16415,#16416,#16417,#16418,#16419));
#3139=EDGE_LOOP('',(#16420,#16421,#16422,#16423));
#3140=EDGE_LOOP('',(#16424,#16425,#16426,#16427,#16428,#16429));
#3141=EDGE_LOOP('',(#16430,#16431,#16432,#16433));
#3142=EDGE_LOOP('',(#16434,#16435,#16436,#16437));
#3143=EDGE_LOOP('',(#16438,#16439,#16440,#16441));
#3144=EDGE_LOOP('',(#16442,#16443,#16444,#16445,#16446,#16447));
#3145=EDGE_LOOP('',(#16448,#16449,#16450,#16451));
#3146=EDGE_LOOP('',(#16452,#16453,#16454,#16455,#16456,#16457));
#3147=EDGE_LOOP('',(#16458,#16459,#16460,#16461));
#3148=EDGE_LOOP('',(#16462,#16463,#16464,#16465));
#3149=EDGE_LOOP('',(#16466,#16467,#16468,#16469));
#3150=EDGE_LOOP('',(#16470,#16471,#16472,#16473,#16474,#16475));
#3151=EDGE_LOOP('',(#16476,#16477,#16478,#16479));
#3152=EDGE_LOOP('',(#16480,#16481,#16482,#16483,#16484,#16485));
#3153=EDGE_LOOP('',(#16486,#16487,#16488,#16489));
#3154=EDGE_LOOP('',(#16490,#16491,#16492,#16493));
#3155=EDGE_LOOP('',(#16494,#16495,#16496,#16497));
#3156=EDGE_LOOP('',(#16498,#16499,#16500,#16501,#16502,#16503));
#3157=EDGE_LOOP('',(#16504,#16505,#16506,#16507));
#3158=EDGE_LOOP('',(#16508,#16509,#16510,#16511,#16512,#16513));
#3159=EDGE_LOOP('',(#16514,#16515,#16516,#16517));
#3160=EDGE_LOOP('',(#16518,#16519,#16520,#16521));
#3161=EDGE_LOOP('',(#16522,#16523,#16524,#16525));
#3162=EDGE_LOOP('',(#16526,#16527,#16528,#16529,#16530,#16531));
#3163=EDGE_LOOP('',(#16532,#16533,#16534,#16535));
#3164=EDGE_LOOP('',(#16536,#16537,#16538,#16539,#16540,#16541));
#3165=EDGE_LOOP('',(#16542,#16543,#16544,#16545));
#3166=EDGE_LOOP('',(#16546,#16547,#16548,#16549));
#3167=EDGE_LOOP('',(#16550,#16551,#16552,#16553));
#3168=EDGE_LOOP('',(#16554,#16555,#16556,#16557,#16558,#16559));
#3169=EDGE_LOOP('',(#16560,#16561,#16562,#16563));
#3170=EDGE_LOOP('',(#16564,#16565,#16566,#16567,#16568,#16569));
#3171=EDGE_LOOP('',(#16570,#16571,#16572,#16573));
#3172=EDGE_LOOP('',(#16574,#16575,#16576,#16577));
#3173=EDGE_LOOP('',(#16578,#16579,#16580,#16581));
#3174=EDGE_LOOP('',(#16582,#16583,#16584,#16585,#16586,#16587));
#3175=EDGE_LOOP('',(#16588,#16589,#16590,#16591));
#3176=EDGE_LOOP('',(#16592,#16593,#16594,#16595,#16596,#16597));
#3177=EDGE_LOOP('',(#16598,#16599,#16600,#16601));
#3178=EDGE_LOOP('',(#16602,#16603,#16604,#16605));
#3179=EDGE_LOOP('',(#16606,#16607,#16608,#16609));
#3180=EDGE_LOOP('',(#16610,#16611,#16612,#16613,#16614,#16615));
#3181=EDGE_LOOP('',(#16616,#16617,#16618,#16619));
#3182=EDGE_LOOP('',(#16620,#16621,#16622,#16623,#16624,#16625));
#3183=EDGE_LOOP('',(#16626,#16627,#16628,#16629));
#3184=EDGE_LOOP('',(#16630,#16631,#16632,#16633));
#3185=EDGE_LOOP('',(#16634,#16635,#16636,#16637));
#3186=EDGE_LOOP('',(#16638,#16639,#16640,#16641,#16642,#16643));
#3187=EDGE_LOOP('',(#16644,#16645,#16646,#16647));
#3188=EDGE_LOOP('',(#16648,#16649,#16650,#16651,#16652,#16653));
#3189=EDGE_LOOP('',(#16654,#16655,#16656,#16657));
#3190=EDGE_LOOP('',(#16658,#16659,#16660,#16661));
#3191=EDGE_LOOP('',(#16662,#16663,#16664,#16665));
#3192=EDGE_LOOP('',(#16666,#16667,#16668,#16669,#16670,#16671));
#3193=EDGE_LOOP('',(#16672,#16673,#16674,#16675));
#3194=EDGE_LOOP('',(#16676,#16677,#16678,#16679,#16680,#16681));
#3195=EDGE_LOOP('',(#16682,#16683,#16684,#16685));
#3196=EDGE_LOOP('',(#16686,#16687,#16688,#16689));
#3197=EDGE_LOOP('',(#16690,#16691,#16692,#16693));
#3198=EDGE_LOOP('',(#16694,#16695,#16696,#16697));
#3199=EDGE_LOOP('',(#16698,#16699,#16700,#16701));
#3200=EDGE_LOOP('',(#16702,#16703,#16704,#16705,#16706));
#3201=EDGE_LOOP('',(#16707,#16708,#16709,#16710,#16711,#16712));
#3202=EDGE_LOOP('',(#16713));
#3203=EDGE_LOOP('',(#16714,#16715,#16716,#16717,#16718,#16719));
#3204=EDGE_LOOP('',(#16720,#16721,#16722,#16723,#16724,#16725));
#3205=EDGE_LOOP('',(#16726,#16727,#16728,#16729,#16730,#16731));
#3206=EDGE_LOOP('',(#16732,#16733,#16734,#16735,#16736,#16737));
#3207=EDGE_LOOP('',(#16738,#16739,#16740,#16741,#16742));
#3208=EDGE_LOOP('',(#16743));
#3209=EDGE_LOOP('',(#16744,#16745,#16746,#16747));
#3210=EDGE_LOOP('',(#16748,#16749,#16750,#16751));
#3211=EDGE_LOOP('',(#16752,#16753,#16754,#16755));
#3212=EDGE_LOOP('',(#16756,#16757,#16758,#16759));
#3213=EDGE_LOOP('',(#16760,#16761,#16762,#16763));
#3214=EDGE_LOOP('',(#16764,#16765,#16766,#16767));
#3215=EDGE_LOOP('',(#16768,#16769,#16770,#16771));
#3216=EDGE_LOOP('',(#16772));
#3217=EDGE_LOOP('',(#16773,#16774,#16775,#16776));
#3218=EDGE_LOOP('',(#16777,#16778,#16779,#16780));
#3219=EDGE_LOOP('',(#16781,#16782,#16783,#16784));
#3220=EDGE_LOOP('',(#16785,#16786,#16787,#16788));
#3221=EDGE_LOOP('',(#16789,#16790,#16791,#16792));
#3222=EDGE_LOOP('',(#16793,#16794,#16795,#16796));
#3223=EDGE_LOOP('',(#16797));
#3224=EDGE_LOOP('',(#16798,#16799,#16800,#16801));
#3225=EDGE_LOOP('',(#16802,#16803,#16804,#16805,#16806));
#3226=EDGE_LOOP('',(#16807,#16808,#16809,#16810,#16811));
#3227=EDGE_LOOP('',(#16812,#16813,#16814,#16815));
#3228=EDGE_LOOP('',(#16816,#16817,#16818,#16819,#16820));
#3229=EDGE_LOOP('',(#16821,#16822,#16823,#16824,#16825,#16826));
#3230=EDGE_LOOP('',(#16827));
#3231=EDGE_LOOP('',(#16828,#16829,#16830,#16831,#16832,#16833));
#3232=EDGE_LOOP('',(#16834,#16835,#16836,#16837,#16838,#16839));
#3233=EDGE_LOOP('',(#16840,#16841,#16842,#16843,#16844,#16845));
#3234=EDGE_LOOP('',(#16846,#16847,#16848,#16849,#16850,#16851));
#3235=EDGE_LOOP('',(#16852,#16853,#16854,#16855,#16856));
#3236=EDGE_LOOP('',(#16857));
#3237=EDGE_LOOP('',(#16858,#16859,#16860,#16861));
#3238=EDGE_LOOP('',(#16862));
#3239=EDGE_LOOP('',(#16863));
#3240=EDGE_LOOP('',(#16864,#16865,#16866,#16867,#16868,#16869));
#3241=EDGE_LOOP('',(#16870,#16871,#16872,#16873));
#3242=EDGE_LOOP('',(#16874,#16875,#16876));
#3243=EDGE_LOOP('',(#16877,#16878,#16879,#16880));
#3244=EDGE_LOOP('',(#16881,#16882,#16883,#16884));
#3245=EDGE_LOOP('',(#16885,#16886,#16887));
#3246=EDGE_LOOP('',(#16888,#16889,#16890));
#3247=EDGE_LOOP('',(#16891,#16892,#16893,#16894));
#3248=EDGE_LOOP('',(#16895,#16896,#16897));
#3249=EDGE_LOOP('',(#16898,#16899,#16900,#16901,#16902));
#3250=EDGE_LOOP('',(#16903,#16904,#16905,#16906));
#3251=EDGE_LOOP('',(#16907,#16908,#16909,#16910));
#3252=EDGE_LOOP('',(#16911,#16912,#16913,#16914));
#3253=EDGE_LOOP('',(#16915,#16916,#16917,#16918));
#3254=EDGE_LOOP('',(#16919,#16920,#16921));
#3255=EDGE_LOOP('',(#16922,#16923,#16924,#16925));
#3256=EDGE_LOOP('',(#16926,#16927,#16928,#16929));
#3257=EDGE_LOOP('',(#16930,#16931,#16932,#16933));
#3258=EDGE_LOOP('',(#16934,#16935,#16936,#16937));
#3259=EDGE_LOOP('',(#16938,#16939,#16940,#16941,#16942,#16943));
#3260=EDGE_LOOP('',(#16944,#16945,#16946,#16947));
#3261=EDGE_LOOP('',(#16948,#16949,#16950));
#3262=EDGE_LOOP('',(#16951,#16952,#16953,#16954));
#3263=EDGE_LOOP('',(#16955,#16956,#16957,#16958));
#3264=EDGE_LOOP('',(#16959,#16960,#16961));
#3265=EDGE_LOOP('',(#16962,#16963,#16964));
#3266=EDGE_LOOP('',(#16965,#16966,#16967,#16968,#16969));
#3267=EDGE_LOOP('',(#16970,#16971,#16972,#16973));
#3268=EDGE_LOOP('',(#16974,#16975,#16976,#16977));
#3269=EDGE_LOOP('',(#16978,#16979,#16980));
#3270=EDGE_LOOP('',(#16981,#16982,#16983,#16984));
#3271=EDGE_LOOP('',(#16985,#16986,#16987));
#3272=EDGE_LOOP('',(#16988,#16989,#16990,#16991));
#3273=EDGE_LOOP('',(#16992,#16993,#16994,#16995));
#3274=EDGE_LOOP('',(#16996,#16997,#16998,#16999));
#3275=EDGE_LOOP('',(#17000,#17001,#17002,#17003));
#3276=EDGE_LOOP('',(#17004,#17005,#17006,#17007,#17008));
#3277=EDGE_LOOP('',(#17009,#17010,#17011,#17012));
#3278=EDGE_LOOP('',(#17013,#17014,#17015));
#3279=EDGE_LOOP('',(#17016,#17017,#17018));
#3280=EDGE_LOOP('',(#17019,#17020,#17021,#17022));
#3281=EDGE_LOOP('',(#17023,#17024,#17025,#17026));
#3282=EDGE_LOOP('',(#17027,#17028,#17029,#17030));
#3283=EDGE_LOOP('',(#17031,#17032,#17033,#17034,#17035,#17036));
#3284=EDGE_LOOP('',(#17037,#17038,#17039,#17040));
#3285=EDGE_LOOP('',(#17041,#17042,#17043,#17044,#17045,#17046));
#3286=EDGE_LOOP('',(#17047,#17048,#17049));
#3287=EDGE_LOOP('',(#17050,#17051,#17052));
#3288=EDGE_LOOP('',(#17053,#17054,#17055,#17056,#17057));
#3289=EDGE_LOOP('',(#17058,#17059,#17060,#17061));
#3290=EDGE_LOOP('',(#17062,#17063,#17064,#17065));
#3291=EDGE_LOOP('',(#17066,#17067,#17068,#17069));
#3292=EDGE_LOOP('',(#17070,#17071,#17072,#17073));
#3293=EDGE_LOOP('',(#17074,#17075,#17076,#17077,#17078));
#3294=EDGE_LOOP('',(#17079,#17080,#17081,#17082,#17083,#17084,#17085,#17086,
#17087,#17088,#17089,#17090,#17091,#17092,#17093,#17094,#17095,#17096,#17097,
#17098,#17099));
#3295=EDGE_LOOP('',(#17100,#17101,#17102,#17103,#17104,#17105,#17106,#17107,
#17108,#17109,#17110,#17111,#17112,#17113,#17114,#17115,#17116,#17117,#17118,
#17119,#17120,#17121,#17122,#17123));
#3296=EDGE_LOOP('',(#17124));
#3297=EDGE_LOOP('',(#17125,#17126,#17127,#17128,#17129,#17130));
#3298=EDGE_LOOP('',(#17131,#17132,#17133,#17134,#17135));
#3299=EDGE_LOOP('',(#17136,#17137,#17138,#17139,#17140,#17141));
#3300=EDGE_LOOP('',(#17142));
#3301=EDGE_LOOP('',(#17143));
#3302=EDGE_LOOP('',(#17144,#17145,#17146));
#3303=EDGE_LOOP('',(#17147,#17148,#17149,#17150));
#3304=EDGE_LOOP('',(#17151,#17152,#17153,#17154));
#3305=EDGE_LOOP('',(#17155,#17156,#17157));
#3306=EDGE_LOOP('',(#17158,#17159,#17160,#17161));
#3307=EDGE_LOOP('',(#17162,#17163,#17164,#17165));
#3308=EDGE_LOOP('',(#17166,#17167,#17168,#17169,#17170,#17171));
#3309=EDGE_LOOP('',(#17172,#17173,#17174,#17175));
#3310=EDGE_LOOP('',(#17176,#17177,#17178,#17179));
#3311=EDGE_LOOP('',(#17180,#17181,#17182));
#3312=EDGE_LOOP('',(#17183,#17184,#17185));
#3313=EDGE_LOOP('',(#17186,#17187,#17188));
#3314=EDGE_LOOP('',(#17189,#17190,#17191,#17192));
#3315=EDGE_LOOP('',(#17193,#17194,#17195,#17196));
#3316=EDGE_LOOP('',(#17197,#17198,#17199,#17200));
#3317=EDGE_LOOP('',(#17201,#17202,#17203,#17204));
#3318=EDGE_LOOP('',(#17205,#17206,#17207,#17208));
#3319=EDGE_LOOP('',(#17209,#17210,#17211,#17212,#17213,#17214));
#3320=EDGE_LOOP('',(#17215,#17216,#17217,#17218,#17219,#17220));
#3321=EDGE_LOOP('',(#17221,#17222,#17223,#17224,#17225,#17226));
#3322=EDGE_LOOP('',(#17227,#17228,#17229,#17230,#17231));
#3323=EDGE_LOOP('',(#17232,#17233,#17234,#17235));
#3324=EDGE_LOOP('',(#17236,#17237,#17238,#17239,#17240));
#3325=EDGE_LOOP('',(#17241));
#3326=EDGE_LOOP('',(#17242));
#3327=EDGE_LOOP('',(#17243,#17244,#17245,#17246,#17247,#17248));
#3328=EDGE_LOOP('',(#17249,#17250,#17251));
#3329=EDGE_LOOP('',(#17252,#17253,#17254,#17255,#17256));
#3330=EDGE_LOOP('',(#17257,#17258,#17259,#17260));
#3331=EDGE_LOOP('',(#17261,#17262,#17263,#17264));
#3332=EDGE_LOOP('',(#17265,#17266,#17267,#17268));
#3333=EDGE_LOOP('',(#17269,#17270,#17271));
#3334=EDGE_LOOP('',(#17272,#17273,#17274,#17275,#17276));
#3335=EDGE_LOOP('',(#17277,#17278,#17279));
#3336=EDGE_LOOP('',(#17280,#17281,#17282,#17283));
#3337=EDGE_LOOP('',(#17284,#17285,#17286,#17287));
#3338=EDGE_LOOP('',(#17288,#17289,#17290,#17291,#17292));
#3339=EDGE_LOOP('',(#17293,#17294,#17295,#17296,#17297,#17298));
#3340=EDGE_LOOP('',(#17299,#17300,#17301,#17302,#17303));
#3341=EDGE_LOOP('',(#17304));
#3342=EDGE_LOOP('',(#17305));
#3343=EDGE_LOOP('',(#17306,#17307,#17308,#17309));
#3344=EDGE_LOOP('',(#17310,#17311,#17312,#17313));
#3345=EDGE_LOOP('',(#17314,#17315,#17316,#17317));
#3346=EDGE_LOOP('',(#17318,#17319,#17320,#17321,#17322,#17323));
#3347=EDGE_LOOP('',(#17324,#17325,#17326,#17327));
#3348=EDGE_LOOP('',(#17328,#17329,#17330,#17331));
#3349=EDGE_LOOP('',(#17332,#17333,#17334,#17335,#17336,#17337));
#3350=EDGE_LOOP('',(#17338,#17339,#17340));
#3351=EDGE_LOOP('',(#17341,#17342,#17343));
#3352=EDGE_LOOP('',(#17344,#17345,#17346));
#3353=EDGE_LOOP('',(#17347,#17348,#17349));
#3354=EDGE_LOOP('',(#17350,#17351,#17352,#17353));
#3355=EDGE_LOOP('',(#17354,#17355,#17356));
#3356=EDGE_LOOP('',(#17357,#17358,#17359));
#3357=EDGE_LOOP('',(#17360,#17361,#17362,#17363));
#3358=EDGE_LOOP('',(#17364,#17365,#17366));
#3359=EDGE_LOOP('',(#17367,#17368,#17369,#17370));
#3360=EDGE_LOOP('',(#17371,#17372,#17373,#17374));
#3361=EDGE_LOOP('',(#17375,#17376,#17377));
#3362=EDGE_LOOP('',(#17378,#17379,#17380,#17381));
#3363=EDGE_LOOP('',(#17382,#17383,#17384,#17385));
#3364=EDGE_LOOP('',(#17386,#17387,#17388,#17389));
#3365=EDGE_LOOP('',(#17390,#17391,#17392,#17393));
#3366=EDGE_LOOP('',(#17394,#17395,#17396,#17397));
#3367=EDGE_LOOP('',(#17398,#17399,#17400,#17401));
#3368=EDGE_LOOP('',(#17402,#17403,#17404,#17405));
#3369=EDGE_LOOP('',(#17406,#17407,#17408,#17409));
#3370=EDGE_LOOP('',(#17410,#17411,#17412,#17413));
#3371=EDGE_LOOP('',(#17414,#17415,#17416,#17417));
#3372=EDGE_LOOP('',(#17418,#17419,#17420,#17421));
#3373=EDGE_LOOP('',(#17422,#17423,#17424,#17425));
#3374=EDGE_LOOP('',(#17426,#17427,#17428,#17429));
#3375=EDGE_LOOP('',(#17430,#17431,#17432,#17433));
#3376=EDGE_LOOP('',(#17434,#17435,#17436,#17437));
#3377=EDGE_LOOP('',(#17438));
#3378=EDGE_LOOP('',(#17439));
#3379=EDGE_LOOP('',(#17440,#17441,#17442,#17443,#17444));
#3380=EDGE_LOOP('',(#17445,#17446,#17447,#17448,#17449,#17450));
#3381=EDGE_LOOP('',(#17451,#17452,#17453,#17454,#17455,#17456,#17457,#17458,
#17459,#17460,#17461,#17462,#17463,#17464,#17465,#17466,#17467,#17468,#17469,
#17470,#17471,#17472,#17473,#17474,#17475));
#3382=EDGE_LOOP('',(#17476));
#3383=EDGE_LOOP('',(#17477,#17478,#17479,#17480,#17481));
#3384=EDGE_LOOP('',(#17482,#17483,#17484,#17485,#17486,#17487,#17488,#17489,
#17490,#17491,#17492,#17493,#17494,#17495,#17496,#17497,#17498,#17499));
#3385=EDGE_LOOP('',(#17500));
#3386=EDGE_LOOP('',(#17501,#17502,#17503,#17504));
#3387=EDGE_LOOP('',(#17505,#17506,#17507,#17508));
#3388=EDGE_LOOP('',(#17509,#17510,#17511,#17512));
#3389=EDGE_LOOP('',(#17513,#17514,#17515,#17516));
#3390=EDGE_LOOP('',(#17517,#17518,#17519,#17520));
#3391=EDGE_LOOP('',(#17521,#17522,#17523,#17524));
#3392=EDGE_LOOP('',(#17525,#17526,#17527,#17528));
#3393=EDGE_LOOP('',(#17529,#17530,#17531,#17532));
#3394=EDGE_LOOP('',(#17533,#17534,#17535,#17536));
#3395=EDGE_LOOP('',(#17537,#17538,#17539,#17540));
#3396=EDGE_LOOP('',(#17541,#17542,#17543));
#3397=EDGE_LOOP('',(#17544,#17545,#17546,#17547));
#3398=EDGE_LOOP('',(#17548,#17549,#17550));
#3399=EDGE_LOOP('',(#17551,#17552,#17553));
#3400=EDGE_LOOP('',(#17554,#17555,#17556,#17557));
#3401=EDGE_LOOP('',(#17558,#17559,#17560,#17561));
#3402=EDGE_LOOP('',(#17562,#17563,#17564,#17565));
#3403=EDGE_LOOP('',(#17566,#17567,#17568,#17569));
#3404=EDGE_LOOP('',(#17570,#17571,#17572,#17573,#17574,#17575));
#3405=EDGE_LOOP('',(#17576,#17577,#17578,#17579,#17580));
#3406=EDGE_LOOP('',(#17581,#17582,#17583));
#3407=EDGE_LOOP('',(#17584,#17585,#17586,#17587));
#3408=EDGE_LOOP('',(#17588,#17589,#17590,#17591));
#3409=EDGE_LOOP('',(#17592,#17593,#17594,#17595,#17596,#17597,#17598,#17599,
#17600,#17601,#17602,#17603,#17604,#17605,#17606,#17607,#17608,#17609,#17610,
#17611,#17612));
#3410=EDGE_LOOP('',(#17613,#17614,#17615,#17616,#17617));
#3411=EDGE_LOOP('',(#17618,#17619,#17620));
#3412=EDGE_LOOP('',(#17621,#17622,#17623));
#3413=EDGE_LOOP('',(#17624,#17625,#17626,#17627));
#3414=EDGE_LOOP('',(#17628,#17629,#17630,#17631));
#3415=EDGE_LOOP('',(#17632,#17633,#17634,#17635));
#3416=EDGE_LOOP('',(#17636,#17637,#17638,#17639));
#3417=EDGE_LOOP('',(#17640,#17641,#17642,#17643));
#3418=EDGE_LOOP('',(#17644,#17645,#17646,#17647,#17648,#17649));
#3419=EDGE_LOOP('',(#17650,#17651,#17652));
#3420=EDGE_LOOP('',(#17653,#17654,#17655,#17656));
#3421=EDGE_LOOP('',(#17657,#17658,#17659));
#3422=EDGE_LOOP('',(#17660,#17661,#17662));
#3423=EDGE_LOOP('',(#17663,#17664,#17665));
#3424=EDGE_LOOP('',(#17666,#17667,#17668,#17669));
#3425=EDGE_LOOP('',(#17670,#17671,#17672,#17673));
#3426=EDGE_LOOP('',(#17674,#17675,#17676,#17677,#17678));
#3427=EDGE_LOOP('',(#17679,#17680,#17681,#17682,#17683));
#3428=EDGE_LOOP('',(#17684,#17685,#17686,#17687,#17688,#17689));
#3429=EDGE_LOOP('',(#17690,#17691,#17692,#17693));
#3430=EDGE_LOOP('',(#17694,#17695,#17696,#17697,#17698));
#3431=EDGE_LOOP('',(#17699,#17700,#17701,#17702,#17703,#17704));
#3432=EDGE_LOOP('',(#17705,#17706,#17707));
#3433=EDGE_LOOP('',(#17708,#17709,#17710));
#3434=EDGE_LOOP('',(#17711,#17712,#17713,#17714));
#3435=EDGE_LOOP('',(#17715,#17716,#17717,#17718,#17719,#17720));
#3436=EDGE_LOOP('',(#17721,#17722,#17723,#17724,#17725));
#3437=EDGE_LOOP('',(#17726,#17727,#17728));
#3438=EDGE_LOOP('',(#17729,#17730,#17731,#17732));
#3439=EDGE_LOOP('',(#17733,#17734,#17735,#17736,#17737));
#3440=EDGE_LOOP('',(#17738,#17739,#17740,#17741));
#3441=EDGE_LOOP('',(#17742,#17743,#17744));
#3442=EDGE_LOOP('',(#17745,#17746,#17747,#17748,#17749,#17750));
#3443=EDGE_LOOP('',(#17751,#17752,#17753,#17754));
#3444=EDGE_LOOP('',(#17755,#17756,#17757,#17758));
#3445=EDGE_LOOP('',(#17759,#17760,#17761,#17762));
#3446=EDGE_LOOP('',(#17763,#17764,#17765));
#3447=EDGE_LOOP('',(#17766,#17767,#17768,#17769));
#3448=EDGE_LOOP('',(#17770,#17771,#17772,#17773,#17774,#17775));
#3449=EDGE_LOOP('',(#17776,#17777,#17778,#17779,#17780,#17781));
#3450=EDGE_LOOP('',(#17782,#17783,#17784,#17785));
#3451=EDGE_LOOP('',(#17786,#17787,#17788,#17789));
#3452=EDGE_LOOP('',(#17790,#17791,#17792,#17793,#17794,#17795));
#3453=EDGE_LOOP('',(#17796,#17797,#17798));
#3454=EDGE_LOOP('',(#17799,#17800,#17801,#17802));
#3455=EDGE_LOOP('',(#17803,#17804,#17805,#17806,#17807,#17808,#17809,#17810,
#17811,#17812,#17813,#17814,#17815,#17816,#17817,#17818,#17819,#17820,#17821,
#17822,#17823,#17824,#17825,#17826,#17827,#17828,#17829,#17830,#17831,#17832,
#17833,#17834,#17835,#17836,#17837,#17838));
#3456=EDGE_LOOP('',(#17839,#17840,#17841,#17842));
#3457=EDGE_LOOP('',(#17843,#17844,#17845,#17846,#17847,#17848));
#3458=EDGE_LOOP('',(#17849,#17850,#17851,#17852));
#3459=EDGE_LOOP('',(#17853,#17854,#17855,#17856));
#3460=EDGE_LOOP('',(#17857,#17858,#17859,#17860,#17861,#17862));
#3461=EDGE_LOOP('',(#17863,#17864,#17865,#17866));
#3462=EDGE_LOOP('',(#17867,#17868,#17869,#17870));
#3463=EDGE_LOOP('',(#17871,#17872,#17873,#17874,#17875));
#3464=EDGE_LOOP('',(#17876,#17877,#17878));
#3465=EDGE_LOOP('',(#17879,#17880,#17881,#17882));
#3466=EDGE_LOOP('',(#17883,#17884,#17885,#17886,#17887,#17888,#17889));
#3467=EDGE_LOOP('',(#17890,#17891,#17892,#17893));
#3468=EDGE_LOOP('',(#17894,#17895,#17896,#17897,#17898,#17899));
#3469=EDGE_LOOP('',(#17900,#17901,#17902,#17903,#17904,#17905));
#3470=EDGE_LOOP('',(#17906,#17907,#17908,#17909));
#3471=EDGE_LOOP('',(#17910,#17911,#17912,#17913));
#3472=EDGE_LOOP('',(#17914,#17915,#17916));
#3473=EDGE_LOOP('',(#17917,#17918,#17919,#17920,#17921));
#3474=EDGE_LOOP('',(#17922,#17923,#17924,#17925,#17926));
#3475=EDGE_LOOP('',(#17927,#17928,#17929,#17930));
#3476=EDGE_LOOP('',(#17931,#17932,#17933,#17934));
#3477=EDGE_LOOP('',(#17935,#17936,#17937,#17938));
#3478=EDGE_LOOP('',(#17939,#17940,#17941));
#3479=EDGE_LOOP('',(#17942,#17943,#17944));
#3480=EDGE_LOOP('',(#17945,#17946,#17947,#17948));
#3481=EDGE_LOOP('',(#17949,#17950,#17951,#17952));
#3482=EDGE_LOOP('',(#17953,#17954,#17955,#17956));
#3483=EDGE_LOOP('',(#17957,#17958,#17959,#17960,#17961,#17962));
#3484=EDGE_LOOP('',(#17963,#17964,#17965,#17966,#17967));
#3485=EDGE_LOOP('',(#17968,#17969,#17970,#17971,#17972,#17973));
#3486=EDGE_LOOP('',(#17974,#17975,#17976,#17977,#17978,#17979));
#3487=EDGE_LOOP('',(#17980,#17981,#17982,#17983));
#3488=EDGE_LOOP('',(#17984,#17985,#17986,#17987,#17988,#17989,#17990,#17991,
#17992,#17993,#17994,#17995,#17996,#17997,#17998));
#3489=EDGE_LOOP('',(#17999,#18000,#18001,#18002,#18003,#18004));
#3490=EDGE_LOOP('',(#18005,#18006,#18007,#18008));
#3491=EDGE_LOOP('',(#18009,#18010,#18011,#18012,#18013,#18014));
#3492=EDGE_LOOP('',(#18015,#18016,#18017,#18018,#18019,#18020,#18021,#18022,
#18023,#18024,#18025,#18026,#18027,#18028,#18029,#18030,#18031));
#3493=EDGE_LOOP('',(#18032,#18033,#18034,#18035));
#3494=EDGE_LOOP('',(#18036,#18037,#18038,#18039,#18040,#18041,#18042,#18043,
#18044,#18045,#18046,#18047,#18048,#18049,#18050));
#3495=EDGE_LOOP('',(#18051,#18052,#18053,#18054));
#3496=EDGE_LOOP('',(#18055,#18056,#18057,#18058,#18059,#18060,#18061,#18062,
#18063,#18064,#18065,#18066,#18067,#18068,#18069));
#3497=EDGE_LOOP('',(#18070,#18071,#18072,#18073));
#3498=EDGE_LOOP('',(#18074,#18075,#18076,#18077,#18078,#18079,#18080,#18081,
#18082,#18083,#18084,#18085,#18086,#18087,#18088));
#3499=EDGE_LOOP('',(#18089,#18090,#18091,#18092,#18093));
#3500=EDGE_LOOP('',(#18094,#18095,#18096,#18097));
#3501=EDGE_LOOP('',(#18098,#18099,#18100));
#3502=EDGE_LOOP('',(#18101,#18102,#18103,#18104));
#3503=EDGE_LOOP('',(#18105,#18106,#18107,#18108));
#3504=EDGE_LOOP('',(#18109,#18110,#18111,#18112));
#3505=EDGE_LOOP('',(#18113,#18114,#18115,#18116));
#3506=EDGE_LOOP('',(#18117,#18118,#18119,#18120));
#3507=EDGE_LOOP('',(#18121,#18122,#18123,#18124));
#3508=EDGE_LOOP('',(#18125,#18126,#18127,#18128));
#3509=EDGE_LOOP('',(#18129,#18130,#18131,#18132));
#3510=EDGE_LOOP('',(#18133,#18134,#18135,#18136));
#3511=EDGE_LOOP('',(#18137,#18138,#18139,#18140));
#3512=EDGE_LOOP('',(#18141,#18142,#18143,#18144));
#3513=EDGE_LOOP('',(#18145,#18146,#18147,#18148));
#3514=EDGE_LOOP('',(#18149,#18150,#18151,#18152));
#3515=EDGE_LOOP('',(#18153,#18154,#18155,#18156));
#3516=EDGE_LOOP('',(#18157,#18158,#18159,#18160));
#3517=EDGE_LOOP('',(#18161,#18162,#18163,#18164));
#3518=EDGE_LOOP('',(#18165,#18166,#18167,#18168));
#3519=EDGE_LOOP('',(#18169,#18170,#18171,#18172,#18173));
#3520=EDGE_LOOP('',(#18174,#18175,#18176));
#3521=EDGE_LOOP('',(#18177,#18178,#18179,#18180));
#3522=EDGE_LOOP('',(#18181,#18182,#18183,#18184));
#3523=EDGE_LOOP('',(#18185,#18186,#18187,#18188,#18189,#18190,#18191,#18192,
#18193,#18194,#18195));
#3524=EDGE_LOOP('',(#18196,#18197,#18198,#18199,#18200,#18201,#18202,#18203,
#18204,#18205,#18206));
#3525=EDGE_LOOP('',(#18207,#18208,#18209,#18210,#18211,#18212));
#3526=EDGE_LOOP('',(#18213,#18214,#18215,#18216,#18217,#18218,#18219,#18220,
#18221,#18222,#18223));
#3527=EDGE_LOOP('',(#18224,#18225,#18226,#18227));
#3528=EDGE_LOOP('',(#18228,#18229,#18230,#18231));
#3529=EDGE_LOOP('',(#18232,#18233,#18234,#18235));
#3530=EDGE_LOOP('',(#18236,#18237,#18238,#18239));
#3531=EDGE_LOOP('',(#18240,#18241,#18242,#18243));
#3532=EDGE_LOOP('',(#18244,#18245,#18246,#18247));
#3533=EDGE_LOOP('',(#18248,#18249,#18250,#18251,#18252,#18253));
#3534=EDGE_LOOP('',(#18254,#18255,#18256,#18257));
#3535=EDGE_LOOP('',(#18258,#18259,#18260,#18261,#18262,#18263,#18264,#18265,
#18266,#18267,#18268,#18269,#18270,#18271,#18272));
#3536=EDGE_LOOP('',(#18273,#18274,#18275,#18276,#18277,#18278,#18279,#18280,
#18281,#18282,#18283,#18284,#18285,#18286,#18287));
#3537=EDGE_LOOP('',(#18288,#18289,#18290,#18291));
#3538=EDGE_LOOP('',(#18292,#18293,#18294,#18295));
#3539=EDGE_LOOP('',(#18296,#18297,#18298,#18299,#18300,#18301));
#3540=EDGE_LOOP('',(#18302,#18303,#18304,#18305));
#3541=EDGE_LOOP('',(#18306,#18307,#18308,#18309));
#3542=CIRCLE('',#20144,6.933);
#3543=CIRCLE('',#20145,6.933);
#3544=CIRCLE('',#20146,6.933);
#3545=CIRCLE('',#20147,6.933);
#3546=CIRCLE('',#20148,6.933);
#3547=CIRCLE('',#20149,6.933);
#3548=CIRCLE('',#20150,6.933);
#3549=CIRCLE('',#20151,6.933);
#3550=CIRCLE('',#20152,6.933);
#3551=CIRCLE('',#20215,6.933);
#3552=CIRCLE('',#20216,6.933);
#3553=CIRCLE('',#20217,6.933);
#3554=CIRCLE('',#20234,6.21925);
#3555=CIRCLE('',#20251,6.21925);
#3556=CIRCLE('',#20253,6.21925);
#3557=CIRCLE('',#20320,6.933);
#3558=CIRCLE('',#20321,6.933);
#3559=CIRCLE('',#20323,6.21925);
#3560=CIRCLE('',#20326,6.933);
#3561=CIRCLE('',#20327,6.933);
#3562=CIRCLE('',#20329,6.21925);
#3563=CIRCLE('',#20332,6.933);
#3564=CIRCLE('',#20334,10.125);
#3565=CIRCLE('',#20335,7.8125);
#3566=CIRCLE('',#20337,7.8125);
#3567=CIRCLE('',#20339,10.125);
#3568=CIRCLE('',#20341,10.625);
#3569=CIRCLE('',#20342,10.125);
#3570=CIRCLE('',#20344,10.125);
#3571=CIRCLE('',#20345,10.625);
#3572=CIRCLE('',#20347,10.625);
#3573=CIRCLE('',#20349,10.125);
#3574=CIRCLE('',#20351,10.125);
#3575=CIRCLE('',#20352,7.8125);
#3576=CIRCLE('',#20354,7.8125);
#3577=CIRCLE('',#20356,10.125);
#3578=CIRCLE('',#20358,10.625);
#3579=CIRCLE('',#20359,10.125);
#3580=CIRCLE('',#20361,10.625);
#3581=CIRCLE('',#20363,10.125);
#3582=CIRCLE('',#20365,10.125);
#3583=CIRCLE('',#20366,7.8125);
#3584=CIRCLE('',#20368,7.8125);
#3585=CIRCLE('',#20370,10.125);
#3586=CIRCLE('',#20372,10.625);
#3587=CIRCLE('',#20373,10.125);
#3588=CIRCLE('',#20375,10.625);
#3589=CIRCLE('',#20377,10.125);
#3590=CIRCLE('',#20379,10.125);
#3591=CIRCLE('',#20380,7.8125);
#3592=CIRCLE('',#20382,7.8125);
#3593=CIRCLE('',#20384,10.125);
#3594=CIRCLE('',#20386,10.625);
#3595=CIRCLE('',#20387,10.125);
#3596=CIRCLE('',#20389,10.625);
#3597=CIRCLE('',#20391,10.125);
#3598=CIRCLE('',#20393,10.125);
#3599=CIRCLE('',#20394,7.8125);
#3600=CIRCLE('',#20396,7.8125);
#3601=CIRCLE('',#20398,10.125);
#3602=CIRCLE('',#20400,10.625);
#3603=CIRCLE('',#20401,10.125);
#3604=CIRCLE('',#20403,10.625);
#3605=CIRCLE('',#20405,10.125);
#3606=CIRCLE('',#20407,10.125);
#3607=CIRCLE('',#20408,7.8125);
#3608=CIRCLE('',#20410,7.8125);
#3609=CIRCLE('',#20412,10.125);
#3610=CIRCLE('',#20414,10.625);
#3611=CIRCLE('',#20415,10.125);
#3612=CIRCLE('',#20417,10.625);
#3613=CIRCLE('',#20419,10.125);
#3614=CIRCLE('',#20421,10.125);
#3615=CIRCLE('',#20422,7.8125);
#3616=CIRCLE('',#20424,7.8125);
#3617=CIRCLE('',#20426,10.125);
#3618=CIRCLE('',#20428,10.625);
#3619=CIRCLE('',#20429,10.125);
#3620=CIRCLE('',#20431,10.625);
#3621=CIRCLE('',#20433,10.125);
#3622=CIRCLE('',#20435,10.125);
#3623=CIRCLE('',#20436,10.125);
#3624=CIRCLE('',#20437,7.8125);
#3625=CIRCLE('',#20439,7.8125);
#3626=CIRCLE('',#20441,10.125);
#3627=CIRCLE('',#20442,10.125);
#3628=CIRCLE('',#20444,10.625);
#3629=CIRCLE('',#20445,10.125);
#3630=CIRCLE('',#20447,10.625);
#3631=CIRCLE('',#20449,10.125);
#3632=CIRCLE('',#20451,10.125);
#3633=CIRCLE('',#20452,7.8125);
#3634=CIRCLE('',#20454,7.8125);
#3635=CIRCLE('',#20456,10.125);
#3636=CIRCLE('',#20458,10.625);
#3637=CIRCLE('',#20459,10.125);
#3638=CIRCLE('',#20461,10.625);
#3639=CIRCLE('',#20463,10.125);
#3640=CIRCLE('',#20465,10.125);
#3641=CIRCLE('',#20466,7.8125);
#3642=CIRCLE('',#20468,7.8125);
#3643=CIRCLE('',#20470,10.125);
#3644=CIRCLE('',#20472,10.625);
#3645=CIRCLE('',#20473,10.125);
#3646=CIRCLE('',#20475,10.625);
#3647=CIRCLE('',#20477,10.125);
#3648=CIRCLE('',#20479,10.125);
#3649=CIRCLE('',#20480,7.8125);
#3650=CIRCLE('',#20482,7.8125);
#3651=CIRCLE('',#20484,10.125);
#3652=CIRCLE('',#20486,10.625);
#3653=CIRCLE('',#20487,10.125);
#3654=CIRCLE('',#20489,10.625);
#3655=CIRCLE('',#20491,10.125);
#3656=CIRCLE('',#20493,10.125);
#3657=CIRCLE('',#20494,7.8125);
#3658=CIRCLE('',#20496,7.8125);
#3659=CIRCLE('',#20498,10.125);
#3660=CIRCLE('',#20500,10.625);
#3661=CIRCLE('',#20501,10.125);
#3662=CIRCLE('',#20503,10.625);
#3663=CIRCLE('',#20505,10.125);
#3664=CIRCLE('',#20507,10.125);
#3665=CIRCLE('',#20508,7.8125);
#3666=CIRCLE('',#20510,7.8125);
#3667=CIRCLE('',#20512,10.125);
#3668=CIRCLE('',#20514,10.625);
#3669=CIRCLE('',#20515,10.125);
#3670=CIRCLE('',#20517,10.625);
#3671=CIRCLE('',#20519,10.125);
#3672=CIRCLE('',#20521,10.125);
#3673=CIRCLE('',#20522,7.8125);
#3674=CIRCLE('',#20524,7.8125);
#3675=CIRCLE('',#20526,10.125);
#3676=CIRCLE('',#20528,10.625);
#3677=CIRCLE('',#20529,10.125);
#3678=CIRCLE('',#20531,10.625);
#3679=CIRCLE('',#20533,10.125);
#3680=CIRCLE('',#20535,10.125);
#3681=CIRCLE('',#20536,7.8125);
#3682=CIRCLE('',#20538,7.8125);
#3683=CIRCLE('',#20540,10.125);
#3684=CIRCLE('',#20542,10.625);
#3685=CIRCLE('',#20543,10.125);
#3686=CIRCLE('',#20546,6.);
#3687=CIRCLE('',#20551,6.933);
#3688=CIRCLE('',#20553,6.);
#3689=CIRCLE('',#20557,0.499999999999999);
#3690=CIRCLE('',#20558,0.500000000000002);
#3691=CIRCLE('',#20560,0.499999999999999);
#3692=CIRCLE('',#20561,0.499999999999998);
#3693=CIRCLE('',#20562,0.499999999999997);
#3694=CIRCLE('',#20564,0.499999999999999);
#3695=CIRCLE('',#20565,0.499999999999998);
#3696=CIRCLE('',#20567,0.499999999999997);
#3697=CIRCLE('',#20568,0.5);
#3698=CIRCLE('',#20570,0.500000000000001);
#3699=CIRCLE('',#20572,0.500000000000001);
#3700=CIRCLE('',#20573,0.499999999999999);
#3701=CIRCLE('',#20574,0.499999999999999);
#3702=CIRCLE('',#20575,0.5);
#3703=CIRCLE('',#20577,0.499999999999998);
#3704=CIRCLE('',#20579,0.499999999999999);
#3705=CIRCLE('',#20580,0.499999999999999);
#3706=CIRCLE('',#20582,0.499999999999999);
#3707=CIRCLE('',#20584,0.499999999999998);
#3708=CIRCLE('',#20587,0.5);
#3709=CIRCLE('',#20590,0.499999999999999);
#3710=CIRCLE('',#20594,0.499999999999999);
#3711=CIRCLE('',#20596,0.5);
#3712=CIRCLE('',#20599,0.5);
#3713=CIRCLE('',#20604,0.499999999999999);
#3714=CIRCLE('',#20606,0.500000000000001);
#3715=CIRCLE('',#20608,0.5);
#3716=CIRCLE('',#20609,0.5);
#3717=CIRCLE('',#20611,0.499999999999999);
#3718=CIRCLE('',#20613,0.5);
#3719=CIRCLE('',#20615,0.5);
#3720=CIRCLE('',#20618,0.500000000000001);
#3721=CIRCLE('',#20619,0.499999999999998);
#3722=CIRCLE('',#20620,0.499999999999999);
#3723=CIRCLE('',#20621,0.499999999999998);
#3724=CIRCLE('',#20624,0.5);
#3725=CIRCLE('',#20626,0.499999999999999);
#3726=CIRCLE('',#20628,0.499999999999997);
#3727=CIRCLE('',#20630,0.499999999999999);
#3728=CIRCLE('',#20632,0.499999999999998);
#3729=CIRCLE('',#20635,0.500000000000001);
#3730=CIRCLE('',#20639,0.5);
#3731=CIRCLE('',#20645,0.500000000000002);
#3732=CIRCLE('',#20647,0.500000000000002);
#3733=CIRCLE('',#20649,0.499999999999999);
#3734=CIRCLE('',#20653,0.499999999999996);
#3735=CIRCLE('',#20655,0.499999999999998);
#3736=CIRCLE('',#20657,0.5);
#3737=CIRCLE('',#20660,0.499999999999999);
#3738=CIRCLE('',#20661,0.5);
#3739=CIRCLE('',#20663,0.499999999999995);
#3740=CIRCLE('',#20664,0.499999999999999);
#3741=CIRCLE('',#20666,0.500000000000001);
#3742=CIRCLE('',#20667,0.499999999999998);
#3743=CIRCLE('',#20668,0.499999999999998);
#3744=CIRCLE('',#20672,0.499999999999999);
#3745=CIRCLE('',#20673,0.499999999999998);
#3746=CIRCLE('',#20675,0.500000000000001);
#3747=CIRCLE('',#20677,0.499999999999999);
#3748=CIRCLE('',#20678,0.5);
#3749=CIRCLE('',#20680,0.499999999999999);
#3750=CIRCLE('',#20682,0.499999999999999);
#3751=CIRCLE('',#20684,0.500000000000001);
#3752=CIRCLE('',#20686,0.499999999999998);
#3753=CIRCLE('',#20689,0.499999999999999);
#3754=CIRCLE('',#20692,0.5);
#3755=CIRCLE('',#20695,0.500000000000005);
#3756=CIRCLE('',#20697,0.499999999999999);
#3757=CIRCLE('',#20700,0.499999999999993);
#3758=CIRCLE('',#20701,0.5);
#3759=CIRCLE('',#20703,0.499999999999999);
#3760=CIRCLE('',#20706,0.499999999999999);
#3761=CIRCLE('',#20709,0.499999999999998);
#3762=CIRCLE('',#20710,0.499999999999999);
#3763=CIRCLE('',#20713,0.5);
#3764=CIRCLE('',#20717,0.499999999999998);
#3765=CIRCLE('',#20718,0.499999999999998);
#3766=CIRCLE('',#20720,0.499999999999997);
#3767=CIRCLE('',#20721,0.5);
#3768=CIRCLE('',#20723,0.499999999999998);
#3769=CIRCLE('',#20725,0.5);
#3770=CIRCLE('',#20731,0.499999999999993);
#3771=CIRCLE('',#20733,0.499999999999999);
#3772=CIRCLE('',#20735,0.499999999999999);
#3773=CIRCLE('',#20738,0.5);
#3774=CIRCLE('',#20740,0.5);
#3775=CIRCLE('',#20742,0.499999999999999);
#3776=CIRCLE('',#20743,0.5);
#3777=CIRCLE('',#20746,0.499999999999995);
#3778=CIRCLE('',#20749,0.5);
#3779=CIRCLE('',#20757,0.499999999999999);
#3780=CIRCLE('',#20760,0.5);
#3781=CIRCLE('',#20762,0.499999999999999);
#3782=CIRCLE('',#20763,0.499999999999999);
#3783=CIRCLE('',#20765,0.500000000000001);
#3784=CIRCLE('',#20766,0.5);
#3785=CIRCLE('',#20767,0.5);
#3786=CIRCLE('',#20769,0.500000000000001);
#3787=CIRCLE('',#20770,0.5);
#3788=CIRCLE('',#20771,0.499999999999999);
#3789=CIRCLE('',#20773,0.5);
#3790=CIRCLE('',#20775,0.500000000000001);
#3791=CIRCLE('',#20777,0.499999999999998);
#3792=CIRCLE('',#20780,0.500000000000005);
#3793=CIRCLE('',#20782,0.499999999999999);
#3794=CIRCLE('',#20783,0.5);
#3795=CIRCLE('',#20785,0.499999999999999);
#3796=CIRCLE('',#20786,0.500000000000001);
#3797=CIRCLE('',#20788,0.5);
#3798=CIRCLE('',#20793,0.5);
#3799=CIRCLE('',#20796,0.499999999999998);
#3800=CIRCLE('',#20800,0.499999999999997);
#3801=CIRCLE('',#20804,0.5);
#3802=CIRCLE('',#20807,0.499999999999999);
#3803=CIRCLE('',#20810,0.499999999999996);
#3804=CIRCLE('',#20812,0.499999999999996);
#3805=CIRCLE('',#20814,0.5);
#3806=CIRCLE('',#20823,0.499999999999999);
#3807=CIRCLE('',#20825,0.499999999999998);
#3808=CIRCLE('',#20828,0.5);
#3809=CIRCLE('',#20830,0.5);
#3810=CIRCLE('',#20834,0.499999999999998);
#3811=CIRCLE('',#20835,0.499999999999998);
#3812=CIRCLE('',#20837,0.499999999999999);
#3813=CIRCLE('',#20840,0.5);
#3814=CIRCLE('',#20844,44.);
#3815=CIRCLE('',#20845,0.5);
#3816=CIRCLE('',#20846,43.5);
#3817=CIRCLE('',#20847,44.);
#3818=CIRCLE('',#20849,44.);
#3819=CIRCLE('',#20850,44.);
#3820=CIRCLE('',#20851,44.);
#3821=CIRCLE('',#20852,44.);
#3822=CIRCLE('',#20853,44.);
#3823=CIRCLE('',#20854,44.);
#3824=CIRCLE('',#20855,44.);
#3825=CIRCLE('',#20856,44.);
#3826=CIRCLE('',#20857,44.);
#3827=CIRCLE('',#20859,42.4);
#3828=CIRCLE('',#20861,0.499999999999997);
#3829=CIRCLE('',#20863,0.499999999999997);
#3830=CIRCLE('',#20864,3.5);
#3831=CIRCLE('',#20865,3.);
#3832=CIRCLE('',#20867,0.500000000000001);
#3833=CIRCLE('',#20869,0.499999999999997);
#3834=CIRCLE('',#20870,0.5);
#3835=CIRCLE('',#20872,0.499999999999997);
#3836=CIRCLE('',#20873,0.5);
#3837=CIRCLE('',#20874,0.500000000000001);
#3838=CIRCLE('',#20875,0.5);
#3839=CIRCLE('',#20876,0.5);
#3840=CIRCLE('',#20878,42.9928932188135);
#3841=CIRCLE('',#20879,3.5);
#3842=CIRCLE('',#20880,42.9928932188135);
#3843=CIRCLE('',#20881,3.5);
#3844=CIRCLE('',#20882,42.9928932188135);
#3845=CIRCLE('',#20883,3.5);
#3846=CIRCLE('',#20884,42.9928932188135);
#3847=CIRCLE('',#20885,7.75710678118654);
#3848=CIRCLE('',#20887,43.3464466094067);
#3849=CIRCLE('',#20888,0.500000000000002);
#3850=CIRCLE('',#20890,43.8535533905933);
#3851=CIRCLE('',#20892,0.499999999999987);
#3852=CIRCLE('',#20894,0.5);
#3853=CIRCLE('',#20896,0.499999999999997);
#3854=CIRCLE('',#20898,0.499999999999995);
#3855=CIRCLE('',#20899,3.);
#3856=CIRCLE('',#20903,0.500000000000007);
#3857=CIRCLE('',#20904,43.3464466094067);
#3858=CIRCLE('',#20906,43.3464466094068);
#3859=CIRCLE('',#20909,43.8535533905933);
#3860=CIRCLE('',#20911,0.5);
#3861=CIRCLE('',#20912,0.500000000000001);
#3862=CIRCLE('',#20913,0.500000000000001);
#3863=CIRCLE('',#20915,0.5);
#3864=CIRCLE('',#20917,0.500000000000001);
#3865=CIRCLE('',#20918,0.500000000000001);
#3866=CIRCLE('',#20919,0.5);
#3867=CIRCLE('',#20921,0.5);
#3868=CIRCLE('',#20922,0.500000000000002);
#3869=CIRCLE('',#20925,43.8535533905933);
#3870=CIRCLE('',#20932,0.499999999999999);
#3871=CIRCLE('',#20933,0.499999999999997);
#3872=CIRCLE('',#20935,0.499999999999997);
#3873=CIRCLE('',#20937,0.499999999999999);
#3874=CIRCLE('',#20939,0.499999999999997);
#3875=CIRCLE('',#20943,0.499999999999991);
#3876=CIRCLE('',#20944,0.499999999999999);
#3877=CIRCLE('',#20945,0.500000000000004);
#3878=CIRCLE('',#20947,0.499999999999995);
#3879=CIRCLE('',#20948,0.5);
#3880=CIRCLE('',#20950,0.5);
#3881=CIRCLE('',#20952,43.8535533905933);
#3882=CIRCLE('',#20953,0.5);
#3883=CIRCLE('',#20955,43.3464466094067);
#3884=CIRCLE('',#20957,43.5);
#3885=CIRCLE('',#20959,3.);
#3886=CIRCLE('',#20960,1.75);
#3887=CIRCLE('',#20962,0.500000000000003);
#3888=CIRCLE('',#20963,0.500000000000004);
#3889=CIRCLE('',#20964,0.499999999999997);
#3890=CIRCLE('',#20966,0.5);
#3891=CIRCLE('',#20968,0.500000000000007);
#3892=CIRCLE('',#20970,0.499999999999997);
#3893=CIRCLE('',#20972,0.499999999999997);
#3894=CIRCLE('',#20973,3.);
#3895=CIRCLE('',#20976,0.499999999999995);
#3896=CIRCLE('',#20980,0.500000000000001);
#3897=CIRCLE('',#20982,3.);
#3898=CIRCLE('',#20984,3.);
#3899=CIRCLE('',#20986,0.5);
#3900=CIRCLE('',#20987,1.25);
#3901=CIRCLE('',#20989,1.25);
#3902=CIRCLE('',#20990,1.25);
#3903=CIRCLE('',#20992,0.499999999999996);
#3904=CIRCLE('',#20993,0.499999999999999);
#3905=CIRCLE('',#20994,0.499999999999998);
#3906=CIRCLE('',#20999,0.5);
#3907=CIRCLE('',#21006,0.499999999999999);
#3908=CIRCLE('',#21011,0.499999999999998);
#3909=CIRCLE('',#21013,0.499999999999997);
#3910=CIRCLE('',#21014,0.499999999999999);
#3911=CIRCLE('',#21021,43.5);
#3912=CIRCLE('',#21023,3.);
#3913=CIRCLE('',#21024,1.75);
#3914=CIRCLE('',#21026,0.5);
#3915=CIRCLE('',#21027,1.25);
#3916=CIRCLE('',#21029,1.25);
#3917=CIRCLE('',#21030,1.25);
#3918=CIRCLE('',#21032,0.499999999999997);
#3919=CIRCLE('',#21033,0.5);
#3920=CIRCLE('',#21035,0.5);
#3921=CIRCLE('',#21037,0.499999999999996);
#3922=CIRCLE('',#21039,0.500000000000003);
#3923=CIRCLE('',#21041,0.499999999999999);
#3924=CIRCLE('',#21043,0.500000000000003);
#3925=CIRCLE('',#21044,0.499999999999999);
#3926=CIRCLE('',#21045,0.5);
#3927=CIRCLE('',#21047,0.5);
#3928=CIRCLE('',#21050,0.499999999999997);
#3929=CIRCLE('',#21052,0.500000000000002);
#3930=CIRCLE('',#21054,0.500000000000001);
#3931=CIRCLE('',#21060,44.);
#3932=CIRCLE('',#21061,0.5);
#3933=CIRCLE('',#21062,43.5);
#3934=CIRCLE('',#21063,44.);
#3935=CIRCLE('',#21065,44.);
#3936=CIRCLE('',#21066,44.);
#3937=CIRCLE('',#21068,42.4);
#3938=CIRCLE('',#21070,43.8535533905933);
#3939=CIRCLE('',#21071,43.8535533905933);
#3940=CIRCLE('',#21072,0.5);
#3941=CIRCLE('',#21074,43.3464466094067);
#3942=CIRCLE('',#21075,43.3464466094067);
#3943=CIRCLE('',#21077,43.5);
#3944=CIRCLE('',#21079,3.);
#3945=CIRCLE('',#21080,1.75);
#3946=CIRCLE('',#21082,43.5);
#3947=CIRCLE('',#21084,1.75);
#3948=CIRCLE('',#21086,0.499999999999999);
#3949=CIRCLE('',#21091,0.499999999999999);
#3950=CIRCLE('',#21093,0.499999999999998);
#3951=CIRCLE('',#21098,0.5);
#3952=CIRCLE('',#21099,1.25);
#3953=CIRCLE('',#21101,1.25);
#3954=CIRCLE('',#21102,1.25);
#3955=CIRCLE('',#21104,0.5);
#3956=CIRCLE('',#21105,1.25);
#3957=CIRCLE('',#21107,1.25);
#3958=CIRCLE('',#21108,1.25);
#3959=CIRCLE('',#21110,3.5);
#3960=CIRCLE('',#21111,0.5);
#3961=CIRCLE('',#21112,3.);
#3962=CIRCLE('',#21113,3.);
#3963=CIRCLE('',#21115,42.9928932188134);
#3964=CIRCLE('',#21116,3.5);
#3965=CIRCLE('',#21117,1.75);
#3966=CIRCLE('',#21118,3.5);
#3967=CIRCLE('',#21119,1.75);
#3968=CIRCLE('',#21120,4.5);
#3969=CIRCLE('',#21121,4.5);
#3970=CIRCLE('',#21122,4.5);
#3971=CIRCLE('',#21123,7.55);
#3972=CIRCLE('',#21124,1.75);
#3973=CIRCLE('',#21125,1.75);
#3974=CIRCLE('',#21127,3.);
#3975=CIRCLE('',#21129,0.5);
#3976=CIRCLE('',#21130,3.);
#3977=CIRCLE('',#21131,3.);
#3978=CIRCLE('',#21133,3.);
#3979=CIRCLE('',#21135,0.5);
#3980=CIRCLE('',#21137,0.5);
#3981=CIRCLE('',#21139,0.5);
#3982=CIRCLE('',#21141,0.5);
#3983=CIRCLE('',#21142,3.);
#3984=CIRCLE('',#21143,3.);
#3985=CIRCLE('',#21145,3.);
#3986=CIRCLE('',#21147,0.5);
#3987=CIRCLE('',#21149,0.5);
#3988=CIRCLE('',#21151,3.);
#3989=CIRCLE('',#21152,0.5);
#3990=CIRCLE('',#21153,3.5);
#3991=CIRCLE('',#21155,3.);
#3992=CIRCLE('',#21157,5.);
#3993=CIRCLE('',#21159,3.);
#3994=CIRCLE('',#21160,0.5);
#3995=CIRCLE('',#21161,3.5);
#3996=CIRCLE('',#21163,3.);
#3997=CIRCLE('',#21165,5.);
#3998=CIRCLE('',#21167,3.);
#3999=CIRCLE('',#21168,0.5);
#4000=CIRCLE('',#21169,3.5);
#4001=CIRCLE('',#21171,3.);
#4002=CIRCLE('',#21173,5.);
#4003=CIRCLE('',#21175,0.499999999999999);
#4004=CIRCLE('',#21177,0.499999999999999);
#4005=CIRCLE('',#21179,0.499999999999998);
#4006=CIRCLE('',#21182,0.5);
#4007=CIRCLE('',#21184,44.);
#4008=CIRCLE('',#21185,44.);
#4009=CIRCLE('',#21186,0.5);
#4010=CIRCLE('',#21187,43.8535533905933);
#4011=CIRCLE('',#21188,43.8535533905933);
#4012=CIRCLE('',#21190,43.5464466094067);
#4013=CIRCLE('',#21191,43.5464466094067);
#4014=CIRCLE('',#21193,44.);
#4015=CIRCLE('',#21194,44.);
#4016=CIRCLE('',#21196,0.5);
#4017=CIRCLE('',#21197,43.1928932188135);
#4018=CIRCLE('',#21199,3.5);
#4019=CIRCLE('',#21200,3.5);
#4020=CIRCLE('',#21201,4.5);
#4021=CIRCLE('',#21202,4.5);
#4022=CIRCLE('',#21203,4.5);
#4023=CIRCLE('',#21204,12.5);
#4024=CIRCLE('',#21205,3.5);
#4025=CIRCLE('',#21207,0.5);
#4026=CIRCLE('',#21209,0.5);
#4027=CIRCLE('',#21211,0.5);
#4028=CIRCLE('',#21213,7.05);
#4029=CIRCLE('',#21214,7.05);
#4030=CIRCLE('',#21215,0.5);
#4031=CIRCLE('',#21217,7.05);
#4032=CIRCLE('',#21218,7.05);
#4033=CIRCLE('',#21220,7.40355339059327);
#4034=CIRCLE('',#21221,0.5);
#4035=CIRCLE('',#21222,7.40355339059327);
#4036=CIRCLE('',#21224,7.19644660940673);
#4037=CIRCLE('',#21225,7.19644660940673);
#4038=CIRCLE('',#21227,0.5);
#4039=CIRCLE('',#21229,0.5);
#4040=CIRCLE('',#21230,12.);
#4041=CIRCLE('',#21231,12.);
#4042=CIRCLE('',#21233,12.);
#4043=CIRCLE('',#21234,12.);
#4044=CIRCLE('',#21236,43.8535533905933);
#4045=CIRCLE('',#21237,43.8535533905933);
#4046=CIRCLE('',#21238,0.5);
#4047=CIRCLE('',#21240,43.5464466094067);
#4048=CIRCLE('',#21241,43.5464466094067);
#4049=CIRCLE('',#21242,43.4);
#4050=CIRCLE('',#21244,43.1928932188135);
#4051=CIRCLE('',#21245,43.1928932188135);
#4052=CIRCLE('',#21246,43.1928932188135);
#4053=CIRCLE('',#21247,43.1928932188135);
#4054=CIRCLE('',#21248,43.1928932188135);
#4055=CIRCLE('',#21249,43.1928932188135);
#4056=CIRCLE('',#21250,43.1928932188135);
#4057=CIRCLE('',#21252,5.5);
#4058=CIRCLE('',#21253,0.5);
#4059=CIRCLE('',#21254,5.);
#4060=CIRCLE('',#21255,5.);
#4061=CIRCLE('',#21257,5.5);
#4062=CIRCLE('',#21258,12.7071067811865);
#4063=CIRCLE('',#21259,5.5);
#4064=CIRCLE('',#21262,0.5);
#4065=CIRCLE('',#21263,5.);
#4066=CIRCLE('',#21264,5.);
#4067=CIRCLE('',#21267,0.5);
#4068=CIRCLE('',#21268,5.);
#4069=CIRCLE('',#21269,5.);
#4070=CIRCLE('',#21272,12.1464466094067);
#4071=CIRCLE('',#21273,0.5);
#4072=CIRCLE('',#21274,12.1464466094067);
#4073=CIRCLE('',#21276,12.3535533905933);
#4074=CIRCLE('',#21277,12.3535533905933);
#4075=CIRCLE('',#21279,0.5);
#4076=CIRCLE('',#21300,3.03);
#4077=CIRCLE('',#21301,3.03);
#4078=CIRCLE('',#21302,3.33);
#4079=CIRCLE('',#21304,3.03);
#4080=CIRCLE('',#21305,3.03);
#4081=CIRCLE('',#21307,7.1875);
#4082=CIRCLE('',#21308,9.5);
#4083=CIRCLE('',#21309,7.1875);
#4084=CIRCLE('',#21310,9.5);
#4085=CIRCLE('',#21311,7.1875);
#4086=CIRCLE('',#21312,9.5);
#4087=CIRCLE('',#21313,7.1875);
#4088=CIRCLE('',#21314,9.5);
#4089=CIRCLE('',#21315,7.1875);
#4090=CIRCLE('',#21316,9.5);
#4091=CIRCLE('',#21317,7.1875);
#4092=CIRCLE('',#21318,9.5);
#4093=CIRCLE('',#21319,7.1875);
#4094=CIRCLE('',#21320,9.5);
#4095=CIRCLE('',#21321,7.1875);
#4096=CIRCLE('',#21322,9.5);
#4097=CIRCLE('',#21323,7.1875);
#4098=CIRCLE('',#21324,9.5);
#4099=CIRCLE('',#21325,7.1875);
#4100=CIRCLE('',#21326,9.5);
#4101=CIRCLE('',#21327,7.1875);
#4102=CIRCLE('',#21328,9.5);
#4103=CIRCLE('',#21329,7.1875);
#4104=CIRCLE('',#21330,9.5);
#4105=CIRCLE('',#21331,7.1875);
#4106=CIRCLE('',#21332,9.5);
#4107=CIRCLE('',#21333,7.1875);
#4108=CIRCLE('',#21334,9.5);
#4109=CIRCLE('',#21336,3.33);
#4110=CIRCLE('',#21338,14.0625);
#4111=CIRCLE('',#21339,16.375);
#4112=CIRCLE('',#21340,14.0625);
#4113=CIRCLE('',#21341,16.375);
#4114=CIRCLE('',#21342,14.0625);
#4115=CIRCLE('',#21343,16.375);
#4116=CIRCLE('',#21344,14.0625);
#4117=CIRCLE('',#21345,16.375);
#4118=CIRCLE('',#21346,14.0625);
#4119=CIRCLE('',#21347,16.375);
#4120=CIRCLE('',#21348,14.0625);
#4121=CIRCLE('',#21349,16.375);
#4122=CIRCLE('',#21350,14.0625);
#4123=CIRCLE('',#21351,16.375);
#4124=CIRCLE('',#21352,14.0625);
#4125=CIRCLE('',#21353,16.375);
#4126=CIRCLE('',#21354,14.0625);
#4127=CIRCLE('',#21355,16.375);
#4128=CIRCLE('',#21356,14.0625);
#4129=CIRCLE('',#21357,16.375);
#4130=CIRCLE('',#21358,14.0625);
#4131=CIRCLE('',#21359,16.375);
#4132=CIRCLE('',#21360,14.0625);
#4133=CIRCLE('',#21361,16.375);
#4134=CIRCLE('',#21362,14.0625);
#4135=CIRCLE('',#21363,16.375);
#4136=CIRCLE('',#21364,14.0625);
#4137=CIRCLE('',#21365,16.375);
#4138=CIRCLE('',#21366,14.0625);
#4139=CIRCLE('',#21367,16.375);
#4140=CIRCLE('',#21368,14.0625);
#4141=CIRCLE('',#21369,16.375);
#4142=CIRCLE('',#21370,14.0625);
#4143=CIRCLE('',#21371,16.375);
#4144=CIRCLE('',#21372,14.0625);
#4145=CIRCLE('',#21373,16.375);
#4146=CIRCLE('',#21374,14.0625);
#4147=CIRCLE('',#21375,16.375);
#4148=CIRCLE('',#21376,14.0625);
#4149=CIRCLE('',#21377,16.375);
#4150=CIRCLE('',#21378,14.0625);
#4151=CIRCLE('',#21379,16.375);
#4152=CIRCLE('',#21380,14.0625);
#4153=CIRCLE('',#21381,16.375);
#4154=CIRCLE('',#21382,14.0625);
#4155=CIRCLE('',#21383,16.375);
#4156=CIRCLE('',#21384,14.0625);
#4157=CIRCLE('',#21385,16.375);
#4158=CIRCLE('',#21386,14.0625);
#4159=CIRCLE('',#21387,16.375);
#4160=CIRCLE('',#21389,7.1875);
#4161=CIRCLE('',#21391,10.);
#4162=CIRCLE('',#21393,10.);
#4163=CIRCLE('',#21395,7.1875);
#4164=CIRCLE('',#21397,16.375);
#4165=CIRCLE('',#21398,14.0625);
#4166=CIRCLE('',#21399,16.375);
#4167=CIRCLE('',#21400,14.0625);
#4168=CIRCLE('',#21401,16.375);
#4169=CIRCLE('',#21402,14.0625);
#4170=CIRCLE('',#21403,16.375);
#4171=CIRCLE('',#21404,14.0625);
#4172=CIRCLE('',#21405,16.375);
#4173=CIRCLE('',#21406,14.0625);
#4174=CIRCLE('',#21407,16.375);
#4175=CIRCLE('',#21408,14.0625);
#4176=CIRCLE('',#21409,16.375);
#4177=CIRCLE('',#21410,14.0625);
#4178=CIRCLE('',#21411,16.375);
#4179=CIRCLE('',#21412,14.0625);
#4180=CIRCLE('',#21413,16.375);
#4181=CIRCLE('',#21414,14.0625);
#4182=CIRCLE('',#21415,16.375);
#4183=CIRCLE('',#21416,14.0625);
#4184=CIRCLE('',#21417,16.375);
#4185=CIRCLE('',#21418,14.0625);
#4186=CIRCLE('',#21419,16.375);
#4187=CIRCLE('',#21420,14.0625);
#4188=CIRCLE('',#21421,16.375);
#4189=CIRCLE('',#21422,14.0625);
#4190=CIRCLE('',#21423,16.375);
#4191=CIRCLE('',#21424,14.0625);
#4192=CIRCLE('',#21425,16.375);
#4193=CIRCLE('',#21426,14.0625);
#4194=CIRCLE('',#21427,16.375);
#4195=CIRCLE('',#21428,14.0625);
#4196=CIRCLE('',#21429,16.375);
#4197=CIRCLE('',#21430,14.0625);
#4198=CIRCLE('',#21431,16.375);
#4199=CIRCLE('',#21432,14.0625);
#4200=CIRCLE('',#21433,16.375);
#4201=CIRCLE('',#21434,14.0625);
#4202=CIRCLE('',#21435,16.375);
#4203=CIRCLE('',#21436,14.0625);
#4204=CIRCLE('',#21437,16.375);
#4205=CIRCLE('',#21438,14.0625);
#4206=CIRCLE('',#21439,16.375);
#4207=CIRCLE('',#21440,14.0625);
#4208=CIRCLE('',#21441,16.375);
#4209=CIRCLE('',#21442,14.0625);
#4210=CIRCLE('',#21443,16.375);
#4211=CIRCLE('',#21444,14.0625);
#4212=CIRCLE('',#21445,16.375);
#4213=CIRCLE('',#21446,14.0625);
#4214=CIRCLE('',#21447,10.);
#4215=CIRCLE('',#21448,10.);
#4216=CIRCLE('',#21449,7.1875);
#4217=CIRCLE('',#21450,10.);
#4218=CIRCLE('',#21451,7.1875);
#4219=CIRCLE('',#21452,10.);
#4220=CIRCLE('',#21453,7.1875);
#4221=CIRCLE('',#21454,10.);
#4222=CIRCLE('',#21455,7.1875);
#4223=CIRCLE('',#21456,10.);
#4224=CIRCLE('',#21457,7.1875);
#4225=CIRCLE('',#21458,10.);
#4226=CIRCLE('',#21459,7.1875);
#4227=CIRCLE('',#21460,10.);
#4228=CIRCLE('',#21461,7.1875);
#4229=CIRCLE('',#21462,10.);
#4230=CIRCLE('',#21463,7.1875);
#4231=CIRCLE('',#21464,10.);
#4232=CIRCLE('',#21465,7.1875);
#4233=CIRCLE('',#21466,10.);
#4234=CIRCLE('',#21467,7.1875);
#4235=CIRCLE('',#21468,10.);
#4236=CIRCLE('',#21469,7.1875);
#4237=CIRCLE('',#21470,10.);
#4238=CIRCLE('',#21471,7.1875);
#4239=CIRCLE('',#21473,10.);
#4240=CIRCLE('',#21477,10.);
#4241=CIRCLE('',#21481,10.);
#4242=CIRCLE('',#21485,10.);
#4243=CIRCLE('',#21489,10.);
#4244=CIRCLE('',#21493,10.);
#4245=CIRCLE('',#21497,10.);
#4246=CIRCLE('',#21501,10.);
#4247=CIRCLE('',#21505,10.);
#4248=CIRCLE('',#21509,10.);
#4249=CIRCLE('',#21513,10.);
#4250=CIRCLE('',#21517,10.);
#4251=CIRCLE('',#21522,16.875);
#4252=CIRCLE('',#21524,16.875);
#4253=CIRCLE('',#21528,16.875);
#4254=CIRCLE('',#21530,16.875);
#4255=CIRCLE('',#21534,16.875);
#4256=CIRCLE('',#21536,16.875);
#4257=CIRCLE('',#21540,16.875);
#4258=CIRCLE('',#21542,16.875);
#4259=CIRCLE('',#21546,16.875);
#4260=CIRCLE('',#21548,16.875);
#4261=CIRCLE('',#21552,16.875);
#4262=CIRCLE('',#21554,16.875);
#4263=CIRCLE('',#21558,16.875);
#4264=CIRCLE('',#21560,16.875);
#4265=CIRCLE('',#21564,16.875);
#4266=CIRCLE('',#21566,16.875);
#4267=CIRCLE('',#21570,16.875);
#4268=CIRCLE('',#21572,16.875);
#4269=CIRCLE('',#21576,16.875);
#4270=CIRCLE('',#21578,16.875);
#4271=CIRCLE('',#21582,16.875);
#4272=CIRCLE('',#21584,16.875);
#4273=CIRCLE('',#21588,16.875);
#4274=CIRCLE('',#21590,16.875);
#4275=CIRCLE('',#21594,16.875);
#4276=CIRCLE('',#21596,16.875);
#4277=CIRCLE('',#21600,16.875);
#4278=CIRCLE('',#21602,16.875);
#4279=CIRCLE('',#21606,16.875);
#4280=CIRCLE('',#21608,16.875);
#4281=CIRCLE('',#21612,16.875);
#4282=CIRCLE('',#21614,16.875);
#4283=CIRCLE('',#21618,16.875);
#4284=CIRCLE('',#21620,16.875);
#4285=CIRCLE('',#21624,16.875);
#4286=CIRCLE('',#21626,16.875);
#4287=CIRCLE('',#21630,16.875);
#4288=CIRCLE('',#21632,16.875);
#4289=CIRCLE('',#21636,16.875);
#4290=CIRCLE('',#21638,16.875);
#4291=CIRCLE('',#21642,16.875);
#4292=CIRCLE('',#21644,16.875);
#4293=CIRCLE('',#21648,16.875);
#4294=CIRCLE('',#21650,16.875);
#4295=CIRCLE('',#21654,16.875);
#4296=CIRCLE('',#21656,16.875);
#4297=CIRCLE('',#21660,16.875);
#4298=CIRCLE('',#21662,16.875);
#4299=CIRCLE('',#21666,16.875);
#4300=CIRCLE('',#21668,16.875);
#4301=CIRCLE('',#21671,10.);
#4302=CIRCLE('',#21675,2.47573593128807);
#4303=CIRCLE('',#21676,0.3);
#4304=CIRCLE('',#21677,2.68786796564404);
#4305=CIRCLE('',#21678,2.68786796564404);
#4306=CIRCLE('',#21680,2.91213203435596);
#4307=CIRCLE('',#21681,2.91213203435596);
#4308=CIRCLE('',#21684,0.3);
#4309=CIRCLE('',#21685,3.);
#4310=CIRCLE('',#21686,3.);
#4311=CIRCLE('',#21688,3.);
#4312=CIRCLE('',#21689,3.);
#4313=CIRCLE('',#21691,0.3);
#4314=CIRCLE('',#21692,2.91213203435597);
#4315=CIRCLE('',#21693,2.91213203435597);
#4316=CIRCLE('',#21695,2.68786796564404);
#4317=CIRCLE('',#21696,2.68786796564404);
#4318=CIRCLE('',#21698,0.3);
#4319=CIRCLE('',#21699,2.47573593128807);
#4320=CIRCLE('',#21703,0.3);
#4321=CIRCLE('',#21704,0.3);
#4322=CIRCLE('',#21706,0.3);
#4323=CIRCLE('',#21707,2.2);
#4324=CIRCLE('',#21708,2.5);
#4325=CIRCLE('',#21710,0.3);
#4326=CIRCLE('',#21712,2.2);
#4327=CIRCLE('',#21713,2.5);
#4328=CIRCLE('',#21715,2.5);
#4329=CIRCLE('',#21718,1.575);
#4330=CIRCLE('',#21720,0.3);
#4331=CIRCLE('',#21721,0.3);
#4332=CIRCLE('',#21723,0.3);
#4333=CIRCLE('',#21724,2.2);
#4334=CIRCLE('',#21725,2.5);
#4335=CIRCLE('',#21727,0.3);
#4336=CIRCLE('',#21729,2.2);
#4337=CIRCLE('',#21732,1.575);
#4338=CIRCLE('',#21734,0.3);
#4339=CIRCLE('',#21735,1.275);
#4340=CIRCLE('',#21737,1.275);
#4341=CIRCLE('',#21738,1.275);
#4342=CIRCLE('',#21740,0.3);
#4343=CIRCLE('',#21744,0.867157287525381);
#4344=CIRCLE('',#21745,0.2);
#4345=CIRCLE('',#21746,1.00857864376269);
#4346=CIRCLE('',#21747,1.00857864376269);
#4347=CIRCLE('',#21749,1.19142135623731);
#4348=CIRCLE('',#21750,1.19142135623731);
#4349=CIRCLE('',#21753,0.2);
#4350=CIRCLE('',#21754,1.25);
#4351=CIRCLE('',#21755,1.25);
#4352=CIRCLE('',#21757,1.25);
#4353=CIRCLE('',#21758,1.25);
#4354=CIRCLE('',#21760,0.2);
#4355=CIRCLE('',#21761,1.19142135623731);
#4356=CIRCLE('',#21762,1.19142135623731);
#4357=CIRCLE('',#21764,1.00857864376269);
#4358=CIRCLE('',#21765,1.00857864376269);
#4359=CIRCLE('',#21767,0.2);
#4360=CIRCLE('',#21768,0.867157287525381);
#4361=CIRCLE('',#21772,0.599999999999996);
#4362=CIRCLE('',#21773,42.6);
#4363=CIRCLE('',#21774,0.599999999999996);
#4364=CIRCLE('',#21779,0.4);
#4365=CIRCLE('',#21782,0.4);
#4366=CIRCLE('',#21785,0.4);
#4367=CIRCLE('',#21786,0.4);
#4368=CIRCLE('',#21787,0.4);
#4369=CIRCLE('',#21790,0.4);
#4370=CIRCLE('',#21792,0.399999999999999);
#4371=CIRCLE('',#21793,0.399999999999999);
#4372=CIRCLE('',#21795,0.4);
#4373=CIRCLE('',#21796,0.4);
#4374=CIRCLE('',#21797,0.400000000000001);
#4375=CIRCLE('',#21800,0.400000000000001);
#4376=CIRCLE('',#21802,0.4);
#4377=CIRCLE('',#21803,0.4);
#4378=CIRCLE('',#21808,0.4);
#4379=CIRCLE('',#21810,0.4);
#4380=CIRCLE('',#21811,0.4);
#4381=CIRCLE('',#21816,21.3988897061572);
#4382=CIRCLE('',#21818,0.4);
#4383=CIRCLE('',#21821,0.4);
#4384=CIRCLE('',#21822,0.4);
#4385=CIRCLE('',#21824,0.4);
#4386=CIRCLE('',#21825,0.400000000000001);
#4387=CIRCLE('',#21827,0.4);
#4388=CIRCLE('',#21830,0.4);
#4389=CIRCLE('',#21832,0.4);
#4390=CIRCLE('',#21834,0.400000000000001);
#4391=CIRCLE('',#21836,0.4);
#4392=CIRCLE('',#21837,0.4);
#4393=CIRCLE('',#21841,0.4);
#4394=CIRCLE('',#21842,0.4);
#4395=CIRCLE('',#21843,0.4);
#4396=CIRCLE('',#21845,0.4);
#4397=CIRCLE('',#21847,0.4);
#4398=CIRCLE('',#21848,0.4);
#4399=CIRCLE('',#21854,21.3988897061572);
#4400=CIRCLE('',#21855,21.3988897061572);
#4401=CIRCLE('',#21857,0.4);
#4402=CIRCLE('',#21858,0.4);
#4403=CIRCLE('',#21860,0.400000000000001);
#4404=CIRCLE('',#21861,0.4);
#4405=CIRCLE('',#21863,0.4);
#4406=CIRCLE('',#21864,0.400000000000001);
#4407=CIRCLE('',#21866,0.400000000000001);
#4408=CIRCLE('',#21868,0.4);
#4409=CIRCLE('',#21871,0.4);
#4410=CIRCLE('',#21874,0.4);
#4411=CIRCLE('',#21875,0.4);
#4412=CIRCLE('',#21878,0.4);
#4413=CIRCLE('',#21880,0.400000000000001);
#4414=CIRCLE('',#21883,0.399999999999999);
#4415=CIRCLE('',#21884,0.4);
#4416=CIRCLE('',#21890,0.4);
#4417=CIRCLE('',#21891,0.4);
#4418=CIRCLE('',#21893,0.4);
#4419=CIRCLE('',#21894,21.4171572875254);
#4420=CIRCLE('',#21895,21.4171572875254);
#4421=CIRCLE('',#21896,21.1343145750508);
#4422=CIRCLE('',#21897,21.3988897061572);
#4423=CIRCLE('',#21898,21.1343145750508);
#4424=CIRCLE('',#21899,21.3988897061572);
#4425=CIRCLE('',#21900,21.1343145750508);
#4426=CIRCLE('',#21901,21.1343145750508);
#4427=CIRCLE('',#21903,0.4);
#4428=CIRCLE('',#21904,0.4);
#4429=CIRCLE('',#21905,10.7968626966597);
#4430=CIRCLE('',#21907,21.6828427124746);
#4431=CIRCLE('',#21908,21.6828427124746);
#4432=CIRCLE('',#21910,22.6);
#4433=CIRCLE('',#21911,0.4);
#4434=CIRCLE('',#21912,23.);
#4435=CIRCLE('',#21913,23.);
#4436=CIRCLE('',#21915,23.);
#4437=CIRCLE('',#21916,23.);
#4438=CIRCLE('',#21918,21.8);
#4439=CIRCLE('',#21920,0.4);
#4440=CIRCLE('',#21921,0.4);
#4441=CIRCLE('',#21923,0.4);
#4442=CIRCLE('',#21930,0.4);
#4443=CIRCLE('',#21932,0.4);
#4444=CIRCLE('',#21933,0.4);
#4445=CIRCLE('',#21935,0.4);
#4446=CIRCLE('',#21936,0.4);
#4447=CIRCLE('',#21938,0.399999999999999);
#4448=CIRCLE('',#21939,0.399999999999999);
#4449=CIRCLE('',#21941,0.400000000000001);
#4450=CIRCLE('',#21943,0.400000000000001);
#4451=CIRCLE('',#21946,0.4);
#4452=CIRCLE('',#21949,0.4);
#4453=CIRCLE('',#21952,0.4);
#4454=CIRCLE('',#21953,22.8828427124746);
#4455=CIRCLE('',#21954,22.8828427124746);
#4456=CIRCLE('',#21956,22.5171572875254);
#4457=CIRCLE('',#21957,22.5171572875254);
#4458=CIRCLE('',#21959,0.4);
#4459=CIRCLE('',#21960,21.8);
#4460=CIRCLE('',#21961,21.8);
#4461=CIRCLE('',#21964,10.4);
#4462=CIRCLE('',#21965,0.4);
#4463=CIRCLE('',#21967,0.4);
#4464=CIRCLE('',#21968,22.2343145750508);
#4465=CIRCLE('',#21970,7.45);
#4466=CIRCLE('',#21972,0.4);
#4467=CIRCLE('',#21975,0.400000000000001);
#4468=CIRCLE('',#21977,0.4);
#4469=CIRCLE('',#21980,0.400000000000001);
#4470=CIRCLE('',#21983,0.4);
#4471=CIRCLE('',#21986,0.4);
#4472=CIRCLE('',#21987,0.4);
#4473=CIRCLE('',#21991,0.4);
#4474=CIRCLE('',#21992,7.05);
#4475=CIRCLE('',#21993,7.05);
#4476=CIRCLE('',#21995,7.05);
#4477=CIRCLE('',#21996,7.05);
#4478=CIRCLE('',#21998,0.4);
#4479=CIRCLE('',#21999,7.45);
#4480=CIRCLE('',#22001,10.4);
#4481=CIRCLE('',#22037,0.8);
#4482=CIRCLE('',#22038,0.8);
#4483=CIRCLE('',#22043,9.5);
#4484=CIRCLE('',#22044,0.5);
#4485=CIRCLE('',#22045,9.);
#4486=CIRCLE('',#22046,9.);
#4487=CIRCLE('',#22048,9.);
#4488=CIRCLE('',#22049,9.);
#4489=CIRCLE('',#22051,0.5);
#4490=CIRCLE('',#22052,18.5);
#4491=CIRCLE('',#22053,0.5);
#4492=CIRCLE('',#22054,0.5);
#4493=CIRCLE('',#22055,18.5);
#4494=CIRCLE('',#22056,18.5);
#4495=CIRCLE('',#22057,0.5);
#4496=CIRCLE('',#22058,0.5);
#4497=CIRCLE('',#22059,18.5);
#4498=CIRCLE('',#22060,0.5);
#4499=CIRCLE('',#22061,0.5);
#4500=CIRCLE('',#22062,18.5);
#4501=CIRCLE('',#22063,0.5);
#4502=CIRCLE('',#22065,0.5);
#4503=CIRCLE('',#22066,9.5);
#4504=CIRCLE('',#22068,18.5);
#4505=CIRCLE('',#22069,18.5);
#4506=CIRCLE('',#22070,18.5);
#4507=CIRCLE('',#22071,0.5);
#4508=CIRCLE('',#22072,0.5);
#4509=CIRCLE('',#22073,18.5);
#4510=CIRCLE('',#22075,0.5);
#4511=CIRCLE('',#22076,0.5);
#4512=CIRCLE('',#22079,0.5);
#4513=CIRCLE('',#22080,0.5);
#4514=CIRCLE('',#22082,0.5);
#4515=CIRCLE('',#22083,0.5);
#4516=CIRCLE('',#22086,0.5);
#4517=CIRCLE('',#22087,0.5);
#4518=CIRCLE('',#22089,0.5);
#4519=CIRCLE('',#22090,0.5);
#4520=CIRCLE('',#22093,0.5);
#4521=CIRCLE('',#22094,0.5);
#4522=CIRCLE('',#22096,0.5);
#4523=CIRCLE('',#22097,20.6464466094067);
#4524=CIRCLE('',#22098,0.500000000405903);
#4525=CIRCLE('',#22099,20.2928932188135);
#4526=CIRCLE('',#22101,0.500000000000001);
#4527=CIRCLE('',#22102,0.5);
#4528=CIRCLE('',#22104,0.5);
#4529=CIRCLE('',#22105,0.5);
#4530=CIRCLE('',#22107,0.5);
#4531=CIRCLE('',#22108,0.5);
#4532=CIRCLE('',#22110,0.5);
#4533=CIRCLE('',#22112,0.500000000000001);
#4534=CIRCLE('',#22113,0.500000000000002);
#4535=CIRCLE('',#22115,20.8535533905933);
#4536=CIRCLE('',#22116,0.5);
#4537=CIRCLE('',#22119,0.499999999999995);
#4538=CIRCLE('',#22120,0.5);
#4539=CIRCLE('',#22122,0.5);
#4540=CIRCLE('',#22124,19.);
#4541=CIRCLE('',#22126,21.);
#4542=CIRCLE('',#22127,0.500000000000004);
#4543=CIRCLE('',#22129,21.);
#4544=CIRCLE('',#22130,21.);
#4545=CIRCLE('',#22131,21.);
#4546=CIRCLE('',#22132,21.);
#4547=CIRCLE('',#22133,21.);
#4548=CIRCLE('',#22134,21.);
#4549=CIRCLE('',#22135,21.);
#4550=CIRCLE('',#22136,21.);
#4551=CIRCLE('',#22137,21.);
#4552=CIRCLE('',#22138,21.);
#4553=CIRCLE('',#22140,0.5);
#4554=CIRCLE('',#22141,0.5);
#4555=CIRCLE('',#22143,0.499999999999999);
#4556=CIRCLE('',#22144,0.5);
#4557=CIRCLE('',#22146,0.499999999999999);
#4558=CIRCLE('',#22147,0.5);
#4559=CIRCLE('',#22148,0.5);
#4560=CIRCLE('',#22150,20.8535533905933);
#4561=CIRCLE('',#22151,0.5);
#4562=CIRCLE('',#22153,20.6464466094067);
#4563=CIRCLE('',#22155,20.2928932188135);
#4564=CIRCLE('',#22156,0.5);
#4565=CIRCLE('',#22158,20.5);
#4566=CIRCLE('',#22160,0.5);
#4567=CIRCLE('',#22161,19.);
#4568=CIRCLE('',#22163,0.5);
#4569=CIRCLE('',#22164,0.5);
#4570=CIRCLE('',#22165,0.5);
#4571=CIRCLE('',#22167,0.499999999999996);
#4572=CIRCLE('',#22168,20.8535533905933);
#4573=CIRCLE('',#22169,0.499999999999996);
#4574=CIRCLE('',#22171,0.5);
#4575=CIRCLE('',#22172,0.5);
#4576=CIRCLE('',#22174,0.499999999999998);
#4577=CIRCLE('',#22175,0.5);
#4578=CIRCLE('',#22177,0.499999999999999);
#4579=CIRCLE('',#22178,0.5);
#4580=CIRCLE('',#22179,0.5);
#4581=CIRCLE('',#22181,0.5);
#4582=CIRCLE('',#22185,0.5);
#4583=CIRCLE('',#22187,20.5);
#4584=CIRCLE('',#22189,19.);
#4585=CIRCLE('',#22190,0.5);
#4586=CIRCLE('',#22192,0.5);
#4587=CIRCLE('',#22194,0.500000000000001);
#4588=CIRCLE('',#22195,0.5);
#4589=CIRCLE('',#22199,0.5);
#4590=CIRCLE('',#22201,0.5);
#4591=CIRCLE('',#22202,0.5);
#4592=CIRCLE('',#22203,0.5);
#4593=CIRCLE('',#22205,0.499999999999995);
#4594=CIRCLE('',#22206,0.5);
#4595=CIRCLE('',#22208,20.5);
#4596=CIRCLE('',#22212,0.5);
#4597=CIRCLE('',#22214,19.);
#4598=CIRCLE('',#22216,0.5);
#4599=CIRCLE('',#22218,0.5);
#4600=CIRCLE('',#22219,0.5);
#4601=CIRCLE('',#22221,20.5);
#4602=CIRCLE('',#22223,0.5);
#4603=CIRCLE('',#22224,19.);
#4604=CIRCLE('',#22226,18.5);
#4605=CIRCLE('',#22228,18.5);
#4606=CIRCLE('',#22229,0.500000000000003);
#4607=CIRCLE('',#22232,18.5);
#4608=CIRCLE('',#22234,0.5);
#4609=CIRCLE('',#22237,18.5);
#4610=CIRCLE('',#22238,18.5);
#4611=CIRCLE('',#22239,18.5);
#4612=CIRCLE('',#22240,18.5);
#4613=CIRCLE('',#22241,18.5);
#4614=CIRCLE('',#22242,18.5);
#4615=CIRCLE('',#22243,18.5);
#4616=CIRCLE('',#22244,18.5);
#4617=CIRCLE('',#22245,18.5);
#4618=CIRCLE('',#22246,18.5);
#4619=CIRCLE('',#22249,19.);
#4620=CIRCLE('',#22253,19.);
#4621=CIRCLE('',#22257,0.500000000000004);
#4622=CIRCLE('',#22258,19.);
#4623=CIRCLE('',#22260,0.500000000000001);
#4624=CIRCLE('',#22261,0.5);
#4625=CIRCLE('',#22266,19.);
#4626=CIRCLE('',#22270,0.500000000000001);
#4627=CIRCLE('',#22272,0.5);
#4628=CIRCLE('',#22276,20.2928932188135);
#4629=CIRCLE('',#22277,20.6464466094067);
#4630=CIRCLE('',#22279,19.);
#4631=CIRCLE('',#22281,0.5);
#4632=CIRCLE('',#22283,0.5);
#4633=CIRCLE('',#22284,0.500000000000002);
#4634=CIRCLE('',#22286,0.500000000000003);
#4635=CIRCLE('',#22287,0.5);
#4636=CIRCLE('',#22293,20.5);
#4637=CIRCLE('',#22294,0.5);
#4638=CIRCLE('',#22300,19.);
#4639=CIRCLE('',#22303,20.8535533905933);
#4640=CIRCLE('',#22304,20.8535533905933);
#4641=CIRCLE('',#22305,0.5);
#4642=CIRCLE('',#22307,20.3464466094067);
#4643=CIRCLE('',#22308,20.3464466094067);
#4644=CIRCLE('',#22309,20.3464466094067);
#4645=CIRCLE('',#22310,20.3464466094067);
#4646=CIRCLE('',#22318,0.499999999999998);
#4647=CIRCLE('',#22321,18.5);
#4648=CIRCLE('',#22322,0.500000000000001);
#4649=CIRCLE('',#22323,19.);
#4650=CIRCLE('',#22325,0.500000000000001);
#4651=CIRCLE('',#22329,19.9928932188135);
#4652=CIRCLE('',#22332,19.9928932188135);
#4653=CIRCLE('',#22334,19.);
#4654=CIRCLE('',#22336,18.5);
#4655=CIRCLE('',#22339,19.9928932188135);
#4656=CIRCLE('',#22341,19.);
#4657=CIRCLE('',#22343,18.5);
#4658=CIRCLE('',#22346,19.9928932188135);
#4659=CIRCLE('',#22347,19.);
#4660=CIRCLE('',#22349,0.499999999999998);
#4661=CIRCLE('',#22350,18.5);
#4662=CIRCLE('',#22353,0.499999999999999);
#4663=CIRCLE('',#22355,0.500000000000001);
#4664=CIRCLE('',#22359,0.5);
#4665=CIRCLE('',#22360,0.5);
#4666=CIRCLE('',#22364,0.5);
#4667=CIRCLE('',#22365,0.5);
#4668=CIRCLE('',#22373,19.);
#4669=B_SPLINE_CURVE_WITH_KNOTS('',3,(#27826,#27827,#27828,#27829,#27830,
#27831,#27832,#27833,#27834,#27835,#27836,#27837,#27838,#27839,#27840,#27841,
#27842,#27843,#27844,#27845,#27846,#27847,#27848,#27849,#27850),
 .UNSPECIFIED.,.F.,.F.,(4,3,3,3,3,3,3,3,4),(-7.57991119318069,-6.9847970994778,
-6.48588302094367,-5.98696894240955,-5.48805486387542,-4.98914078534129,
-3.99131262827303,-2.99348447120477,-2.07135887395547),.UNSPECIFIED.);
#4670=B_SPLINE_CURVE_WITH_KNOTS('',3,(#27871,#27872,#27873,#27874,#27875,
#27876,#27877,#27878,#27879,#27880,#27881,#27882,#27883,#27884,#27885,#27886,
#27887,#27888,#27889,#27890,#27891,#27892),.UNSPECIFIED.,.F.,.F.,(4,3,3,
3,3,3,3,4),(0.,0.498914078534124,0.99782815706825,1.49674223560237,1.9956563141365,
2.99348447120475,3.991312628273,4.60707443244022),.UNSPECIFIED.);
#4671=B_SPLINE_CURVE_WITH_KNOTS('',3,(#27905,#27906,#27907,#27908,#27909,
#27910,#27911,#27912,#27913,#27914,#27915,#27916,#27917,#27918,#27919,#27920,
#27921,#27922,#27923,#27924,#27925,#27926,#27927,#27928,#27929,#27930,#27931,
#27932),.UNSPECIFIED.,.F.,.F.,(4,3,3,3,3,3,3,3,3,4),(-13.8630965003603,
-13.4706801204215,-12.9717660418873,-12.4728519633532,-11.9739378848191,
-10.9761097277508,-9.97828157068257,-8.98045341361432,-7.98262525654606,
-7.57991119318069),.UNSPECIFIED.);
#4672=B_SPLINE_CURVE_WITH_KNOTS('',3,(#27933,#27934,#27935,#27936,#27937,
#27938,#27939,#27940,#27941,#27942,#27943,#27944,#27945,#27946,#27947,#27948,
#27949,#27950,#27951,#27952,#27953,#27954,#27955,#27956,#27957,#27958,#27959,
#27960),.UNSPECIFIED.,.F.,.F.,(4,3,3,3,3,3,3,3,3,4),(4.60707443244022,4.98914078534126,
5.48805486387539,5.98696894240953,6.48588302094366,6.9847970994778,7.98262525654606,
8.98045341361433,9.9782815706826,10.8902597396198),.UNSPECIFIED.);
#4673=B_SPLINE_CURVE_WITH_KNOTS('',3,(#27965,#27966,#27967,#27968,#27969,
#27970,#27971,#27972,#27973,#27974,#27975,#27976,#27977,#27978,#27979,#27980,
#27981,#27982,#27983,#27984,#27985,#27986,#27987,#27988,#27989),
 .UNSPECIFIED.,.F.,.F.,(4,3,3,3,3,3,3,3,4),(-20.1462818075399,-19.2833612722667,
-18.4204407369935,-17.5575202017204,-16.6945996664472,-15.831679131174,
-14.9687585959009,-14.1058380606277,-13.8630965003603),.UNSPECIFIED.);
#4674=B_SPLINE_CURVE_WITH_KNOTS('',3,(#27990,#27991,#27992,#27993,#27994,
#27995,#27996,#27997,#27998,#27999,#28000,#28001,#28002,#28003,#28004,#28005,
#28006,#28007,#28008,#28009,#28010,#28011,#28012,#28013,#28014,#28015,#28016,
#28017,#28018,#28019,#28020),.UNSPECIFIED.,.F.,.F.,(4,3,3,3,3,3,3,3,3,3,
4),(10.8902597396198,10.9761097277509,11.9739378848191,12.4728519633533,
12.9717660418874,13.4706801204215,13.9695941989556,14.9674223560239,15.9652505130921,
16.9630786701604,17.1734450467994),.UNSPECIFIED.);
#4675=B_SPLINE_CURVE_WITH_KNOTS('',3,(#28025,#28026,#28027,#28028,#28029,
#28030,#28031,#28032,#28033,#28034,#28035,#28036,#28037,#28038,#28039,#28040,
#28041,#28042,#28043,#28044,#28045,#28046,#28047,#28048,#28049),
 .UNSPECIFIED.,.F.,.F.,(4,3,3,3,3,3,3,3,4),(-26.4294671147194,-25.9435320837747,
-24.9457039267064,-23.9478757696382,-22.9500476125699,-21.9522194555017,
-20.9543912984334,-20.4554772198993,-20.1462818075399),.UNSPECIFIED.);
#4676=B_SPLINE_CURVE_WITH_KNOTS('',3,(#28050,#28051,#28052,#28053,#28054,
#28055,#28056,#28057,#28058,#28059,#28060,#28061,#28062,#28063,#28064,#28065,
#28066,#28067,#28068,#28069,#28070,#28071,#28072,#28073,#28074,#28075,#28076,
#28077),.UNSPECIFIED.,.F.,.F.,(4,3,3,3,3,3,3,3,3,4),(17.1734450467994,17.9609068272287,
18.9587349842969,19.457649062831,19.9565631413651,20.4554772198993,20.9543912984334,
21.9522194555017,22.9500476125699,23.456630353979),.UNSPECIFIED.);
#4677=B_SPLINE_CURVE_WITH_KNOTS('',3,(#28082,#28083,#28084,#28085,#28086,
#28087,#28088,#28089,#28090,#28091,#28092,#28093,#28094,#28095,#28096,#28097,
#28098,#28099,#28100,#28101,#28102,#28103,#28104,#28105,#28106,#28107,#28108,
#28109),.UNSPECIFIED.,.F.,.F.,(4,3,3,3,3,3,3,3,3,4),(-32.712652421899,-31.9305010261842,
-30.932672869116,-29.9348447120477,-28.9370165549795,-27.9391883979112,
-27.4402743193771,-26.9413602408429,-26.4424461623088,-26.4294671147194),
 .UNSPECIFIED.);
#4678=B_SPLINE_CURVE_WITH_KNOTS('',3,(#28110,#28111,#28112,#28113,#28114,
#28115,#28116,#28117,#28118,#28119,#28120,#28121,#28122,#28123,#28124,#28125,
#28126,#28127,#28128,#28129,#28130,#28131,#28132,#28133,#28134,#28135,#28136,
#28137),.UNSPECIFIED.,.F.,.F.,(4,3,3,3,3,3,3,3,3,4),(23.456630353979,23.9478757696382,
24.9457039267064,25.9435320837747,26.4424461623088,26.941360240843,27.4402743193771,
27.9391883979112,28.9370165549795,29.7398156611586),.UNSPECIFIED.);
#4679=B_SPLINE_CURVE_WITH_KNOTS('',3,(#28142,#28143,#28144,#28145,#28146,
#28147,#28148,#28149,#28150,#28151,#28152,#28153,#28154,#28155,#28156,#28157,
#28158,#28159,#28160,#28161,#28162,#28163,#28164,#28165,#28166),
 .UNSPECIFIED.,.F.,.F.,(4,3,3,3,3,3,3,3,4),(-38.9958377290786,-38.1329171938055,
-37.2699966585323,-36.4070761232591,-35.544155587986,-34.6812350527128,
-33.8183145174396,-32.9553939821665,-32.712652421899),.UNSPECIFIED.);
#4680=B_SPLINE_CURVE_WITH_KNOTS('',3,(#28167,#28168,#28169,#28170,#28171,
#28172,#28173,#28174,#28175,#28176,#28177,#28178,#28179,#28180,#28181,#28182,
#28183,#28184,#28185,#28186,#28187,#28188,#28189,#28190,#28191,#28192,#28193,
#28194,#28195,#28196,#28197),.UNSPECIFIED.,.F.,.F.,(4,3,3,3,3,3,3,3,3,3,
4),(29.7398156611586,29.9348447120478,30.932672869116,31.9305010261843,
32.9283291832525,33.4272432617867,33.9261573403208,34.4250714188549,34.923985497389,
35.9218136544573,36.0230009683381),.UNSPECIFIED.);
#4681=B_SPLINE_CURVE_WITH_KNOTS('',3,(#28202,#28203,#28204,#28205,#28206,
#28207,#28208,#28209,#28210,#28211,#28212,#28213,#28214,#28215,#28216,#28217,
#28218,#28219,#28220,#28221,#28222,#28223,#28224,#28225,#28226,#28227,#28228,
#28229),.UNSPECIFIED.,.F.,.F.,(4,3,3,3,3,3,3,3,3,4),(-45.2790230362582,
-44.9022670680716,-43.9044389110033,-42.9066107539351,-41.9087825968668,
-41.4098685183327,-40.9109544397985,-40.4120403612644,-39.9131262827303,
-38.9958377290786),.UNSPECIFIED.);
#4682=B_SPLINE_CURVE_WITH_KNOTS('',3,(#28230,#28231,#28232,#28233,#28234,
#28235,#28236,#28237,#28238,#28239,#28240,#28241,#28242,#28243,#28244,#28245,
#28246,#28247,#28248,#28249,#28250,#28251,#28252,#28253,#28254,#28255,#28256,
#28257),.UNSPECIFIED.,.F.,.F.,(4,3,3,3,3,3,3,3,3,4),(36.0230009683381,36.9196418115256,
37.9174699685938,38.915298125662,39.9131262827303,40.4120403612644,40.9109544397986,
41.4098685183327,41.9087825968668,42.3061862755177),.UNSPECIFIED.);
#4683=B_SPLINE_CURVE_WITH_KNOTS('',3,(#28262,#28263,#28264,#28265,#28266,
#28267,#28268,#28269,#28270,#28271,#28272,#28273,#28274,#28275,#28276,#28277,
#28278,#28279,#28280,#28281,#28282,#28283,#28284,#28285,#28286,#28287,#28288,
#28289),.UNSPECIFIED.,.F.,.F.,(4,3,3,3,3,3,3,3,3,4),(-51.5622083434378,
-50.8892360104811,-49.8914078534129,-48.8935796963446,-48.3946656178105,
-47.8957515392764,-47.3968374607422,-46.8979233822081,-45.9000952251398,
-45.2790230362582),.UNSPECIFIED.);
#4684=B_SPLINE_CURVE_WITH_KNOTS('',3,(#28290,#28291,#28292,#28293,#28294,
#28295,#28296,#28297,#28298,#28299,#28300,#28301,#28302,#28303,#28304,#28305,
#28306,#28307,#28308,#28309,#28310,#28311,#28312,#28313,#28314),
 .UNSPECIFIED.,.F.,.F.,(4,3,3,3,3,3,3,3,4),(42.3061862755177,43.1691068107909,
44.0320273460641,44.8949478813372,45.7578684166104,46.6207889518835,47.4837094871567,
48.3466300224299,48.5893715826973),.UNSPECIFIED.);
#4685=B_SPLINE_CURVE_WITH_KNOTS('',3,(#28319,#28320,#28321,#28322,#28323,
#28324,#28325,#28326,#28327,#28328,#28329,#28330,#28331,#28332,#28333,#28334,
#28335,#28336,#28337,#28338,#28339,#28340,#28341,#28342,#28343,#28344,#28345,
#28346),.UNSPECIFIED.,.F.,.F.,(4,3,3,3,3,3,3,3,3,4),(-57.8453936506174,
-56.8762049528907,-55.8783767958224,-55.3794627172883,-54.8805486387542,
-54.38163456022,-53.8827204816859,-52.8848923246177,-51.8870641675494,-51.5622083434378),
 .UNSPECIFIED.);
#4686=B_SPLINE_CURVE_WITH_KNOTS('',3,(#28347,#28348,#28349,#28350,#28351,
#28352,#28353,#28354,#28355,#28356,#28357,#28358,#28359,#28360,#28361,#28362,
#28363,#28364,#28365,#28366,#28367,#28368,#28369,#28370,#28371),
 .UNSPECIFIED.,.F.,.F.,(4,3,3,3,3,3,3,3,4),(48.5893715826973,48.8935796963447,
49.8914078534129,50.8892360104811,51.8870641675494,52.8848923246177,53.8827204816859,
54.38163456022,54.8725568898769),.UNSPECIFIED.);
#4687=B_SPLINE_CURVE_WITH_KNOTS('',3,(#28376,#28377,#28378,#28379,#28380,
#28381,#28382,#28383,#28384,#28385,#28386,#28387,#28388,#28389,#28390,#28391,
#28392,#28393,#28394,#28395,#28396,#28397,#28398,#28399,#28400,#28401,#28402,
#28403,#28404,#28405,#28406),.UNSPECIFIED.,.F.,.F.,(4,3,3,3,3,3,3,3,3,3,
4),(-64.128578957797,-63.8610020523685,-62.8631738953002,-62.3642598167661,
-61.865345738232,-61.3664316596978,-60.8675175811637,-59.8696894240954,
-58.8718612670272,-57.8740331099589,-57.8453936506174),.UNSPECIFIED.);
#4688=B_SPLINE_CURVE_WITH_KNOTS('',3,(#28407,#28408,#28409,#28410,#28411,
#28412,#28413,#28414,#28415,#28416,#28417,#28418,#28419,#28420,#28421,#28422,
#28423,#28424,#28425,#28426,#28427,#28428,#28429,#28430,#28431,#28432,#28433,
#28434),.UNSPECIFIED.,.F.,.F.,(4,3,3,3,3,3,3,3,3,4),(54.8725568898769,54.8805486387541,
55.3794627172883,55.8783767958224,56.8762049528906,57.8740331099589,58.8718612670272,
59.8696894240955,60.8675175811637,61.1557421970565),.UNSPECIFIED.);
#4689=B_SPLINE_CURVE_WITH_KNOTS('',3,(#28439,#28440,#28441,#28442,#28443,
#28444,#28445,#28446,#28447,#28448,#28449,#28450,#28451,#28452,#28453,#28454,
#28455,#28456,#28457,#28458,#28459,#28460,#28461,#28462,#28463),
 .UNSPECIFIED.,.F.,.F.,(4,3,3,3,3,3,3,3,4),(-70.4117642649766,-69.5488437297034,
-68.6859231944302,-67.823002659157,-66.9600821238839,-66.0971615886107,
-65.2342410533375,-64.3713205180643,-64.128578957797),.UNSPECIFIED.);
#4690=B_SPLINE_CURVE_WITH_KNOTS('',3,(#28464,#28465,#28466,#28467,#28468,
#28469,#28470,#28471,#28472,#28473,#28474,#28475,#28476,#28477,#28478,#28479,
#28480,#28481,#28482,#28483,#28484,#28485,#28486,#28487,#28488),
 .UNSPECIFIED.,.F.,.F.,(4,3,3,3,3,3,3,3,4),(61.1557421970565,62.0186627323297,
62.8815832676029,63.7445038028761,64.6074243381492,65.4703448734224,66.3332654086956,
67.1961859439688,67.4389275042361),.UNSPECIFIED.);
#4691=B_SPLINE_CURVE_WITH_KNOTS('',3,(#28493,#28494,#28495,#28496,#28497,
#28498,#28499,#28500,#28501,#28502,#28503,#28504,#28505,#28506,#28507,#28508,
#28509,#28510,#28511,#28512,#28513,#28514,#28515,#28516,#28517,#28518,#28519,
#28520),.UNSPECIFIED.,.F.,.F.,(4,3,3,3,3,3,3,3,3,4),(-76.6949495721561,
-76.3338540157217,-75.8349399371876,-75.3360258586534,-74.8371117801193,
-73.8392836230511,-72.8414554659828,-71.8436273089145,-70.8457991518463,
-70.4117642649766),.UNSPECIFIED.);
#4692=B_SPLINE_CURVE_WITH_KNOTS('',3,(#28521,#28522,#28523,#28524,#28525,
#28526,#28527,#28528,#28529,#28530,#28531,#28532,#28533,#28534,#28535,#28536,
#28537,#28538,#28539,#28540,#28541,#28542,#28543,#28544,#28545,#28546,#28547,
#28548),.UNSPECIFIED.,.F.,.F.,(4,3,3,3,3,3,3,3,3,4),(67.4389275042361,67.8523146806415,
68.3512287591757,68.8501428377098,69.3490569162439,69.847970994778,70.8457991518463,
71.8436273089145,72.8414554659828,73.7221128114157),.UNSPECIFIED.);
#4693=B_SPLINE_CURVE_WITH_KNOTS('',3,(#28553,#28554,#28555,#28556,#28557,
#28558,#28559,#28560,#28561,#28562,#28563,#28564,#28565,#28566,#28567,#28568,
#28569,#28570,#28571,#28572,#28573,#28574,#28575,#28576,#28577),
 .UNSPECIFIED.,.F.,.F.,(4,3,3,3,3,3,3,3,4),(-82.9781348793357,-82.1152143440626,
-81.2522938087894,-80.3893732735162,-79.526452738243,-78.6635322029699,
-77.8006116676967,-76.9376911324235,-76.6949495721561),.UNSPECIFIED.);
#4694=B_SPLINE_CURVE_WITH_KNOTS('',3,(#28578,#28579,#28580,#28581,#28582,
#28583,#28584,#28585,#28586,#28587,#28588,#28589,#28590,#28591,#28592,#28593,
#28594,#28595,#28596,#28597,#28598,#28599,#28600,#28601,#28602,#28603,#28604,
#28605,#28606,#28607,#28608),.UNSPECIFIED.,.F.,.F.,(4,3,3,3,3,3,3,3,3,3,
4),(73.7221128114157,73.839283623051,74.8371117801193,75.3360258586534,
75.8349399371876,76.3338540157217,76.8327680942558,77.8305962513241,78.8284244083924,
79.8262525654606,80.0052981185953),.UNSPECIFIED.);
#4695=B_SPLINE_CURVE_WITH_KNOTS('',3,(#28613,#28614,#28615,#28616,#28617,
#28618,#28619,#28620,#28621,#28622,#28623,#28624,#28625,#28626,#28627,#28628,
#28629,#28630,#28631,#28632,#28633,#28634,#28635,#28636,#28637),
 .UNSPECIFIED.,.F.,.F.,(4,3,3,3,3,3,3,3,4),(-89.2613201865154,-88.8067059790749,
-87.8088778220067,-86.8110496649384,-85.8132215078701,-84.8153933508019,
-83.8175651937336,-83.3186511151995,-82.9781348793357),.UNSPECIFIED.);
#4696=B_SPLINE_CURVE_WITH_KNOTS('',3,(#28638,#28639,#28640,#28641,#28642,
#28643,#28644,#28645,#28646,#28647,#28648,#28649,#28650,#28651,#28652,#28653,
#28654,#28655,#28656,#28657,#28658,#28659,#28660,#28661,#28662,#28663,#28664,
#28665),.UNSPECIFIED.,.F.,.F.,(4,3,3,3,3,3,3,3,3,4),(80.0052981185953,80.8240807225289,
81.8219088795971,82.3208229581313,82.8197370366654,83.3186511151995,83.8175651937337,
84.8153933508019,85.8132215078702,86.2884834257749),.UNSPECIFIED.);
#4697=B_SPLINE_CURVE_WITH_KNOTS('',3,(#28670,#28671,#28672,#28673,#28674,
#28675,#28676,#28677,#28678,#28679,#28680,#28681,#28682,#28683,#28684,#28685,
#28686,#28687,#28688,#28689,#28690,#28691,#28692,#28693,#28694),
 .UNSPECIFIED.,.F.,.F.,(4,3,3,3,3,3,3,3,4),(-95.544505493695,-94.6815849584218,
-93.8186644231486,-92.9557438878754,-92.0928233526023,-91.2299028173291,
-90.3669822820559,-89.5040617467827,-89.2613201865154),.UNSPECIFIED.);
#4698=B_SPLINE_CURVE_WITH_KNOTS('',3,(#28695,#28696,#28697,#28698,#28699,
#28700,#28701,#28702,#28703,#28704,#28705,#28706,#28707,#28708,#28709,#28710,
#28711,#28712,#28713,#28714,#28715,#28716,#28717,#28718,#28719,#28720,#28721,
#28722),.UNSPECIFIED.,.F.,.F.,(4,3,3,3,3,3,3,3,3,4),(86.2884834257749,86.8110496649385,
87.8088778220067,88.8067059790749,89.3056200576091,89.8045341361432,90.3034482146773,
90.8023622932114,91.8001904502797,92.5716687329545),.UNSPECIFIED.);
#4699=B_SPLINE_CURVE_WITH_KNOTS('',3,(#28727,#28728,#28729,#28730,#28731,
#28732,#28733,#28734,#28735,#28736,#28737,#28738,#28739,#28740,#28741,#28742,
#28743,#28744,#28745,#28746,#28747,#28748,#28749,#28750,#28751,#28752,#28753,
#28754,#28755,#28756,#28757),.UNSPECIFIED.,.F.,.F.,(4,3,3,3,3,3,3,3,3,3,
4),(-101.827690800875,-101.778472020962,-100.780643863894,-99.7828157068258,
-98.7849875497575,-97.7871593926892,-97.2882453141551,-96.789331235621,
-96.2904171570868,-95.7915030785527,-95.544505493695),.UNSPECIFIED.);
#4700=B_SPLINE_CURVE_WITH_KNOTS('',3,(#28758,#28759,#28760,#28761,#28762,
#28763,#28764,#28765,#28766,#28767,#28768,#28769,#28770,#28771,#28772,#28773,
#28774,#28775,#28776,#28777,#28778,#28779,#28780,#28781,#28782,#28783,#28784,
#28785,#28786,#28787,#28788),.UNSPECIFIED.,.F.,.F.,(4,3,3,3,3,3,3,3,3,3,
4),(92.5716687329545,92.798018607348,93.7958467644162,94.7936749214845,
95.7915030785527,96.2904171570868,96.7893312356209,97.2882453141551,97.7871593926892,
98.7849875497574,98.8548540401341),.UNSPECIFIED.);
#4701=B_SPLINE_CURVE_WITH_KNOTS('',3,(#28793,#28794,#28795,#28796,#28797,
#28798,#28799,#28800,#28801,#28802,#28803,#28804,#28805,#28806,#28807,#28808,
#28809,#28810,#28811,#28812,#28813,#28814,#28815,#28816,#28817,#28818,#28819,
#28820),.UNSPECIFIED.,.F.,.F.,(4,3,3,3,3,3,3,3,3,4),(-108.110876108054,
-107.765440963372,-106.767612806304,-105.769784649235,-104.771956492167,
-104.273042413633,-103.774128335099,-103.275214256565,-102.776300178031,
-101.827690800875),.UNSPECIFIED.);
#4702=B_SPLINE_CURVE_WITH_KNOTS('',3,(#28821,#28822,#28823,#28824,#28825,
#28826,#28827,#28828,#28829,#28830,#28831,#28832,#28833,#28834,#28835,#28836,
#28837,#28838,#28839,#28840,#28841,#28842,#28843,#28844,#28845,#28846,#28847,
#28848),.UNSPECIFIED.,.F.,.F.,(4,3,3,3,3,3,3,3,3,4),(98.8548540401341,99.7828157068257,
100.780643863894,101.778472020962,102.776300178031,103.275214256565,103.774128335099,
104.273042413633,104.771956492167,105.138039347314),.UNSPECIFIED.);
#4703=B_SPLINE_CURVE_WITH_KNOTS('',3,(#28853,#28854,#28855,#28856,#28857,
#28858,#28859,#28860,#28861,#28862,#28863,#28864,#28865,#28866,#28867,#28868,
#28869,#28870,#28871,#28872,#28873,#28874,#28875,#28876,#28877,#28878,#28879,
#28880),.UNSPECIFIED.,.F.,.F.,(4,3,3,3,3,3,3,3,3,4),(-114.394061415234,
-113.752409905781,-112.754581748713,-111.756753591645,-111.257839513111,
-110.758925434577,-110.260011356042,-109.761097277508,-108.76326912044,
-108.110876108054),.UNSPECIFIED.);
#4704=B_SPLINE_CURVE_WITH_KNOTS('',3,(#28881,#28882,#28883,#28884,#28885,
#28886,#28887,#28888,#28889,#28890,#28891,#28892,#28893,#28894,#28895,#28896,
#28897,#28898,#28899,#28900,#28901,#28902,#28903,#28904,#28905),
 .UNSPECIFIED.,.F.,.F.,(4,3,3,3,3,3,3,3,4),(105.138039347314,106.000959882587,
106.86388041786,107.726800953133,108.589721488406,109.45264202368,110.315562558953,
111.178483094226,111.421224654493),.UNSPECIFIED.);
#4705=B_SPLINE_CURVE_WITH_KNOTS('',3,(#28910,#28911,#28912,#28913,#28914,
#28915,#28916,#28917,#28918,#28919,#28920,#28921,#28922,#28923,#28924,#28925,
#28926,#28927,#28928,#28929,#28930,#28931,#28932,#28933,#28934,#28935,#28936,
#28937),.UNSPECIFIED.,.F.,.F.,(4,3,3,3,3,3,3,3,3,4),(-120.677246722413,
-119.739378848191,-118.741550691123,-118.242636612589,-117.743722534054,
-117.24480845552,-116.745894376986,-115.748066219918,-114.75023806285,-114.394061415234),
 .UNSPECIFIED.);
#4706=B_SPLINE_CURVE_WITH_KNOTS('',3,(#28938,#28939,#28940,#28941,#28942,
#28943,#28944,#28945,#28946,#28947,#28948,#28949,#28950,#28951,#28952,#28953,
#28954,#28955,#28956,#28957,#28958,#28959,#28960,#28961,#28962),
 .UNSPECIFIED.,.F.,.F.,(4,3,3,3,3,3,3,3,4),(111.421224654493,111.756753591645,
112.754581748713,113.752409905781,114.75023806285,115.748066219918,116.745894376986,
117.24480845552,117.704409961673),.UNSPECIFIED.);
#4707=B_SPLINE_CURVE_WITH_KNOTS('',3,(#28967,#28968,#28969,#28970,#28971,
#28972,#28973,#28974,#28975,#28976,#28977,#28978,#28979,#28980,#28981,#28982,
#28983,#28984,#28985,#28986,#28987,#28988,#28989,#28990,#28991,#28992,#28993,
#28994,#28995,#28996,#28997),.UNSPECIFIED.,.F.,.F.,(4,3,3,3,3,3,3,3,3,3,
4),(-126.960432029593,-126.724175947669,-125.7263477906,-125.227433712066,
-124.728519633532,-124.229605554998,-123.730691476464,-122.732863319396,
-121.735035162327,-120.737207005259,-120.677246722413),.UNSPECIFIED.);
#4708=B_SPLINE_CURVE_WITH_KNOTS('',3,(#28998,#28999,#29000,#29001,#29002,
#29003,#29004,#29005,#29006,#29007,#29008,#29009,#29010,#29011,#29012,#29013,
#29014,#29015,#29016,#29017,#29018,#29019,#29020,#29021,#29022,#29023,#29024,
#29025),.UNSPECIFIED.,.F.,.F.,(4,3,3,3,3,3,3,3,3,4),(117.704409961673,117.743722534054,
118.242636612588,118.741550691123,119.739378848191,120.737207005259,121.735035162327,
122.732863319396,123.730691476464,123.987595268852),.UNSPECIFIED.);
#4709=B_SPLINE_CURVE_WITH_KNOTS('',3,(#29030,#29031,#29032,#29033,#29034,
#29035,#29036,#29037,#29038,#29039,#29040,#29041,#29042,#29043,#29044,#29045,
#29046,#29047,#29048,#29049,#29050,#29051,#29052,#29053,#29054),
 .UNSPECIFIED.,.F.,.F.,(4,3,3,3,3,3,3,3,4),(-133.243617336773,-132.380696801499,
-131.517776266226,-130.654855730953,-129.79193519568,-128.929014660407,
-128.066094125133,-127.20317358986,-126.960432029593),.UNSPECIFIED.);
#4710=B_SPLINE_CURVE_WITH_KNOTS('',3,(#29055,#29056,#29057,#29058,#29059,
#29060,#29061,#29062,#29063,#29064,#29065,#29066,#29067,#29068,#29069,#29070,
#29071,#29072,#29073,#29074,#29075,#29076,#29077,#29078,#29079),
 .UNSPECIFIED.,.F.,.F.,(4,3,3,3,3,3,3,3,4),(123.987595268852,124.850515804126,
125.713436339399,126.576356874672,127.439277409945,128.302197945218,129.165118480492,
130.028039015765,130.270780576032),.UNSPECIFIED.);
#4711=B_SPLINE_CURVE_WITH_KNOTS('',3,(#29084,#29085,#29086,#29087,#29088,
#29089,#29090,#29091,#29092,#29093,#29094,#29095,#29096,#29097,#29098,#29099,
#29100,#29101,#29102,#29103,#29104,#29105,#29106,#29107,#29108),
 .UNSPECIFIED.,.F.,.F.,(4,3,3,3,3,3,3,3,4),(-139.526802643952,-138.663882108679,
-137.800961573406,-136.938041038132,-136.075120502859,-135.212199967586,
-134.349279432313,-133.48635889704,-133.243617336773),.UNSPECIFIED.);
#4712=B_SPLINE_CURVE_WITH_KNOTS('',3,(#29109,#29110,#29111,#29112,#29113,
#29114,#29115,#29116,#29117,#29118,#29119,#29120,#29121,#29122,#29123,#29124,
#29125,#29126,#29127,#29128,#29129,#29130,#29131,#29132,#29133,#29134,#29135,
#29136),.UNSPECIFIED.,.F.,.F.,(4,3,3,3,3,3,3,3,3,4),(130.270780576032,130.715488575942,
131.214402654476,131.71331673301,132.212230811544,132.711144890078,133.708973047147,
134.706801204215,135.704629361283,136.553965883212),.UNSPECIFIED.);
#4713=B_SPLINE_CURVE_WITH_KNOTS('',3,(#29141,#29142,#29143,#29144,#29145,
#29146,#29147,#29148,#29149,#29150,#29151,#29152,#29153,#29154,#29155,#29156,
#29157,#29158,#29159,#29160,#29161,#29162,#29163,#29164,#29165),
 .UNSPECIFIED.,.F.,.F.,(4,3,3,3,3,3,3,3,4),(-145.809987951132,-144.947067415858,
-144.084146880585,-143.221226345312,-142.358305810039,-141.495385274766,
-140.632464739492,-139.769544204219,-139.526802643952),.UNSPECIFIED.);
#4714=B_SPLINE_CURVE_WITH_KNOTS('',3,(#29166,#29167,#29168,#29169,#29170,
#29171,#29172,#29173,#29174,#29175,#29176,#29177,#29178,#29179,#29180,#29181,
#29182,#29183,#29184,#29185,#29186,#29187,#29188,#29189,#29190,#29191,#29192,
#29193,#29194,#29195,#29196),.UNSPECIFIED.,.F.,.F.,(4,3,3,3,3,3,3,3,3,3,
4),(136.553965883212,136.702457518351,137.70028567542,138.199199753954,
138.698113832488,139.197027911022,139.695941989556,140.693770146624,141.691598303693,
142.689426460761,142.837151190391),.UNSPECIFIED.);
#4715=B_SPLINE_CURVE_WITH_KNOTS('',3,(#29201,#29202,#29203,#29204,#29205,
#29206,#29207,#29208,#29209,#29210,#29211,#29212,#29213,#29214,#29215,#29216,
#29217,#29218,#29219,#29220,#29221,#29222,#29223,#29224,#29225),
 .UNSPECIFIED.,.F.,.F.,(4,3,3,3,3,3,3,3,4),(-152.093173258311,-151.669879874375,
-150.672051717307,-149.674223560239,-148.67639540317,-147.678567246102,
-146.680739089034,-146.1818250105,-145.809987951132),.UNSPECIFIED.);
#4716=B_SPLINE_CURVE_WITH_KNOTS('',3,(#29226,#29227,#29228,#29229,#29230,
#29231,#29232,#29233,#29234,#29235,#29236,#29237,#29238,#29239,#29240,#29241,
#29242,#29243,#29244,#29245,#29246,#29247,#29248,#29249,#29250,#29251,#29252,
#29253),.UNSPECIFIED.,.F.,.F.,(4,3,3,3,3,3,3,3,3,4),(142.837151190391,143.687254617829,
144.685082774897,145.183996853431,145.682910931966,146.1818250105,146.680739089034,
147.678567246102,148.67639540317,149.120336497571),.UNSPECIFIED.);
#4717=B_SPLINE_CURVE_WITH_KNOTS('',3,(#29258,#29259,#29260,#29261,#29262,
#29263,#29264,#29265,#29266,#29267,#29268,#29269,#29270,#29271,#29272,#29273,
#29274,#29275,#29276,#29277,#29278,#29279,#29280,#29281,#29282),
 .UNSPECIFIED.,.F.,.F.,(4,3,3,3,3,3,3,3,4),(-158.376358565491,-157.513438030218,
-156.650517494944,-155.787596959671,-154.924676424398,-154.061755889125,
-153.198835353852,-152.335914818578,-152.093173258311),.UNSPECIFIED.);
#4718=B_SPLINE_CURVE_WITH_KNOTS('',3,(#29283,#29284,#29285,#29286,#29287,
#29288,#29289,#29290,#29291,#29292,#29293,#29294,#29295,#29296,#29297,#29298,
#29299,#29300,#29301,#29302,#29303,#29304,#29305,#29306,#29307,#29308,#29309,
#29310),.UNSPECIFIED.,.F.,.F.,(4,3,3,3,3,3,3,3,3,4),(149.120336497571,149.674223560239,
150.672051717307,151.669879874375,152.168793952909,152.667708031443,153.166622109978,
153.665536188512,154.66336434558,155.40352180475),.UNSPECIFIED.);
#4719=B_SPLINE_CURVE_WITH_KNOTS('',3,(#29315,#29316,#29317,#29318,#29319,
#29320,#29321,#29322,#29323,#29324,#29325,#29326,#29327,#29328,#29329,#29330,
#29331,#29332,#29333,#29334,#29335,#29336,#29337,#29338,#29339,#29340,#29341,
#29342,#29343,#29344,#29345),.UNSPECIFIED.,.F.,.F.,(4,3,3,3,3,3,3,3,3,3,
4),(-164.65954387267,-164.641645916262,-163.643817759194,-162.645989602126,
-161.648161445058,-160.650333287989,-160.151419209455,-159.652505130921,
-159.153591052387,-158.654676973853,-158.376358565491),.UNSPECIFIED.);
#4720=B_SPLINE_CURVE_WITH_KNOTS('',3,(#29346,#29347,#29348,#29349,#29350,
#29351,#29352,#29353,#29354,#29355,#29356,#29357,#29358,#29359,#29360,#29361,
#29362,#29363,#29364,#29365,#29366,#29367,#29368,#29369,#29370,#29371,#29372,
#29373,#29374,#29375,#29376),.UNSPECIFIED.,.F.,.F.,(4,3,3,3,3,3,3,3,3,3,
4),(155.40352180475,155.661192502648,156.659020659716,157.656848816785,
158.654676973853,159.153591052387,159.652505130921,160.151419209455,160.650333287989,
161.648161445058,161.68670711193),.UNSPECIFIED.);
#4721=B_SPLINE_CURVE_WITH_KNOTS('',3,(#29381,#29382,#29383,#29384,#29385,
#29386,#29387,#29388,#29389,#29390,#29391,#29392,#29393,#29394,#29395,#29396,
#29397,#29398,#29399,#29400,#29401,#29402,#29403,#29404,#29405,#29406,#29407,
#29408),.UNSPECIFIED.,.F.,.F.,(4,3,3,3,3,3,3,3,3,4),(-170.94272917985,-170.628614858672,
-169.630786701604,-168.632958544536,-167.635130387467,-167.136216308933,
-166.637302230399,-166.138388151865,-165.639474073331,-164.65954387267),
 .UNSPECIFIED.);
#4722=B_SPLINE_CURVE_WITH_KNOTS('',3,(#29409,#29410,#29411,#29412,#29413,
#29414,#29415,#29416,#29417,#29418,#29419,#29420,#29421,#29422,#29423,#29424,
#29425,#29426,#29427,#29428,#29429,#29430,#29431,#29432,#29433,#29434,#29435,
#29436),.UNSPECIFIED.,.F.,.F.,(4,3,3,3,3,3,3,3,3,4),(161.68670711193,162.645989602126,
163.643817759194,164.641645916263,165.639474073331,166.138388151865,166.637302230399,
167.136216308933,167.635130387467,167.969892419109),.UNSPECIFIED.);
#4723=B_SPLINE_CURVE_WITH_KNOTS('',3,(#29441,#29442,#29443,#29444,#29445,
#29446,#29447,#29448,#29449,#29450,#29451,#29452,#29453,#29454,#29455,#29456,
#29457,#29458,#29459,#29460,#29461,#29462,#29463,#29464,#29465,#29466,#29467,
#29468),.UNSPECIFIED.,.F.,.F.,(4,3,3,3,3,3,3,3,3,4),(-177.225914487029,
-176.615583801082,-175.617755644013,-174.619927486945,-174.121013408411,
-173.622099329877,-173.123185251343,-172.624271172809,-171.62644301574,
-170.94272917985),.UNSPECIFIED.);
#4724=B_SPLINE_CURVE_WITH_KNOTS('',3,(#29469,#29470,#29471,#29472,#29473,
#29474,#29475,#29476,#29477,#29478,#29479,#29480,#29481,#29482,#29483,#29484,
#29485,#29486,#29487,#29488,#29489,#29490,#29491,#29492,#29493),
 .UNSPECIFIED.,.F.,.F.,(4,3,3,3,3,3,3,3,4),(167.969892419109,168.832812954383,
169.695733489656,170.558654024929,171.421574560202,172.284495095475,173.147415630748,
174.010336166022,174.253077726289),.UNSPECIFIED.);
#4725=B_SPLINE_CURVE_WITH_KNOTS('',3,(#29498,#29499,#29500,#29501,#29502,
#29503,#29504,#29505,#29506,#29507,#29508,#29509,#29510,#29511,#29512,#29513,
#29514,#29515,#29516,#29517,#29518,#29519,#29520,#29521,#29522,#29523,#29524,
#29525),.UNSPECIFIED.,.F.,.F.,(4,3,3,3,3,3,3,3,3,4),(-183.509099794209,
-182.602552743491,-181.604724586423,-181.105810507889,-180.606896429355,
-180.10798235082,-179.609068272286,-178.611240115218,-177.61341195815,-177.225914487029),
 .UNSPECIFIED.);
#4726=B_SPLINE_CURVE_WITH_KNOTS('',3,(#29526,#29527,#29528,#29529,#29530,
#29531,#29532,#29533,#29534,#29535,#29536,#29537,#29538,#29539,#29540,#29541,
#29542,#29543,#29544,#29545,#29546,#29547,#29548,#29549,#29550),
 .UNSPECIFIED.,.F.,.F.,(4,3,3,3,3,3,3,3,4),(174.253077726289,174.619927486945,
175.617755644013,176.615583801082,177.61341195815,178.611240115218,179.609068272286,
180.107982350821,180.536263033469),.UNSPECIFIED.);
#4727=B_SPLINE_CURVE_WITH_KNOTS('',3,(#29555,#29556,#29557,#29558,#29559,
#29560,#29561,#29562,#29563,#29564,#29565,#29566,#29567,#29568,#29569,#29570,
#29571,#29572,#29573,#29574,#29575,#29576,#29577,#29578,#29579,#29580,#29581,
#29582,#29583,#29584,#29585),.UNSPECIFIED.,.F.,.F.,(4,3,3,3,3,3,3,3,3,3,
4),(-189.792285101389,-189.587349842969,-188.589521685901,-188.090607607367,
-187.591693528832,-187.092779450298,-186.593865371764,-185.596037214696,
-184.598209057628,-183.600380900559,-183.509099794209),.UNSPECIFIED.);
#4728=B_SPLINE_CURVE_WITH_KNOTS('',3,(#29586,#29587,#29588,#29589,#29590,
#29591,#29592,#29593,#29594,#29595,#29596,#29597,#29598,#29599,#29600,#29601,
#29602,#29603,#29604,#29605,#29606,#29607,#29608,#29609,#29610),
 .UNSPECIFIED.,.F.,.F.,(4,3,3,3,3,3,3,3,4),(180.536263033469,181.399183568742,
182.262104104015,183.125024639288,183.987945174561,184.850865709834,185.713786245107,
186.576706780381,186.819448340648),.UNSPECIFIED.);
#4729=B_SPLINE_CURVE_WITH_KNOTS('',3,(#29615,#29616,#29617,#29618,#29619,
#29620,#29621,#29622,#29623,#29624,#29625,#29626,#29627,#29628,#29629,#29630,
#29631,#29632,#29633,#29634,#29635,#29636,#29637,#29638,#29639),
 .UNSPECIFIED.,.F.,.F.,(4,3,3,3,3,3,3,3,4),(-196.075470408568,-195.212549873295,
-194.349629338022,-193.486708802749,-192.623788267476,-191.760867732202,
-190.897947196929,-190.035026661656,-189.792285101389),.UNSPECIFIED.);
#4730=B_SPLINE_CURVE_WITH_KNOTS('',3,(#29640,#29641,#29642,#29643,#29644,
#29645,#29646,#29647,#29648,#29649,#29650,#29651,#29652,#29653,#29654,#29655,
#29656,#29657,#29658,#29659,#29660,#29661,#29662,#29663,#29664),
 .UNSPECIFIED.,.F.,.F.,(4,3,3,3,3,3,3,3,4),(186.819448340648,187.682368875921,
188.545289411195,189.408209946468,190.271130481741,191.134051017014,191.996971552287,
192.859892087561,193.102633647828),.UNSPECIFIED.);
#4731=B_SPLINE_CURVE_WITH_KNOTS('',3,(#29669,#29670,#29671,#29672,#29673,
#29674,#29675,#29676,#29677,#29678,#29679,#29680,#29681,#29682,#29683,#29684,
#29685,#29686,#29687,#29688,#29689,#29690,#29691,#29692,#29693),
 .UNSPECIFIED.,.F.,.F.,(4,3,3,3,3,3,3,3,4),(-202.358655715748,-202.060201806322,
-201.561287727788,-200.56345957072,-199.565631413651,-198.567803256583,
-197.569975099515,-196.572146942447,-196.075470408568),.UNSPECIFIED.);
#4732=B_SPLINE_CURVE_WITH_KNOTS('',3,(#29694,#29695,#29696,#29697,#29698,
#29699,#29700,#29701,#29702,#29703,#29704,#29705,#29706,#29707,#29708,#29709,
#29710,#29711,#29712,#29713,#29714,#29715,#29716,#29717,#29718,#29719,#29720,
#29721),.UNSPECIFIED.,.F.,.F.,(4,3,3,3,3,3,3,3,3,4),(193.102633647828,193.578662471242,
194.077576549776,194.57649062831,195.075404706844,195.574318785378,196.572146942447,
197.569975099515,198.567803256583,199.385818955007),.UNSPECIFIED.);
#4733=B_SPLINE_CURVE_WITH_KNOTS('',3,(#29726,#29727,#29728,#29729,#29730,
#29731,#29732,#29733,#29734,#29735,#29736,#29737,#29738,#29739,#29740,#29741,
#29742,#29743,#29744,#29745,#29746,#29747,#29748,#29749,#29750,#29751,#29752,
#29753,#29754,#29755,#29756),.UNSPECIFIED.,.F.,.F.,(4,3,3,3,3,3,3,3,3,3,
4),(-208.641841022927,-208.546084827266,-207.548256670198,-207.049342591663,
-206.550428513129,-206.051514434595,-205.552600356061,-204.554772198993,
-203.556944041925,-202.559115884856,-202.358655715748),.UNSPECIFIED.);
#4734=B_SPLINE_CURVE_WITH_KNOTS('',3,(#29757,#29758,#29759,#29760,#29761,
#29762,#29763,#29764,#29765,#29766,#29767,#29768,#29769,#29770,#29771,#29772,
#29773,#29774,#29775,#29776,#29777,#29778,#29779,#29780,#29781,#29782,#29783,
#29784),.UNSPECIFIED.,.F.,.F.,(4,3,3,3,3,3,3,3,3,4),(199.385818955007,199.565631413652,
200.56345957072,201.561287727788,202.060201806322,202.559115884856,203.556944041925,
204.554772198993,205.552600356061,205.669004262187),.UNSPECIFIED.);
#4735=B_SPLINE_CURVE_WITH_KNOTS('',3,(#29789,#29790,#29791,#29792,#29793,
#29794,#29795,#29796,#29797,#29798,#29799,#29800,#29801,#29802,#29803,#29804,
#29805,#29806,#29807,#29808,#29809,#29810,#29811,#29812,#29813,#29814,#29815,
#29816),.UNSPECIFIED.,.F.,.F.,(4,3,3,3,3,3,3,3,3,4),(-214.925026330107,
-214.533053769675,-214.034139691141,-213.535225612607,-213.036311534073,
-212.537397455539,-211.539569298471,-210.541741141402,-209.543912984334,
-208.641841022927),.UNSPECIFIED.);
#4736=B_SPLINE_CURVE_WITH_KNOTS('',3,(#29817,#29818,#29819,#29820,#29821,
#29822,#29823,#29824,#29825,#29826,#29827,#29828,#29829,#29830,#29831,#29832,
#29833,#29834,#29835,#29836,#29837,#29838,#29839,#29840,#29841,#29842,#29843,
#29844),.UNSPECIFIED.,.F.,.F.,(4,3,3,3,3,3,3,3,3,4),(205.669004262187,206.051514434595,
206.550428513129,207.049342591663,207.548256670198,208.546084827266,209.543912984334,
210.541741141402,211.539569298471,211.952189569366),.UNSPECIFIED.);
#4737=B_SPLINE_CURVE_WITH_KNOTS('',3,(#29849,#29850,#29851,#29852,#29853,
#29854,#29855,#29856,#29857,#29858,#29859,#29860,#29861,#29862,#29863,#29864,
#29865,#29866,#29867,#29868,#29869,#29870,#29871,#29872,#29873),
 .UNSPECIFIED.,.F.,.F.,(4,3,3,3,3,3,3,3,4),(-221.208211637286,-220.345291102013,
-219.48237056674,-218.619450031467,-217.756529496194,-216.893608960921,
-216.030688425647,-215.167767890374,-214.925026330107),.UNSPECIFIED.);
#4738=B_SPLINE_CURVE_WITH_KNOTS('',3,(#29874,#29875,#29876,#29877,#29878,
#29879,#29880,#29881,#29882,#29883,#29884,#29885,#29886,#29887,#29888,#29889,
#29890,#29891,#29892,#29893,#29894,#29895,#29896,#29897,#29898),
 .UNSPECIFIED.,.F.,.F.,(4,3,3,3,3,3,3,3,4),(211.952189569366,212.81511010464,
213.678030639913,214.540951175186,215.403871710459,216.266792245732,217.129712781005,
217.992633316278,218.235374876546),.UNSPECIFIED.);
#4739=B_SPLINE_CURVE_WITH_KNOTS('',3,(#29903,#29904,#29905,#29906,#29907,
#29908,#29909,#29910,#29911,#29912,#29913,#29914,#29915,#29916,#29917,#29918,
#29919,#29920,#29921,#29922,#29923,#29924,#29925,#29926,#29927),
 .UNSPECIFIED.,.F.,.F.,(4,3,3,3,3,3,3,3,4),(-227.491396944466,-227.005905733029,
-226.506991654494,-225.509163497426,-224.511335340358,-223.51350718329,
-222.515679026221,-221.517850869153,-221.208211637286),.UNSPECIFIED.);
#4740=B_SPLINE_CURVE_WITH_KNOTS('',3,(#29928,#29929,#29930,#29931,#29932,
#29933,#29934,#29935,#29936,#29937,#29938,#29939,#29940,#29941,#29942,#29943,
#29944,#29945,#29946,#29947,#29948,#29949,#29950,#29951,#29952,#29953,#29954,
#29955,#29956,#29957,#29958),.UNSPECIFIED.,.F.,.F.,(4,3,3,3,3,3,3,3,3,3,
4),(218.235374876546,218.524366397948,219.522194555017,220.021108633551,
220.520022712085,221.018936790619,221.517850869153,222.515679026221,223.51350718329,
224.511335340358,224.518560183726),.UNSPECIFIED.);
#4741=B_SPLINE_CURVE_WITH_KNOTS('',3,(#29963,#29964,#29965,#29966,#29967,
#29968,#29969,#29970,#29971,#29972,#29973,#29974,#29975,#29976,#29977,#29978,
#29979,#29980,#29981,#29982,#29983,#29984,#29985,#29986,#29987,#29988,#29989,
#29990),.UNSPECIFIED.,.F.,.F.,(4,3,3,3,3,3,3,3,3,4),(-233.774582251646,
-233.491788753972,-232.493960596904,-231.496132439836,-230.498304282767,
-229.500476125699,-228.502647968631,-228.003733890097,-227.504819811563,
-227.491396944466),.UNSPECIFIED.);
#4742=B_SPLINE_CURVE_WITH_KNOTS('',3,(#29991,#29992,#29993,#29994,#29995,
#29996,#29997,#29998,#29999,#30000,#30001,#30002,#30003,#30004,#30005,#30006,
#30007,#30008,#30009,#30010,#30011,#30012,#30013,#30014,#30015,#30016,#30017,
#30018),.UNSPECIFIED.,.F.,.F.,(4,3,3,3,3,3,3,3,3,4),(224.518560183726,225.509163497426,
226.506991654494,227.005905733029,227.504819811563,228.003733890097,228.502647968631,
229.500476125699,230.498304282767,230.801745490905),.UNSPECIFIED.);
#4743=B_SPLINE_CURVE_WITH_KNOTS('',3,(#30023,#30024,#30025,#30026,#30027,
#30028,#30029,#30030,#30031,#30032,#30033,#30034,#30035,#30036,#30037,#30038,
#30039,#30040,#30041,#30042,#30043,#30044,#30045,#30046,#30047),
 .UNSPECIFIED.,.F.,.F.,(4,3,3,3,3,3,3,3,4),(-240.057767558825,-239.194847023552,
-238.331926488279,-237.469005953006,-236.606085417733,-235.74316488246,
-234.880244347186,-234.017323811913,-233.774582251646),.UNSPECIFIED.);
#4744=B_SPLINE_CURVE_WITH_KNOTS('',3,(#30048,#30049,#30050,#30051,#30052,
#30053,#30054,#30055,#30056,#30057,#30058,#30059,#30060,#30061,#30062,#30063,
#30064,#30065,#30066,#30067,#30068,#30069,#30070,#30071,#30072,#30073,#30074,
#30075),.UNSPECIFIED.,.F.,.F.,(4,3,3,3,3,3,3,3,3,4),(230.801745490905,231.496132439836,
232.493960596904,233.491788753972,233.990702832506,234.489616911041,234.988530989575,
235.487445068109,236.485273225177,237.084930798085),.UNSPECIFIED.);
#4745=B_SPLINE_CURVE_WITH_KNOTS('',3,(#30080,#30081,#30082,#30083,#30084,
#30085,#30086,#30087,#30088,#30089,#30090,#30091,#30092,#30093,#30094,#30095,
#30096,#30097,#30098,#30099,#30100,#30101,#30102,#30103,#30104,#30105,#30106,
#30107),.UNSPECIFIED.,.F.,.F.,(4,3,3,3,3,3,3,3,3,4),(-246.340952866005,
-245.465726638791,-244.467898481723,-243.470070324655,-242.472242167587,
-241.973328089052,-241.474414010518,-240.975499931984,-240.47658585345,
-240.057767558825),.UNSPECIFIED.);
#4746=B_SPLINE_CURVE_WITH_KNOTS('',3,(#30108,#30109,#30110,#30111,#30112,
#30113,#30114,#30115,#30116,#30117,#30118,#30119,#30120,#30121,#30122,#30123,
#30124,#30125,#30126,#30127,#30128,#30129,#30130,#30131,#30132,#30133,#30134,
#30135),.UNSPECIFIED.,.F.,.F.,(4,3,3,3,3,3,3,3,3,4),(237.084930798085,237.483101382245,
238.480929539314,239.478757696382,240.47658585345,240.975499931984,241.474414010518,
241.973328089053,242.472242167587,243.368116105264),.UNSPECIFIED.);
#4747=B_SPLINE_CURVE_WITH_KNOTS('',3,(#30140,#30141,#30142,#30143,#30144,
#30145,#30146,#30147,#30148,#30149,#30150,#30151,#30152,#30153,#30154,#30155,
#30156,#30157,#30158,#30159,#30160,#30161,#30162,#30163,#30164,#30165,#30166,
#30167,#30168,#30169,#30170),.UNSPECIFIED.,.F.,.F.,(4,3,3,3,3,3,3,3,3,3,
4),(-252.624138173184,-252.450523738269,-251.452695581201,-250.454867424133,
-249.457039267064,-248.95812518853,-248.459211109996,-247.960297031462,
-247.461382952928,-246.46355479586,-246.340952866005),.UNSPECIFIED.);
#4748=B_SPLINE_CURVE_WITH_KNOTS('',3,(#30171,#30172,#30173,#30174,#30175,
#30176,#30177,#30178,#30179,#30180,#30181,#30182,#30183,#30184,#30185,#30186,
#30187,#30188,#30189,#30190,#30191,#30192,#30193,#30194,#30195),
 .UNSPECIFIED.,.F.,.F.,(4,3,3,3,3,3,3,3,4),(243.368116105264,244.231036640537,
245.093957175811,245.956877711084,246.819798246357,247.68271878163,248.545639316903,
249.408559852176,249.651301412444),.UNSPECIFIED.);
#4749=B_SPLINE_CURVE_WITH_KNOTS('',3,(#30200,#30201,#30202,#30203,#30204,
#30205,#30206,#30207,#30208,#30209,#30210,#30211,#30212,#30213,#30214,#30215,
#30216,#30217,#30218,#30219,#30220,#30221,#30222,#30223,#30224,#30225,#30226,
#30227),.UNSPECIFIED.,.F.,.F.,(4,3,3,3,3,3,3,3,3,4),(-258.907323480364,
-258.437492680679,-257.43966452361,-256.441836366542,-255.942922288008,
-255.444008209474,-254.94509413094,-254.446180052406,-253.448351895337,
-252.624138173184),.UNSPECIFIED.);
#4750=B_SPLINE_CURVE_WITH_KNOTS('',3,(#30228,#30229,#30230,#30231,#30232,
#30233,#30234,#30235,#30236,#30237,#30238,#30239,#30240,#30241,#30242,#30243,
#30244,#30245,#30246,#30247,#30248,#30249,#30250,#30251,#30252),
 .UNSPECIFIED.,.F.,.F.,(4,3,3,3,3,3,3,3,4),(249.651301412444,250.454867424133,
251.452695581201,252.450523738269,253.448351895337,254.446180052406,254.94509413094,
255.444008209474,255.934486719623),.UNSPECIFIED.);
#4751=B_SPLINE_CURVE_WITH_KNOTS('',3,(#30257,#30258,#30259,#30260,#30261,
#30262,#30263,#30264,#30265,#30266,#30267,#30268,#30269,#30270,#30271,#30272,
#30273,#30274,#30275,#30276,#30277,#30278,#30279,#30280,#30281,#30282,#30283,
#30284),.UNSPECIFIED.,.F.,.F.,(4,3,3,3,3,3,3,3,3,4),(-265.190508787543,
-264.424461623088,-263.42663346602,-262.927719387486,-262.428805308952,
-261.929891230418,-261.430977151883,-260.433148994815,-259.435320837747,
-258.907323480364),.UNSPECIFIED.);
#4752=B_SPLINE_CURVE_WITH_KNOTS('',3,(#30285,#30286,#30287,#30288,#30289,
#30290,#30291,#30292,#30293,#30294,#30295,#30296,#30297,#30298,#30299,#30300,
#30301,#30302,#30303,#30304,#30305,#30306,#30307,#30308,#30309,#30310,#30311,
#30312),.UNSPECIFIED.,.F.,.F.,(4,3,3,3,3,3,3,3,3,4),(255.934486719623,255.942922288008,
256.441836366542,257.43966452361,258.437492680679,259.435320837747,260.433148994815,
261.430977151884,261.929891230418,262.217672026803),.UNSPECIFIED.);
#4753=B_SPLINE_CURVE_WITH_KNOTS('',3,(#30317,#30318,#30319,#30320,#30321,
#30322,#30323,#30324,#30325,#30326,#30327,#30328,#30329,#30330,#30331,#30332,
#30333,#30334,#30335,#30336,#30337,#30338,#30339,#30340,#30341,#30342,#30343,
#30344,#30345,#30346,#30347),.UNSPECIFIED.,.F.,.F.,(4,3,3,3,3,3,3,3,3,3,
4),(-271.473694094723,-271.409258722566,-270.411430565498,-269.912516486964,
-269.413602408429,-268.914688329895,-268.415774251361,-267.417946094293,
-266.420117937225,-265.422289780157,-265.190508787543),.UNSPECIFIED.);
#4754=B_SPLINE_CURVE_WITH_KNOTS('',3,(#30348,#30349,#30350,#30351,#30352,
#30353,#30354,#30355,#30356,#30357,#30358,#30359,#30360,#30361,#30362,#30363,
#30364,#30365,#30366,#30367,#30368,#30369,#30370,#30371,#30372),
 .UNSPECIFIED.,.F.,.F.,(4,3,3,3,3,3,3,3,4),(262.217672026803,263.080592562076,
263.943513097349,264.806433632622,265.669354167895,266.532274703169,267.395195238442,
268.258115773715,268.500857333982),.UNSPECIFIED.);
#4755=B_SPLINE_CURVE_WITH_KNOTS('',3,(#30377,#30378,#30379,#30380,#30381,
#30382,#30383,#30384,#30385,#30386,#30387,#30388,#30389,#30390,#30391,#30392,
#30393,#30394,#30395,#30396,#30397,#30398,#30399,#30400,#30401,#30402,#30403,
#30404),.UNSPECIFIED.,.F.,.F.,(4,3,3,3,3,3,3,3,3,4),(-277.756879401903,
-277.396227664976,-276.897313586441,-276.398399507907,-275.899485429373,
-275.400571350839,-274.402743193771,-273.404915036703,-272.407086879634,
-271.473694094723),.UNSPECIFIED.);
#4756=B_SPLINE_CURVE_WITH_KNOTS('',3,(#30405,#30406,#30407,#30408,#30409,
#30410,#30411,#30412,#30413,#30414,#30415,#30416,#30417,#30418,#30419,#30420,
#30421,#30422,#30423,#30424,#30425,#30426,#30427,#30428,#30429,#30430,#30431,
#30432),.UNSPECIFIED.,.F.,.F.,(4,3,3,3,3,3,3,3,3,4),(268.500857333982,268.914688329895,
269.41360240843,269.912516486964,270.411430565498,271.409258722566,272.407086879634,
273.404915036703,274.402743193771,274.784042641162),.UNSPECIFIED.);
#4757=B_SPLINE_CURVE_WITH_KNOTS('',3,(#30437,#30438,#30439,#30440,#30441,
#30442,#30443,#30444,#30445,#30446,#30447,#30448,#30449,#30450,#30451,#30452,
#30453,#30454,#30455,#30456,#30457,#30458,#30459,#30460,#30461),
 .UNSPECIFIED.,.F.,.F.,(4,3,3,3,3,3,3,3,4),(-284.040064709082,-283.177144173809,
-282.314223638536,-281.451303103262,-280.588382567989,-279.725462032716,
-278.862541497443,-277.99962096217,-277.756879401903),.UNSPECIFIED.);
#4758=B_SPLINE_CURVE_WITH_KNOTS('',3,(#30462,#30463,#30464,#30465,#30466,
#30467,#30468,#30469,#30470,#30471,#30472,#30473,#30474,#30475,#30476,#30477,
#30478,#30479,#30480,#30481,#30482,#30483,#30484,#30485,#30486),
 .UNSPECIFIED.,.F.,.F.,(4,3,3,3,3,3,3,3,4),(274.784042641162,275.646963176435,
276.509883711708,277.372804246982,278.235724782255,279.098645317528,279.961565852801,
280.824486388074,281.067227948342),.UNSPECIFIED.);
#4759=B_SPLINE_CURVE_WITH_KNOTS('',3,(#30491,#30492,#30493,#30494,#30495,
#30496,#30497,#30498,#30499,#30500,#30501,#30502,#30503,#30504,#30505,#30506,
#30507,#30508,#30509,#30510,#30511,#30512,#30513,#30514,#30515),
 .UNSPECIFIED.,.F.,.F.,(4,3,3,3,3,3,3,3,4),(-290.323250016262,-289.869079628329,
-289.370165549795,-288.372337392726,-287.374509235658,-286.37668107859,
-285.378852921522,-284.381024764453,-284.040064709082),.UNSPECIFIED.);
#4760=B_SPLINE_CURVE_WITH_KNOTS('',3,(#30516,#30517,#30518,#30519,#30520,
#30521,#30522,#30523,#30524,#30525,#30526,#30527,#30528,#30529,#30530,#30531,
#30532,#30533,#30534,#30535,#30536,#30537,#30538,#30539,#30540,#30541,#30542,
#30543),.UNSPECIFIED.,.F.,.F.,(4,3,3,3,3,3,3,3,3,4),(281.067227948342,281.387540293249,
282.385368450317,282.884282528851,283.383196607385,283.882110685919,284.381024764453,
285.378852921522,286.37668107859,287.350413255521),.UNSPECIFIED.);
#4761=B_SPLINE_CURVE_WITH_KNOTS('',3,(#30548,#30549,#30550,#30551,#30552,
#30553,#30554,#30555,#30556,#30557,#30558,#30559,#30560,#30561,#30562,#30563,
#30564,#30565,#30566,#30567,#30568,#30569,#30570,#30571,#30572,#30573,#30574,
#30575),.UNSPECIFIED.,.F.,.F.,(4,3,3,3,3,3,3,3,3,4),(-296.606435323441,
-296.354962649272,-295.357134492204,-294.359306335136,-293.361478178068,
-292.363650020999,-291.365821863931,-290.866907785397,-290.367993706863,
-290.323250016262),.UNSPECIFIED.);
#4762=B_SPLINE_CURVE_WITH_KNOTS('',3,(#30576,#30577,#30578,#30579,#30580,
#30581,#30582,#30583,#30584,#30585,#30586,#30587,#30588,#30589,#30590,#30591,
#30592,#30593,#30594,#30595,#30596,#30597,#30598,#30599,#30600,#30601,#30602,
#30603,#30604,#30605,#30606),.UNSPECIFIED.,.F.,.F.,(4,3,3,3,3,3,3,3,3,3,
4),(287.350413255521,287.374509235658,288.372337392726,289.370165549795,
289.869079628329,290.367993706863,290.866907785397,291.365821863931,292.363650021,
293.361478178068,293.633598562701),.UNSPECIFIED.);
#4763=B_SPLINE_CURVE_WITH_KNOTS('',3,(#30611,#30612,#30613,#30614,#30615,
#30616,#30617,#30618,#30619,#30620,#30621,#30622,#30623,#30624,#30625,#30626,
#30627,#30628,#30629,#30630,#30631,#30632,#30633,#30634,#30635),
 .UNSPECIFIED.,.F.,.F.,(4,3,3,3,3,3,3,3,4),(-302.889620630621,-302.026700095348,
-301.163779560074,-300.300859024801,-299.437938489528,-298.575017954255,
-297.712097418982,-296.849176883708,-296.606435323441),.UNSPECIFIED.);
#4764=B_SPLINE_CURVE_WITH_KNOTS('',3,(#30636,#30637,#30638,#30639,#30640,
#30641,#30642,#30643,#30644,#30645,#30646,#30647,#30648,#30649,#30650,#30651,
#30652,#30653,#30654,#30655,#30656,#30657,#30658,#30659,#30660,#30661,#30662,
#30663),.UNSPECIFIED.,.F.,.F.,(4,3,3,3,3,3,3,3,3,4),(293.633598562701,294.359306335136,
295.357134492204,296.354962649273,296.853876727807,297.352790806341,297.851704884875,
298.350618963409,299.348447120477,299.91678386988),.UNSPECIFIED.);
#4765=B_SPLINE_CURVE_WITH_KNOTS('',3,(#30668,#30669,#30670,#30671,#30672,
#30673,#30674,#30675,#30676,#30677,#30678,#30679,#30680,#30681,#30682,#30683,
#30684,#30685,#30686,#30687,#30688,#30689,#30690,#30691,#30692,#30693,#30694,
#30695),.UNSPECIFIED.,.F.,.F.,(4,3,3,3,3,3,3,3,3,4),(-309.1728059378,-308.328900534092,
-307.331072377023,-306.333244219955,-305.335416062887,-304.836501984353,
-304.337587905819,-303.838673827284,-303.33975974875,-302.889620630621),
 .UNSPECIFIED.);
#4766=B_SPLINE_CURVE_WITH_KNOTS('',3,(#30696,#30697,#30698,#30699,#30700,
#30701,#30702,#30703,#30704,#30705,#30706,#30707,#30708,#30709,#30710,#30711,
#30712,#30713,#30714,#30715,#30716,#30717,#30718,#30719,#30720,#30721,#30722,
#30723),.UNSPECIFIED.,.F.,.F.,(4,3,3,3,3,3,3,3,3,4),(299.91678386988,300.346275277546,
301.344103434614,302.341931591682,303.33975974875,303.838673827284,304.337587905819,
304.836501984353,305.335416062887,306.19996917706),.UNSPECIFIED.);
#4767=B_SPLINE_CURVE_WITH_KNOTS('',3,(#30728,#30729,#30730,#30731,#30732,
#30733,#30734,#30735,#30736,#30737,#30738,#30739,#30740,#30741,#30742,#30743,
#30744,#30745,#30746,#30747,#30748,#30749,#30750,#30751,#30752,#30753,#30754,
#30755,#30756,#30757,#30758),.UNSPECIFIED.,.F.,.F.,(4,3,3,3,3,3,3,3,3,3,
4),(-315.45599124498,-315.313697633569,-314.315869476501,-313.318041319433,
-312.320213162365,-311.82129908383,-311.322385005296,-310.823470926762,
-310.324556848228,-309.32672869116,-309.1728059378),.UNSPECIFIED.);
#4768=B_SPLINE_CURVE_WITH_KNOTS('',3,(#30759,#30760,#30761,#30762,#30763,
#30764,#30765,#30766,#30767,#30768,#30769,#30770,#30771,#30772,#30773,#30774,
#30775,#30776,#30777,#30778,#30779,#30780,#30781,#30782,#30783),
 .UNSPECIFIED.,.F.,.F.,(4,3,3,3,3,3,3,3,4),(306.19996917706,307.062889712333,
307.925810247606,308.788730782879,309.651651318153,310.514571853426,311.377492388699,
312.240412923972,312.483154484239),.UNSPECIFIED.);
#4769=B_SPLINE_CURVE_WITH_KNOTS('',3,(#30788,#30789,#30790,#30791,#30792,
#30793,#30794,#30795,#30796,#30797,#30798,#30799,#30800,#30801,#30802,#30803,
#30804,#30805,#30806,#30807,#30808,#30809,#30810,#30811,#30812,#30813,#30814,
#30815),.UNSPECIFIED.,.F.,.F.,(4,3,3,3,3,3,3,3,3,4),(-321.739176552159,
-321.300666575979,-320.302838418911,-319.305010261842,-318.806096183308,
-318.307182104774,-317.80826802624,-317.309353947706,-316.311525790638,
-315.45599124498),.UNSPECIFIED.);
#4770=B_SPLINE_CURVE_WITH_KNOTS('',3,(#30816,#30817,#30818,#30819,#30820,
#30821,#30822,#30823,#30824,#30825,#30826,#30827,#30828,#30829,#30830,#30831,
#30832,#30833,#30834,#30835,#30836,#30837,#30838,#30839,#30840),
 .UNSPECIFIED.,.F.,.F.,(4,3,3,3,3,3,3,3,4),(312.483154484239,313.318041319433,
314.315869476501,315.313697633569,316.311525790638,317.309353947706,317.80826802624,
318.307182104774,318.766339791419),.UNSPECIFIED.);
#4771=B_SPLINE_CURVE_WITH_KNOTS('',3,(#30845,#30846,#30847,#30848,#30849,
#30850,#30851,#30852,#30853,#30854,#30855,#30856,#30857,#30858,#30859,#30860,
#30861,#30862,#30863,#30864,#30865,#30866,#30867,#30868,#30869,#30870,#30871,
#30872),.UNSPECIFIED.,.F.,.F.,(4,3,3,3,3,3,3,3,3,4),(-328.022361859339,
-327.287635518388,-326.28980736132,-325.790893282786,-325.291979204252,
-324.793065125718,-324.294151047184,-323.296322890115,-322.298494733047,
-321.739176552159),.UNSPECIFIED.);
#4772=B_SPLINE_CURVE_WITH_KNOTS('',3,(#30873,#30874,#30875,#30876,#30877,
#30878,#30879,#30880,#30881,#30882,#30883,#30884,#30885,#30886,#30887,#30888,
#30889,#30890,#30891,#30892,#30893,#30894,#30895,#30896,#30897,#30898,#30899,
#30900),.UNSPECIFIED.,.F.,.F.,(4,3,3,3,3,3,3,3,3,4),(318.766339791419,318.806096183308,
319.305010261842,320.302838418911,321.300666575979,322.298494733047,323.296322890116,
324.294151047184,324.793065125718,325.049525098599),.UNSPECIFIED.);
#4773=B_SPLINE_CURVE_WITH_KNOTS('',3,(#30905,#30906,#30907,#30908,#30909,
#30910,#30911,#30912,#30913,#30914,#30915,#30916,#30917,#30918,#30919,#30920,
#30921,#30922,#30923,#30924,#30925,#30926,#30927,#30928,#30929,#30930,#30931,
#30932,#30933,#30934,#30935),.UNSPECIFIED.,.F.,.F.,(4,3,3,3,3,3,3,3,3,3,
4),(-334.305547166519,-334.272432617866,-333.274604460798,-332.775690382264,
-332.27677630373,-331.777862225196,-331.278948146661,-330.281119989593,
-329.283291832525,-328.285463675457,-328.022361859339),.UNSPECIFIED.);
#4774=B_SPLINE_CURVE_WITH_KNOTS('',3,(#30936,#30937,#30938,#30939,#30940,
#30941,#30942,#30943,#30944,#30945,#30946,#30947,#30948,#30949,#30950,#30951,
#30952,#30953,#30954,#30955,#30956,#30957,#30958,#30959,#30960,#30961,#30962,
#30963),.UNSPECIFIED.,.F.,.F.,(4,3,3,3,3,3,3,3,3,4),(325.049525098599,325.291979204252,
325.790893282786,326.28980736132,327.287635518389,328.285463675457,329.283291832525,
330.281119989593,331.278948146662,331.332710405778),.UNSPECIFIED.);
#4775=B_SPLINE_CURVE_WITH_KNOTS('',3,(#30968,#30969,#30970,#30971,#30972,
#30973,#30974,#30975,#30976,#30977,#30978,#30979,#30980,#30981,#30982,#30983,
#30984,#30985,#30986,#30987,#30988,#30989,#30990,#30991,#30992,#30993,#30994,
#30995),.UNSPECIFIED.,.F.,.F.,(4,3,3,3,3,3,3,3,3,4),(-340.588732473698,
-340.259401560276,-339.760487481742,-339.261573403207,-338.762659324673,
-338.263745246139,-337.265917089071,-336.268088932003,-335.270260774934,
-334.305547166519),.UNSPECIFIED.);
#4776=B_SPLINE_CURVE_WITH_KNOTS('',3,(#30996,#30997,#30998,#30999,#31000,
#31001,#31002,#31003,#31004,#31005,#31006,#31007,#31008,#31009,#31010,#31011,
#31012,#31013,#31014,#31015,#31016,#31017,#31018,#31019,#31020,#31021,#31022,
#31023),.UNSPECIFIED.,.F.,.F.,(4,3,3,3,3,3,3,3,3,4),(331.332710405778,331.777862225196,
332.27677630373,332.775690382264,333.274604460798,334.272432617866,335.270260774935,
336.268088932003,337.265917089071,337.615895712958),.UNSPECIFIED.);
#4777=B_SPLINE_CURVE_WITH_KNOTS('',3,(#31028,#31029,#31030,#31031,#31032,
#31033,#31034,#31035,#31036,#31037,#31038,#31039,#31040,#31041,#31042,#31043,
#31044,#31045,#31046,#31047,#31048,#31049,#31050,#31051,#31052),
 .UNSPECIFIED.,.F.,.F.,(4,3,3,3,3,3,3,3,4),(-346.871917780878,-346.008997245604,
-345.146076710331,-344.283156175058,-343.420235639785,-342.557315104512,
-341.694394569239,-340.831474033966,-340.588732473698),.UNSPECIFIED.);
#4778=B_SPLINE_CURVE_WITH_KNOTS('',3,(#31053,#31054,#31055,#31056,#31057,
#31058,#31059,#31060,#31061,#31062,#31063,#31064,#31065,#31066,#31067,#31068,
#31069,#31070,#31071,#31072,#31073,#31074,#31075,#31076,#31077),
 .UNSPECIFIED.,.F.,.F.,(4,3,3,3,3,3,3,3,4),(337.615895712958,338.478816248231,
339.341736783504,340.204657318777,341.06757785405,341.930498389324,342.793418924597,
343.65633945987,343.899081020137),.UNSPECIFIED.);
#4779=B_SPLINE_CURVE_WITH_KNOTS('',3,(#31082,#31083,#31084,#31085,#31086,
#31087,#31088,#31089,#31090,#31091,#31092,#31093,#31094,#31095,#31096,#31097,
#31098,#31099,#31100,#31101,#31102,#31103,#31104,#31105,#31106),
 .UNSPECIFIED.,.F.,.F.,(4,3,3,3,3,3,3,3,4),(-353.155103088057,-352.732253523629,
-352.233339445095,-351.235511288027,-350.237683130958,-349.23985497389,
-348.242026816822,-347.244198659754,-346.871917780878),.UNSPECIFIED.);
#4780=B_SPLINE_CURVE_WITH_KNOTS('',3,(#31107,#31108,#31109,#31110,#31111,
#31112,#31113,#31114,#31115,#31116,#31117,#31118,#31119,#31120,#31121,#31122,
#31123,#31124,#31125,#31126,#31127,#31128,#31129,#31130,#31131,#31132,#31133,
#31134),.UNSPECIFIED.,.F.,.F.,(4,3,3,3,3,3,3,3,3,4),(343.899081020137,344.250714188549,
345.248542345617,345.747456424151,346.246370502685,346.74528458122,347.244198659754,
348.242026816822,349.23985497389,350.182266327317),.UNSPECIFIED.);
#4781=B_SPLINE_CURVE_WITH_KNOTS('',3,(#31139,#31140,#31141,#31142,#31143,
#31144,#31145,#31146,#31147,#31148,#31149,#31150,#31151,#31152,#31153,#31154,
#31155,#31156,#31157,#31158,#31159,#31160,#31161,#31162,#31163),
 .UNSPECIFIED.,.F.,.F.,(4,3,3,3,3,3,3,3,4),(-359.438288395237,-358.575367859964,
-357.712447324691,-356.849526789417,-355.986606254144,-355.123685718871,
-354.260765183598,-353.397844648325,-353.155103088057),.UNSPECIFIED.);
#4782=B_SPLINE_CURVE_WITH_KNOTS('',3,(#31164,#31165,#31166,#31167,#31168,
#31169,#31170,#31171,#31172,#31173,#31174,#31175,#31176,#31177,#31178,#31179,
#31180,#31181,#31182,#31183,#31184,#31185,#31186,#31187,#31188,#31189,#31190,
#31191,#31192,#31193,#31194),.UNSPECIFIED.,.F.,.F.,(4,3,3,3,3,3,3,3,3,3,
4),(350.182266327317,350.237683130958,351.235511288027,352.233339445095,
352.732253523629,353.231167602163,353.730081680697,354.228995759231,355.2268239163,
356.224652073368,356.465451634496),.UNSPECIFIED.);
#4783=B_SPLINE_CURVE_WITH_KNOTS('',3,(#31199,#31200,#31201,#31202,#31203,
#31204,#31205,#31206,#31207,#31208,#31209,#31210,#31211,#31212,#31213,#31214,
#31215,#31216,#31217,#31218,#31219,#31220,#31221,#31222,#31223),
 .UNSPECIFIED.,.F.,.F.,(4,3,3,3,3,3,3,3,4),(-365.721473702416,-364.858553167143,
-363.99563263187,-363.132712096597,-362.269791561324,-361.406871026051,
-360.543950490778,-359.681029955504,-359.438288395237),.UNSPECIFIED.);
#4784=B_SPLINE_CURVE_WITH_KNOTS('',3,(#31224,#31225,#31226,#31227,#31228,
#31229,#31230,#31231,#31232,#31233,#31234,#31235,#31236,#31237,#31238,#31239,
#31240,#31241,#31242,#31243,#31244,#31245,#31246,#31247,#31248,#31249,#31250,
#31251),.UNSPECIFIED.,.F.,.F.,(4,3,3,3,3,3,3,3,3,4),(356.465451634496,357.222480230436,
358.220308387505,359.218136544573,359.717050623107,360.215964701641,360.714878780175,
361.213792858709,362.211621015778,362.748636941676),.UNSPECIFIED.);
#4785=B_SPLINE_CURVE_WITH_KNOTS('',3,(#31256,#31257,#31258,#31259,#31260,
#31261,#31262,#31263,#31264,#31265,#31266,#31267,#31268,#31269,#31270,#31271,
#31272,#31273,#31274,#31275,#31276,#31277,#31278,#31279,#31280),
 .UNSPECIFIED.,.F.,.F.,(4,3,3,3,3,3,3,3,4),(-372.004659009596,-371.141738474323,
-370.278817939049,-369.415897403776,-368.552976868503,-367.69005633323,
-366.827135797956,-365.964215262683,-365.721473702416),.UNSPECIFIED.);
#4786=B_SPLINE_CURVE_WITH_KNOTS('',3,(#31281,#31282,#31283,#31284,#31285,
#31286,#31287,#31288,#31289,#31290,#31291,#31292,#31293,#31294,#31295,#31296,
#31297,#31298,#31299,#31300,#31301,#31302,#31303,#31304,#31305,#31306,#31307,
#31308),.UNSPECIFIED.,.F.,.F.,(4,3,3,3,3,3,3,3,3,4),(362.748636941676,363.209449172846,
364.207277329914,365.205105486982,366.202933644051,366.701847722585,367.200761801119,
367.699675879653,368.198589958187,369.031822248856),.UNSPECIFIED.);
#4787=B_SPLINE_CURVE_WITH_KNOTS('',3,(#31313,#31314,#31315,#31316,#31317,
#31318,#31319,#31320,#31321,#31322,#31323,#31324,#31325,#31326,#31327,#31328,
#31329,#31330,#31331,#31332,#31333,#31334,#31335,#31336,#31337,#31338,#31339,
#31340,#31341,#31342,#31343),.UNSPECIFIED.,.F.,.F.,(4,3,3,3,3,3,3,3,3,3,
4),(-378.287844316776,-378.17687152887,-377.179043371801,-376.181215214733,
-375.183387057665,-374.684472979131,-374.185558900597,-373.686644822062,
-373.187730743528,-372.18990258646,-372.004659009596),.UNSPECIFIED.);
#4788=B_SPLINE_CURVE_WITH_KNOTS('',3,(#31344,#31345,#31346,#31347,#31348,
#31349,#31350,#31351,#31352,#31353,#31354,#31355,#31356,#31357,#31358,#31359,
#31360,#31361,#31362,#31363,#31364,#31365,#31366,#31367,#31368),
 .UNSPECIFIED.,.F.,.F.,(4,3,3,3,3,3,3,3,4),(369.031822248856,369.894742784129,
370.757663319402,371.620583854675,372.483504389948,373.346424925221,374.209345460494,
375.072265995767,375.315007556035),.UNSPECIFIED.);
#4789=B_SPLINE_CURVE_WITH_KNOTS('',3,(#31373,#31374,#31375,#31376,#31377,
#31378,#31379,#31380,#31381,#31382,#31383,#31384,#31385,#31386,#31387,#31388,
#31389,#31390,#31391,#31392,#31393,#31394,#31395,#31396,#31397,#31398,#31399,
#31400),.UNSPECIFIED.,.F.,.F.,(4,3,3,3,3,3,3,3,3,4),(-384.571029623955,
-384.163840471279,-383.166012314211,-382.168184157143,-381.669270078608,
-381.170356000074,-380.67144192154,-380.172527843006,-379.174699685938,
-378.287844316776),.UNSPECIFIED.);
#4790=B_SPLINE_CURVE_WITH_KNOTS('',3,(#31401,#31402,#31403,#31404,#31405,
#31406,#31407,#31408,#31409,#31410,#31411,#31412,#31413,#31414,#31415,#31416,
#31417,#31418,#31419,#31420,#31421,#31422,#31423,#31424,#31425),
 .UNSPECIFIED.,.F.,.F.,(4,3,3,3,3,3,3,3,4),(375.315007556035,376.181215214733,
377.179043371801,378.17687152887,379.174699685938,380.172527843006,380.67144192154,
381.170356000074,381.598192863215),.UNSPECIFIED.);
#4791=B_SPLINE_CURVE_WITH_KNOTS('',3,(#31430,#31431,#31432,#31433,#31434,
#31435,#31436,#31437,#31438,#31439,#31440,#31441,#31442,#31443,#31444,#31445,
#31446,#31447,#31448,#31449,#31450,#31451,#31452,#31453,#31454,#31455,#31456,
#31457),.UNSPECIFIED.,.F.,.F.,(4,3,3,3,3,3,3,3,3,4),(-390.854214931135,
-390.150809413689,-389.15298125662,-388.654067178086,-388.155153099552,
-387.656239021018,-387.157324942484,-386.159496785416,-385.161668628347,
-384.571029623955),.UNSPECIFIED.);
#4792=B_SPLINE_CURVE_WITH_KNOTS('',3,(#31458,#31459,#31460,#31461,#31462,
#31463,#31464,#31465,#31466,#31467,#31468,#31469,#31470,#31471,#31472,#31473,
#31474,#31475,#31476,#31477,#31478,#31479,#31480,#31481,#31482,#31483,#31484,
#31485),.UNSPECIFIED.,.F.,.F.,(4,3,3,3,3,3,3,3,3,4),(381.598192863215,381.669270078609,
382.168184157143,383.166012314211,384.163840471279,385.161668628347,386.159496785416,
387.157324942484,387.656239021018,387.881378170394),.UNSPECIFIED.);
#4793=B_SPLINE_CURVE_WITH_KNOTS('',3,(#31491,#31492,#31493,#31494,#31495,
#31496,#31497,#31498,#31499,#31500,#31501,#31502,#31503),.UNSPECIFIED.,
 .F.,.F.,(4,3,3,3,4),(-3.8100000088729,-3.48648673068836,-2.98841719773288,
-2.4903476647774,-2.07135887395545),.UNSPECIFIED.);
#4794=B_SPLINE_CURVE_WITH_KNOTS('',3,(#31511,#31512,#31513,#31514,#31515,
#31516,#31517),.UNSPECIFIED.,.F.,.F.,(4,3,4),(0.,0.498069532955476,0.837163248131365),
 .UNSPECIFIED.);
#4795=B_SPLINE_CURVE_WITH_KNOTS('',3,(#31522,#31523,#31524,#31525,#31526,
#31527,#31528,#31529,#31530,#31531,#31532,#31533,#31534,#31535,#31536,#31537,
#31538,#31539,#31540,#31541,#31542,#31543,#31544,#31545,#31546,#31547,#31548,
#31549,#31550,#31551,#31552,#31553,#31554,#31555,#31556,#31557,#31558,#31559,
#31560,#31561,#31562,#31563,#31564),.UNSPECIFIED.,.F.,.F.,(4,3,3,3,3,3,
3,3,3,3,3,3,3,3,4),(-10.0931853160525,-9.96139065910959,-9.46332112615411,
-8.96525159319863,-8.46718206024316,-7.96911252728767,-7.47104299433219,
-6.97297346137671,-6.47490392842124,-5.97683439546575,-5.47876486251027,
-4.9806953295548,-4.48262579659932,-3.98455626364384,-3.8100000088729),
 .UNSPECIFIED.);
#4796=B_SPLINE_CURVE_WITH_KNOTS('',3,(#31565,#31566,#31567,#31568,#31569,
#31570,#31571,#31572,#31573,#31574,#31575,#31576,#31577,#31578,#31579,#31580,
#31581,#31582,#31583,#31584,#31585,#31586,#31587,#31588,#31589,#31590,#31591,
#31592,#31593,#31594,#31595,#31596,#31597,#31598,#31599,#31600,#31601,#31602,
#31603,#31604,#31605,#31606,#31607),.UNSPECIFIED.,.F.,.F.,(4,3,3,3,3,3,
3,3,3,3,3,3,3,3,4),(0.837163248131365,0.996139065910959,1.49420859886644,
1.99227813182192,2.4903476647774,2.98841719773287,3.48648673068835,3.98455626364383,
4.48262579659931,4.98069532955479,5.47876486251027,5.97683439546575,6.47490392842123,
6.97297346137671,7.12034855531095),.UNSPECIFIED.);
#4797=B_SPLINE_CURVE_WITH_KNOTS('',3,(#31612,#31613,#31614,#31615,#31616,
#31617,#31618,#31619,#31620,#31621,#31622,#31623,#31624,#31625,#31626,#31627,
#31628,#31629,#31630,#31631,#31632,#31633,#31634,#31635,#31636,#31637,#31638,
#31639,#31640,#31641,#31642,#31643,#31644,#31645,#31646,#31647,#31648,#31649,
#31650,#31651),.UNSPECIFIED.,.F.,.F.,(4,3,3,3,3,3,3,3,3,3,3,3,3,4),(-16.3763706232321,
-15.9382250545753,-15.4401555216199,-14.9420859886644,-14.4440164557089,
-13.9459469227534,-13.4478773897979,-12.9498078568425,-12.451738323887,
-11.9536687909315,-11.455599257976,-10.9575297250205,-10.4594601920651,
-10.0931853160525),.UNSPECIFIED.);
#4798=B_SPLINE_CURVE_WITH_KNOTS('',3,(#31652,#31653,#31654,#31655,#31656,
#31657,#31658,#31659,#31660,#31661,#31662,#31663,#31664,#31665,#31666,#31667,
#31668,#31669,#31670,#31671,#31672,#31673,#31674,#31675,#31676,#31677,#31678,
#31679,#31680,#31681,#31682,#31683,#31684,#31685,#31686,#31687,#31688,#31689,
#31690,#31691),.UNSPECIFIED.,.F.,.F.,(4,3,3,3,3,3,3,3,3,3,3,3,3,4),(7.12034855531095,
7.47104299433219,7.96911252728767,8.46718206024315,8.96525159319863,9.46332112615411,
9.96139065910959,10.4594601920651,10.9575297250206,11.455599257976,11.9536687909315,
12.451738323887,12.9498078568425,13.4035338624905),.UNSPECIFIED.);
#4799=B_SPLINE_CURVE_WITH_KNOTS('',3,(#31696,#31697,#31698,#31699,#31700,
#31701,#31702,#31703,#31704,#31705,#31706,#31707,#31708,#31709,#31710,#31711,
#31712,#31713,#31714,#31715,#31716,#31717,#31718,#31719,#31720,#31721,#31722,
#31723,#31724,#31725,#31726,#31727,#31728,#31729,#31730,#31731,#31732,#31733,
#31734,#31735,#31736,#31737,#31738),.UNSPECIFIED.,.F.,.F.,(4,3,3,3,3,3,
3,3,3,3,3,3,3,3,4),(-22.6595559304117,-22.4131289829966,-21.9150594500411,
-21.4169899170856,-20.9189203841301,-20.4208508511747,-19.9227813182192,
-19.4247117852637,-18.9266422523082,-18.4285727193527,-17.9305031863973,
-17.4324336534418,-16.9343641204863,-16.4362945875308,-16.3763706232321),
 .UNSPECIFIED.);
#4800=B_SPLINE_CURVE_WITH_KNOTS('',3,(#31739,#31740,#31741,#31742,#31743,
#31744,#31745,#31746,#31747,#31748,#31749,#31750,#31751,#31752,#31753,#31754,
#31755,#31756,#31757,#31758,#31759,#31760,#31761,#31762,#31763,#31764,#31765,
#31766,#31767,#31768,#31769,#31770,#31771,#31772,#31773,#31774,#31775,#31776,
#31777,#31778,#31779,#31780,#31781),.UNSPECIFIED.,.F.,.F.,(4,3,3,3,3,3,
3,3,3,3,3,3,3,3,4),(13.4035338624905,13.447877389798,13.9459469227534,14.4440164557089,
14.9420859886644,15.4401555216199,15.9382250545754,16.4362945875308,16.9343641204863,
17.4324336534418,17.9305031863973,18.4285727193527,18.9266422523082,19.4247117852637,
19.6867191696701),.UNSPECIFIED.);
#4801=B_SPLINE_CURVE_WITH_KNOTS('',3,(#31786,#31787,#31788,#31789,#31790,
#31791,#31792,#31793,#31794,#31795,#31796,#31797,#31798,#31799,#31800,#31801,
#31802,#31803,#31804,#31805,#31806,#31807,#31808,#31809,#31810,#31811,#31812,
#31813,#31814,#31815,#31816,#31817,#31818,#31819,#31820,#31821,#31822,#31823,
#31824,#31825,#31826,#31827,#31828),.UNSPECIFIED.,.F.,.F.,(4,3,3,3,3,3,
3,3,3,3,3,3,3,3,4),(-28.9427412375912,-28.8880329114178,-28.3899633784623,
-27.8918938455068,-27.3938243125514,-26.8957547795959,-26.3976852466404,
-25.8996157136849,-25.4015461807295,-24.903476647774,-24.4054071148185,
-23.907337581863,-23.4092680489075,-22.9111985159521,-22.6595559304117),
 .UNSPECIFIED.);
#4802=B_SPLINE_CURVE_WITH_KNOTS('',3,(#31829,#31830,#31831,#31832,#31833,
#31834,#31835,#31836,#31837,#31838,#31839,#31840,#31841,#31842,#31843,#31844,
#31845,#31846,#31847,#31848,#31849,#31850,#31851,#31852,#31853,#31854,#31855,
#31856,#31857,#31858,#31859,#31860,#31861,#31862,#31863,#31864,#31865,#31866,
#31867,#31868,#31869,#31870,#31871),.UNSPECIFIED.,.F.,.F.,(4,3,3,3,3,3,
3,3,3,3,3,3,3,3,4),(19.6867191696701,19.9227813182192,20.4208508511747,
20.9189203841301,21.4169899170856,21.9150594500411,22.4131289829966,22.9111985159521,
23.4092680489075,23.907337581863,24.4054071148185,24.903476647774,25.4015461807295,
25.899615713685,25.9699044768497),.UNSPECIFIED.);
#4803=B_SPLINE_CURVE_WITH_KNOTS('',3,(#31876,#31877,#31878,#31879,#31880,
#31881,#31882,#31883,#31884,#31885,#31886,#31887,#31888,#31889,#31890,#31891,
#31892,#31893,#31894,#31895,#31896,#31897,#31898,#31899,#31900,#31901,#31902,
#31903,#31904,#31905,#31906,#31907,#31908,#31909,#31910,#31911,#31912,#31913,
#31914,#31915),.UNSPECIFIED.,.F.,.F.,(4,3,3,3,3,3,3,3,3,3,3,3,3,4),(-35.2259265447708,
-34.8648673068836,-34.3667977739281,-33.8687282409726,-33.3706587080171,
-32.8725891750617,-32.3745196421062,-31.8764501091507,-31.3783805761952,
-30.8803110432397,-30.3822415102843,-29.8841719773288,-29.3861024443733,
-28.9427412375912),.UNSPECIFIED.);
#4804=B_SPLINE_CURVE_WITH_KNOTS('',3,(#31916,#31917,#31918,#31919,#31920,
#31921,#31922,#31923,#31924,#31925,#31926,#31927,#31928,#31929,#31930,#31931,
#31932,#31933,#31934,#31935,#31936,#31937,#31938,#31939,#31940,#31941,#31942,
#31943,#31944,#31945,#31946,#31947,#31948,#31949,#31950,#31951,#31952,#31953,
#31954,#31955),.UNSPECIFIED.,.F.,.F.,(4,3,3,3,3,3,3,3,3,3,3,3,3,4),(25.9699044768497,
26.3976852466404,26.8957547795959,27.3938243125514,27.8918938455069,28.3899633784623,
28.8880329114178,29.3861024443733,29.8841719773288,30.3822415102843,30.8803110432397,
31.3783805761952,31.8764501091507,32.2530897840293),.UNSPECIFIED.);
#4805=B_SPLINE_CURVE_WITH_KNOTS('',3,(#31960,#31961,#31962,#31963,#31964,
#31965,#31966,#31967,#31968,#31969,#31970,#31971,#31972,#31973,#31974,#31975,
#31976,#31977,#31978,#31979,#31980,#31981,#31982,#31983,#31984,#31985,#31986,
#31987,#31988,#31989,#31990,#31991,#31992,#31993,#31994,#31995,#31996,#31997,
#31998,#31999,#32000,#32001,#32002),.UNSPECIFIED.,.F.,.F.,(4,3,3,3,3,3,
3,3,3,3,3,3,3,3,4),(-41.5091118519504,-41.3397712353048,-40.8417017023493,
-40.3436321693938,-39.8455626364384,-39.3474931034829,-38.8494235705274,
-38.3513540375719,-37.8532845046164,-37.355214971661,-36.8571454387055,
-36.35907590575,-35.8610063727945,-35.362936839839,-35.2259265447708),
 .UNSPECIFIED.);
#4806=B_SPLINE_CURVE_WITH_KNOTS('',3,(#32003,#32004,#32005,#32006,#32007,
#32008,#32009,#32010,#32011,#32012,#32013,#32014,#32015,#32016,#32017,#32018,
#32019,#32020,#32021,#32022,#32023,#32024,#32025,#32026,#32027,#32028,#32029,
#32030,#32031,#32032,#32033,#32034,#32035,#32036,#32037,#32038,#32039,#32040,
#32041,#32042,#32043,#32044,#32045),.UNSPECIFIED.,.F.,.F.,(4,3,3,3,3,3,
3,3,3,3,3,3,3,3,4),(32.2530897840293,32.3745196421062,32.8725891750617,
33.3706587080171,33.8687282409726,34.3667977739281,34.8648673068836,35.3629368398391,
35.8610063727945,36.35907590575,36.8571454387055,37.355214971661,37.8532845046165,
38.3513540375719,38.5362750912089),.UNSPECIFIED.);
#4807=B_SPLINE_CURVE_WITH_KNOTS('',3,(#32050,#32051,#32052,#32053,#32054,
#32055,#32056,#32057,#32058,#32059,#32060,#32061,#32062,#32063,#32064,#32065,
#32066,#32067,#32068,#32069,#32070,#32071,#32072,#32073,#32074,#32075,#32076,
#32077,#32078,#32079,#32080,#32081,#32082,#32083,#32084,#32085,#32086,#32087,
#32088,#32089),.UNSPECIFIED.,.F.,.F.,(4,3,3,3,3,3,3,3,3,3,3,3,3,4),(-47.79229715913,
-47.3166056307706,-46.8185360978151,-46.3204665648596,-45.8223970319041,
-45.3243274989486,-44.8262579659932,-44.3281884330377,-43.8301189000822,
-43.3320493671267,-42.8339798341712,-42.3359103012158,-41.8378407682603,
-41.5091118519504),.UNSPECIFIED.);
#4808=B_SPLINE_CURVE_WITH_KNOTS('',3,(#32090,#32091,#32092,#32093,#32094,
#32095,#32096,#32097,#32098,#32099,#32100,#32101,#32102,#32103,#32104,#32105,
#32106,#32107,#32108,#32109,#32110,#32111,#32112,#32113,#32114,#32115,#32116,
#32117,#32118,#32119,#32120,#32121,#32122,#32123,#32124,#32125,#32126,#32127,
#32128,#32129),.UNSPECIFIED.,.F.,.F.,(4,3,3,3,3,3,3,3,3,3,3,3,3,4),(38.5362750912089,
38.8494235705274,39.3474931034829,39.8455626364384,40.3436321693939,40.8417017023493,
41.3397712353048,41.8378407682603,42.3359103012158,42.8339798341713,43.3320493671267,
43.8301189000822,44.3281884330377,44.8194603983885),.UNSPECIFIED.);
#4809=B_SPLINE_CURVE_WITH_KNOTS('',3,(#32134,#32135,#32136,#32137,#32138,
#32139,#32140,#32141,#32142,#32143,#32144,#32145,#32146,#32147,#32148,#32149,
#32150,#32151,#32152,#32153,#32154,#32155,#32156,#32157,#32158,#32159,#32160,
#32161,#32162,#32163,#32164,#32165,#32166,#32167,#32168,#32169,#32170,#32171,
#32172,#32173,#32174,#32175,#32176),.UNSPECIFIED.,.F.,.F.,(4,3,3,3,3,3,
3,3,3,3,3,3,3,3,4),(-54.0754824663096,-53.7915095591918,-53.2934400262363,
-52.7953704932808,-52.2973009603254,-51.7992314273699,-51.3011618944144,
-50.8030923614589,-50.3050228285034,-49.8069532955479,-49.3088837625925,
-48.810814229637,-48.3127446966815,-47.814675163726,-47.79229715913),
 .UNSPECIFIED.);
#4810=B_SPLINE_CURVE_WITH_KNOTS('',3,(#32177,#32178,#32179,#32180,#32181,
#32182,#32183,#32184,#32185,#32186,#32187,#32188,#32189,#32190,#32191,#32192,
#32193,#32194,#32195,#32196,#32197,#32198,#32199,#32200,#32201,#32202,#32203,
#32204,#32205,#32206,#32207,#32208,#32209,#32210,#32211,#32212,#32213,#32214,
#32215,#32216,#32217,#32218,#32219),.UNSPECIFIED.,.F.,.F.,(4,3,3,3,3,3,
3,3,3,3,3,3,3,3,4),(44.8194603983885,44.8262579659932,45.3243274989487,
45.8223970319041,46.3204665648596,46.8185360978151,47.3166056307706,47.8146751637261,
48.3127446966815,48.810814229637,49.3088837625925,49.806953295548,50.3050228285035,
50.8030923614589,51.1026457055681),.UNSPECIFIED.);
#4811=B_SPLINE_CURVE_WITH_KNOTS('',3,(#32224,#32225,#32226,#32227,#32228,
#32229,#32230,#32231,#32232,#32233,#32234,#32235,#32236,#32237,#32238,#32239,
#32240,#32241,#32242,#32243,#32244,#32245,#32246,#32247,#32248,#32249,#32250,
#32251,#32252,#32253,#32254,#32255,#32256,#32257,#32258,#32259,#32260,#32261,
#32262,#32263,#32264,#32265,#32266),.UNSPECIFIED.,.F.,.F.,(4,3,3,3,3,3,
3,3,3,3,3,3,3,3,4),(-60.3586677734892,-60.266413487613,-59.7683439546575,
-59.2702744217021,-58.7722048887466,-58.2741353557911,-57.7760658228356,
-57.2779962898802,-56.7799267569247,-56.2818572239692,-55.7837876910137,
-55.2857181580582,-54.7876486251028,-54.2895790921473,-54.0754824663096),
 .UNSPECIFIED.);
#4812=B_SPLINE_CURVE_WITH_KNOTS('',3,(#32267,#32268,#32269,#32270,#32271,
#32272,#32273,#32274,#32275,#32276,#32277,#32278,#32279,#32280,#32281,#32282,
#32283,#32284,#32285,#32286,#32287,#32288,#32289,#32290,#32291,#32292,#32293,
#32294,#32295,#32296,#32297,#32298,#32299,#32300,#32301,#32302,#32303,#32304,
#32305,#32306,#32307,#32308,#32309),.UNSPECIFIED.,.F.,.F.,(4,3,3,3,3,3,
3,3,3,3,3,3,3,3,4),(51.1026457055681,51.3011618944144,51.7992314273699,
52.2973009603254,52.7953704932809,53.2934400262363,53.7915095591918,54.2895790921473,
54.7876486251028,55.2857181580583,55.7837876910137,56.2818572239692,56.7799267569247,
57.2779962898802,57.3858310127477),.UNSPECIFIED.);
#4813=B_SPLINE_CURVE_WITH_KNOTS('',3,(#32314,#32315,#32316,#32317,#32318,
#32319,#32320,#32321,#32322,#32323,#32324,#32325,#32326,#32327,#32328,#32329,
#32330,#32331,#32332,#32333,#32334,#32335,#32336,#32337,#32338,#32339,#32340,
#32341,#32342,#32343,#32344,#32345,#32346,#32347,#32348,#32349,#32350,#32351,
#32352,#32353),.UNSPECIFIED.,.F.,.F.,(4,3,3,3,3,3,3,3,3,3,3,3,3,4),(-66.6418530806688,
-66.2432478830788,-65.7451783501233,-65.2471088171678,-64.7490392842123,
-64.2509697512569,-63.7529002183014,-63.2548306853459,-62.7567611523904,
-62.2586916194349,-61.7606220864795,-61.262552553524,-60.7644830205685,
-60.3586677734892),.UNSPECIFIED.);
#4814=B_SPLINE_CURVE_WITH_KNOTS('',3,(#32354,#32355,#32356,#32357,#32358,
#32359,#32360,#32361,#32362,#32363,#32364,#32365,#32366,#32367,#32368,#32369,
#32370,#32371,#32372,#32373,#32374,#32375,#32376,#32377,#32378,#32379,#32380,
#32381,#32382,#32383,#32384,#32385,#32386,#32387,#32388,#32389,#32390,#32391,
#32392,#32393),.UNSPECIFIED.,.F.,.F.,(4,3,3,3,3,3,3,3,3,3,3,3,3,4),(57.3858310127477,
57.7760658228356,58.2741353557911,58.7722048887466,59.2702744217021,59.7683439546576,
60.266413487613,60.7644830205685,61.262552553524,61.7606220864795,62.258691619435,
62.7567611523904,63.2548306853459,63.6690163199273),.UNSPECIFIED.);
#4815=B_SPLINE_CURVE_WITH_KNOTS('',3,(#32398,#32399,#32400,#32401,#32402,
#32403,#32404,#32405,#32406,#32407,#32408,#32409,#32410,#32411,#32412,#32413,
#32414,#32415,#32416,#32417,#32418,#32419,#32420,#32421,#32422,#32423,#32424,
#32425,#32426,#32427,#32428,#32429,#32430,#32431,#32432,#32433,#32434,#32435,
#32436,#32437,#32438,#32439,#32440),.UNSPECIFIED.,.F.,.F.,(4,3,3,3,3,3,
3,3,3,3,3,3,3,3,4),(-72.9250383878484,-72.7181518115,-72.2200822785445,
-71.7220127455891,-71.2239432126336,-70.7258736796781,-70.2278041467226,
-69.7297346137671,-69.2316650808116,-68.7335955478562,-68.2355260149007,
-67.7374564819452,-67.2393869489897,-66.7413174160342,-66.6418530806688),
 .UNSPECIFIED.);
#4816=B_SPLINE_CURVE_WITH_KNOTS('',3,(#32441,#32442,#32443,#32444,#32445,
#32446,#32447,#32448,#32449,#32450,#32451,#32452,#32453,#32454,#32455,#32456,
#32457,#32458,#32459,#32460,#32461,#32462,#32463,#32464,#32465,#32466,#32467,
#32468,#32469,#32470,#32471,#32472,#32473,#32474,#32475,#32476,#32477,#32478,
#32479,#32480,#32481,#32482,#32483),.UNSPECIFIED.,.F.,.F.,(4,3,3,3,3,3,
3,3,3,3,3,3,3,3,4),(63.6690163199273,63.7529002183014,64.2509697512569,
64.7490392842124,65.2471088171678,65.7451783501233,66.2432478830788,66.7413174160343,
67.2393869489897,67.7374564819452,68.2355260149007,68.7335955478562,69.2316650808117,
69.7297346137671,69.9522016271069),.UNSPECIFIED.);
#4817=B_SPLINE_CURVE_WITH_KNOTS('',3,(#32488,#32489,#32490,#32491,#32492,
#32493,#32494,#32495,#32496,#32497,#32498,#32499,#32500,#32501,#32502,#32503,
#32504,#32505,#32506,#32507,#32508,#32509,#32510,#32511,#32512,#32513,#32514,
#32515,#32516,#32517,#32518,#32519,#32520,#32521,#32522,#32523,#32524,#32525,
#32526,#32527,#32528,#32529,#32530),.UNSPECIFIED.,.F.,.F.,(4,3,3,3,3,3,
3,3,3,3,3,3,3,3,4),(-79.208223695028,-79.1930557399212,-78.6949862069658,
-78.1969166740103,-77.6988471410548,-77.2007776080993,-76.7027080751438,
-76.2046385421883,-75.7065690092329,-75.2084994762774,-74.7104299433219,
-74.2123604103664,-73.714290877411,-73.2162213444555,-72.9250383878484),
 .UNSPECIFIED.);
#4818=B_SPLINE_CURVE_WITH_KNOTS('',3,(#32531,#32532,#32533,#32534,#32535,
#32536,#32537,#32538,#32539,#32540,#32541,#32542,#32543,#32544,#32545,#32546,
#32547,#32548,#32549,#32550,#32551,#32552,#32553,#32554,#32555,#32556,#32557,
#32558,#32559,#32560,#32561,#32562,#32563,#32564,#32565,#32566,#32567,#32568,
#32569,#32570,#32571,#32572,#32573),.UNSPECIFIED.,.F.,.F.,(4,3,3,3,3,3,
3,3,3,3,3,3,3,3,4),(69.9522016271069,70.2278041467226,70.7258736796781,
71.2239432126336,71.7220127455891,72.2200822785446,72.7181518115,73.2162213444555,
73.714290877411,74.2123604103665,74.7104299433219,75.2084994762774,75.7065690092329,
76.2046385421884,76.2353869342864),.UNSPECIFIED.);
#4819=B_SPLINE_CURVE_WITH_KNOTS('',3,(#32578,#32579,#32580,#32581,#32582,
#32583,#32584,#32585,#32586,#32587,#32588,#32589,#32590,#32591,#32592,#32593,
#32594,#32595,#32596,#32597,#32598,#32599,#32600,#32601,#32602,#32603,#32604,
#32605,#32606,#32607,#32608,#32609,#32610,#32611,#32612,#32613,#32614,#32615,
#32616,#32617),.UNSPECIFIED.,.F.,.F.,(4,3,3,3,3,3,3,3,3,3,3,3,3,4),(-85.4914090022076,
-85.169890135387,-84.6718206024315,-84.1737510694761,-83.6756815365206,
-83.1776120035651,-82.6795424706096,-82.1814729376541,-81.6834034046987,
-81.1853338717432,-80.6872643387877,-80.1891948058322,-79.6911252728767,
-79.208223695028),.UNSPECIFIED.);
#4820=B_SPLINE_CURVE_WITH_KNOTS('',3,(#32618,#32619,#32620,#32621,#32622,
#32623,#32624,#32625,#32626,#32627,#32628,#32629,#32630,#32631,#32632,#32633,
#32634,#32635,#32636,#32637,#32638,#32639,#32640,#32641,#32642,#32643,#32644,
#32645,#32646,#32647,#32648,#32649,#32650,#32651,#32652,#32653,#32654,#32655,
#32656,#32657),.UNSPECIFIED.,.F.,.F.,(4,3,3,3,3,3,3,3,3,3,3,3,3,4),(76.2353869342864,
76.7027080751439,77.2007776080993,77.6988471410548,78.1969166740103,78.6949862069658,
79.1930557399212,79.6911252728767,80.1891948058322,80.6872643387877,81.1853338717432,
81.6834034046987,82.1814729376541,82.5185722414661),.UNSPECIFIED.);
#4821=B_SPLINE_CURVE_WITH_KNOTS('',3,(#32662,#32663,#32664,#32665,#32666,
#32667,#32668,#32669,#32670,#32671,#32672,#32673,#32674,#32675,#32676,#32677,
#32678,#32679,#32680,#32681,#32682,#32683,#32684,#32685,#32686,#32687,#32688,
#32689,#32690,#32691,#32692,#32693,#32694,#32695,#32696,#32697,#32698,#32699,
#32700,#32701,#32702,#32703,#32704),.UNSPECIFIED.,.F.,.F.,(4,3,3,3,3,3,
3,3,3,3,3,3,3,3,4),(-91.7745943093872,-91.6447940638082,-91.1467245308528,
-90.6486549978973,-90.1505854649418,-89.6525159319863,-89.1544463990308,
-88.6563768660754,-88.1583073331199,-87.6602378001644,-87.1621682672089,
-86.6640987342534,-86.166029201298,-85.6679596683425,-85.4914090022076),
 .UNSPECIFIED.);
#4822=B_SPLINE_CURVE_WITH_KNOTS('',3,(#32705,#32706,#32707,#32708,#32709,
#32710,#32711,#32712,#32713,#32714,#32715,#32716,#32717,#32718,#32719,#32720,
#32721,#32722,#32723,#32724,#32725,#32726,#32727,#32728,#32729,#32730,#32731,
#32732,#32733,#32734,#32735,#32736,#32737,#32738,#32739,#32740,#32741,#32742,
#32743,#32744,#32745,#32746,#32747),.UNSPECIFIED.,.F.,.F.,(4,3,3,3,3,3,
3,3,3,3,3,3,3,3,4),(82.5185722414661,82.6795424706096,83.1776120035651,
83.6756815365206,84.1737510694761,84.6718206024316,85.169890135387,85.6679596683425,
86.166029201298,86.6640987342535,87.1621682672089,87.6602378001644,88.1583073331199,
88.6563768660754,88.8017575486456),.UNSPECIFIED.);
#4823=B_SPLINE_CURVE_WITH_KNOTS('',3,(#32752,#32753,#32754,#32755,#32756,
#32757,#32758,#32759,#32760,#32761,#32762,#32763,#32764,#32765,#32766,#32767,
#32768,#32769,#32770,#32771,#32772,#32773,#32774,#32775,#32776,#32777,#32778,
#32779,#32780,#32781,#32782,#32783,#32784,#32785,#32786,#32787,#32788,#32789,
#32790,#32791),.UNSPECIFIED.,.F.,.F.,(4,3,3,3,3,3,3,3,3,3,3,3,3,4),(-98.0577796165668,
-97.621628459274,-97.1235589263185,-96.625489393363,-96.1274198604075,-95.6293503274521,
-95.1312807944966,-94.6332112615411,-94.1351417285857,-93.6370721956302,
-93.1390026626747,-92.6409331297192,-92.1428635967637,-91.7745943093872),
 .UNSPECIFIED.);
#4824=B_SPLINE_CURVE_WITH_KNOTS('',3,(#32792,#32793,#32794,#32795,#32796,
#32797,#32798,#32799,#32800,#32801,#32802,#32803,#32804,#32805,#32806,#32807,
#32808,#32809,#32810,#32811,#32812,#32813,#32814,#32815,#32816,#32817,#32818,
#32819,#32820,#32821,#32822,#32823,#32824,#32825,#32826,#32827,#32828,#32829,
#32830,#32831),.UNSPECIFIED.,.F.,.F.,(4,3,3,3,3,3,3,3,3,3,3,3,3,4),(88.8017575486456,
89.1544463990309,89.6525159319864,90.1505854649418,90.6486549978973,91.1467245308528,
91.6447940638083,92.1428635967637,92.6409331297192,93.1390026626747,93.6370721956302,
94.1351417285857,94.6332112615411,95.0849428558252),.UNSPECIFIED.);
#4825=B_SPLINE_CURVE_WITH_KNOTS('',3,(#32837,#32838,#32839,#32840,#32841,
#32842,#32843,#32844,#32845),.UNSPECIFIED.,.F.,.F.,(4,1,1,1,1,1,4),(109.955742875643,
110.017661251305,110.515730784261,111.013800317216,111.511869850172,112.009939383127,
112.428928173949),.UNSPECIFIED.);
#4826=B_SPLINE_CURVE_WITH_KNOTS('',3,(#32848,#32849,#32850,#32851,#32852,
#32853),.UNSPECIFIED.,.F.,.F.,(4,1,1,4),(109.955742875643,110.193799435556,
110.691868968511,111.189938501467),.UNSPECIFIED.);
#4827=B_SPLINE_CURVE_WITH_KNOTS('',3,(#32858,#32859,#32860,#32861,#32862,
#32863,#32864,#32865,#32866,#32867,#32868,#32869,#32870,#32871,#32872,#32873),
 .UNSPECIFIED.,.F.,.F.,(4,1,1,1,1,1,1,1,1,1,1,1,1,4),(103.672557568463,
104.04082685584,104.538896388795,105.036965921751,105.535035454706,106.033104987662,
106.531174520617,107.029244053573,107.527313586528,108.025383119484,108.523452652439,
109.021522185394,109.51959171835,109.955742875643),.UNSPECIFIED.);
#4828=B_SPLINE_CURVE_WITH_KNOTS('',3,(#32874,#32875,#32876,#32877,#32878,
#32879,#32880,#32881,#32882,#32883,#32884,#32885,#32886,#32887,#32888,#32889,
#32890),.UNSPECIFIED.,.F.,.F.,(4,1,1,1,1,1,1,1,1,1,1,1,1,1,4),(103.672557568463,
103.718895507134,104.21696504009,104.715034573045,105.213104106001,105.711173638956,
106.209243171912,106.707312704867,107.205382237823,107.703451770778,108.201521303734,
108.699590836689,109.197660369645,109.6957299026,109.955742875643),
 .UNSPECIFIED.);
#4829=B_SPLINE_CURVE_WITH_KNOTS('',3,(#32895,#32896,#32897,#32898,#32899,
#32900,#32901,#32902,#32903,#32904,#32905,#32906,#32907,#32908,#32909,#32910,
#32911),.UNSPECIFIED.,.F.,.F.,(4,1,1,1,1,1,1,1,1,1,1,1,1,1,4),(97.3893722612836,
97.5659229274184,98.0639924603739,98.5620619933294,99.0601315262849,99.5582010592404,
100.056270592196,100.554340125151,101.052409658107,101.550479191062,102.048548724018,
102.546618256973,103.044687789929,103.542757322884,103.672557568463),
 .UNSPECIFIED.);
#4830=B_SPLINE_CURVE_WITH_KNOTS('',3,(#32912,#32913,#32914,#32915,#32916,
#32917,#32918,#32919,#32920,#32921,#32922,#32923,#32924,#32925,#32926,#32927),
 .UNSPECIFIED.,.F.,.F.,(4,1,1,1,1,1,1,1,1,1,1,1,1,4),(97.3893722612836,
97.7420611116687,98.2401306446242,98.7382001775796,99.2362697105351,99.7343392434906,
100.232408776446,100.730478309402,101.228547842357,101.726617375313,102.224686908268,
102.722756441223,103.220825974179,103.672557568463),.UNSPECIFIED.);
#4831=B_SPLINE_CURVE_WITH_KNOTS('',3,(#32932,#32933,#32934,#32935,#32936,
#32937,#32938,#32939,#32940,#32941,#32942,#32943,#32944,#32945,#32946,#32947),
 .UNSPECIFIED.,.F.,.F.,(4,1,1,1,1,1,1,1,1,1,1,1,1,4),(91.106186954104,91.5890885319527,
92.0871580649082,92.5852275978636,93.0832971308191,93.5813666637746,94.0794361967301,
94.5775057296856,95.0755752626411,95.5736447955965,96.071714328552,96.5697838615075,
97.067853394463,97.3893722612836),.UNSPECIFIED.);
#4832=B_SPLINE_CURVE_WITH_KNOTS('',3,(#32948,#32949,#32950,#32951,#32952,
#32953,#32954,#32955,#32956,#32957,#32958,#32959,#32960,#32961,#32962,#32963,
#32964),.UNSPECIFIED.,.F.,.F.,(4,1,1,1,1,1,1,1,1,1,1,1,1,1,4),(91.106186954104,
91.2671571832475,91.7652267162029,92.2632962491584,92.7613657821139,93.2594353150694,
93.7575048480249,94.2555743809803,94.7536439139358,95.2517134468913,95.7497829798468,
96.2478525128023,96.7459220457577,97.2439915787132,97.3893722612836),
 .UNSPECIFIED.);
#4833=B_SPLINE_CURVE_WITH_KNOTS('',3,(#32969,#32970,#32971,#32972,#32973,
#32974,#32975,#32976,#32977,#32978,#32979,#32980,#32981,#32982,#32983,#32984,
#32985),.UNSPECIFIED.,.F.,.F.,(4,1,1,1,1,1,1,1,1,1,1,1,1,1,4),(84.8230016469244,
85.1141846035315,85.6122541364869,86.1103236694424,86.6083932023979,87.1064627353534,
87.6045322683088,88.1026018012643,88.6006713342198,89.0987408671753,89.5968104001308,
90.0948799330862,90.5929494660417,91.0910189989972,91.106186954104),
 .UNSPECIFIED.);
#4834=B_SPLINE_CURVE_WITH_KNOTS('',3,(#32986,#32987,#32988,#32989,#32990,
#32991,#32992,#32993,#32994,#32995,#32996,#32997,#32998,#32999,#33000,#33001),
 .UNSPECIFIED.,.F.,.F.,(4,1,1,1,1,1,1,1,1,1,1,1,1,4),(84.8230016469244,
85.2903227877817,85.7883923207372,86.2864618536927,86.7845313866481,87.2826009196036,
87.7806704525591,88.2787399855146,88.7768095184701,89.2748790514255,89.772948584381,
90.2710181173365,90.769087650292,91.106186954104),.UNSPECIFIED.);
#4835=B_SPLINE_CURVE_WITH_KNOTS('',3,(#33006,#33007,#33008,#33009,#33010,
#33011,#33012,#33013,#33014,#33015,#33016,#33017,#33018,#33019,#33020,#33021,
#33022),.UNSPECIFIED.,.F.,.F.,(4,1,1,1,1,1,1,1,1,1,1,1,1,1,4),(78.5398163397448,
78.6392806751102,79.1373502080657,79.6354197410212,80.1334892739767,80.6315588069321,
81.1296283398876,81.6276978728431,82.1257674057986,82.6238369387541,83.1219064717095,
83.619976004665,84.1180455376205,84.616115070576,84.8230016469244),
 .UNSPECIFIED.);
#4836=B_SPLINE_CURVE_WITH_KNOTS('',3,(#33023,#33024,#33025,#33026,#33027,
#33028,#33029,#33030,#33031,#33032,#33033,#33034,#33035,#33036,#33037,#33038,
#33039),.UNSPECIFIED.,.F.,.F.,(4,1,1,1,1,1,1,1,1,1,1,1,1,1,4),(78.5398163397448,
78.8154188593605,79.3134883923159,79.8115579252714,80.3096274582269,80.8076969911824,
81.3057665241379,81.8038360570933,82.3019055900488,82.7999751230043,83.2980446559598,
83.7961141889153,84.2941837218707,84.7922532548262,84.8230016469244),
 .UNSPECIFIED.);
#4837=B_SPLINE_CURVE_WITH_KNOTS('',3,(#33044,#33045,#33046,#33047,#33048,
#33049,#33050,#33051,#33052,#33053,#33054,#33055,#33056,#33057,#33058,#33059),
 .UNSPECIFIED.,.F.,.F.,(4,1,1,1,1,1,1,1,1,1,1,1,1,4),(72.2566310325652,
72.6624462796445,73.1605158125999,73.6585853455554,74.1566548785109,74.6547244114664,
75.1527939444219,75.6508634773773,76.1489330103328,76.6470025432883,77.1450720762438,
77.6431416091993,78.1412111421547,78.5398163397448),.UNSPECIFIED.);
#4838=B_SPLINE_CURVE_WITH_KNOTS('',3,(#33060,#33061,#33062,#33063,#33064,
#33065,#33066,#33067,#33068,#33069,#33070,#33071,#33072,#33073,#33074,#33075,
#33076),.UNSPECIFIED.,.F.,.F.,(4,1,1,1,1,1,1,1,1,1,1,1,1,1,4),(72.2566310325652,
72.3405149309392,72.8385844638947,73.3366539968502,73.8347235298057,74.3327930627611,
74.8308625957166,75.3289321286721,75.8270016616276,76.3250711945831,76.8231407275385,
77.321210260494,77.8192797934495,78.317349326405,78.5398163397448),
 .UNSPECIFIED.);
#4839=B_SPLINE_CURVE_WITH_KNOTS('',3,(#33081,#33082,#33083,#33084,#33085,
#33086,#33087,#33088,#33089,#33090,#33091,#33092,#33093,#33094,#33095,#33096,
#33097),.UNSPECIFIED.,.F.,.F.,(4,1,1,1,1,1,1,1,1,1,1,1,1,1,4),(65.9734457253856,
66.1875423512232,66.6856118841787,67.1836814171342,67.6817509500897,68.1798204830451,
68.6778900160006,69.1759595489561,69.6740290819116,70.1720986148671,70.6701681478225,
71.168237680778,71.6663072137335,72.164376746689,72.2566310325652),
 .UNSPECIFIED.);
#4840=B_SPLINE_CURVE_WITH_KNOTS('',3,(#33098,#33099,#33100,#33101,#33102,
#33103,#33104,#33105,#33106,#33107,#33108,#33109,#33110,#33111,#33112,#33113),
 .UNSPECIFIED.,.F.,.F.,(4,1,1,1,1,1,1,1,1,1,1,1,1,4),(65.9734457253856,
66.3636805354735,66.861750068429,67.3598196013844,67.8578891343399,68.3559586672954,
68.8540282002509,69.3520977332063,69.8501672661618,70.3482367991173,70.8463063320728,
71.3443758650283,71.8424453979838,72.2566310325652),.UNSPECIFIED.);
#4841=B_SPLINE_CURVE_WITH_KNOTS('',3,(#33118,#33119,#33120,#33121,#33122,
#33123,#33124,#33125,#33126,#33127,#33128,#33129,#33130,#33131,#33132,#33133,
#33134),.UNSPECIFIED.,.F.,.F.,(4,1,1,1,1,1,1,1,1,1,1,1,1,1,4),(59.690260418206,
59.712638422802,60.2107079557575,60.708777488713,61.2068470216684,61.7049165546239,
62.2029860875794,62.7010556205349,63.1991251534903,63.6971946864458,64.1952642194013,
64.6933337523568,65.1914032853123,65.6894728182677,65.9734457253856),
 .UNSPECIFIED.);
#4842=B_SPLINE_CURVE_WITH_KNOTS('',3,(#33135,#33136,#33137,#33138,#33139,
#33140,#33141,#33142,#33143,#33144,#33145,#33146,#33147,#33148,#33149,#33150,
#33151),.UNSPECIFIED.,.F.,.F.,(4,1,1,1,1,1,1,1,1,1,1,1,1,1,4),(59.690260418206,
59.8887766070523,60.3868461400077,60.8849156729632,61.3829852059187,61.8810547388742,
62.3791242718296,62.8771938047851,63.3752633377406,63.8733328706961,64.3714024036516,
64.869471936607,65.3675414695625,65.865611002518,65.9734457253856),
 .UNSPECIFIED.);
#4843=B_SPLINE_CURVE_WITH_KNOTS('',3,(#33156,#33157,#33158,#33159,#33160,
#33161,#33162,#33163,#33164,#33165,#33166,#33167,#33168,#33169,#33170,#33171),
 .UNSPECIFIED.,.F.,.F.,(4,1,1,1,1,1,1,1,1,1,1,1,1,4),(53.4070751110264,
53.7358040273362,54.2338735602917,54.7319430932472,55.2300126262027,55.7280821591582,
56.2261516921136,56.7242212250691,57.2222907580246,57.7203602909801,58.2184298239356,
58.716499356891,59.2145688898465,59.690260418206),.UNSPECIFIED.);
#4844=B_SPLINE_CURVE_WITH_KNOTS('',3,(#33172,#33173,#33174,#33175,#33176,
#33177,#33178,#33179,#33180,#33181,#33182,#33183,#33184,#33185,#33186,#33187,
#33188),.UNSPECIFIED.,.F.,.F.,(4,1,1,1,1,1,1,1,1,1,1,1,1,1,4),(53.4070751110264,
53.413872678631,53.9119422115865,54.410011744542,54.9080812774974,55.4061508104529,
55.9042203434084,56.4022898763639,56.9003594093194,57.3984289422748,57.8964984752303,
58.3945680081858,58.8926375411413,59.3907070740968,59.690260418206),
 .UNSPECIFIED.);
#4845=B_SPLINE_CURVE_WITH_KNOTS('',3,(#33193,#33194,#33195,#33196,#33197,
#33198,#33199,#33200,#33201,#33202,#33203,#33204,#33205,#33206,#33207,#33208,
#33209),.UNSPECIFIED.,.F.,.F.,(4,1,1,1,1,1,1,1,1,1,1,1,1,1,4),(47.1238898038469,
47.260900098915,47.7589696318705,48.257039164826,48.7551086977815,49.2531782307369,
49.7512477636924,50.2493172966479,50.7473868296034,51.2454563625588,51.7435258955143,
52.2415954284698,52.7396649614253,53.2377344943808,53.4070751110264),
 .UNSPECIFIED.);
#4846=B_SPLINE_CURVE_WITH_KNOTS('',3,(#33210,#33211,#33212,#33213,#33214,
#33215,#33216,#33217,#33218,#33219,#33220,#33221,#33222,#33223,#33224,#33225),
 .UNSPECIFIED.,.F.,.F.,(4,1,1,1,1,1,1,1,1,1,1,1,1,4),(47.1238898038468,
47.4370382831653,47.9351078161207,48.4331773490762,48.9312468820317,49.4293164149872,
49.9273859479427,50.4254554808981,50.9235250138536,51.4215945468091,51.9196640797646,
52.41773361272,52.9158031456755,53.4070751110264),.UNSPECIFIED.);
#4847=B_SPLINE_CURVE_WITH_KNOTS('',3,(#33230,#33231,#33232,#33233,#33234,
#33235,#33236,#33237,#33238,#33239,#33240,#33241,#33242,#33243,#33244,#33245),
 .UNSPECIFIED.,.F.,.F.,(4,1,1,1,1,1,1,1,1,1,1,1,1,4),(40.8407044966672,
41.2840657034493,41.7821352364047,42.2802047693602,42.7782743023157,43.2763438352712,
43.7744133682266,44.2724829011821,44.7705524341376,45.2686219670931,45.7666915000486,
46.264761033004,46.7628305659595,47.1238898038469),.UNSPECIFIED.);
#4848=B_SPLINE_CURVE_WITH_KNOTS('',3,(#33246,#33247,#33248,#33249,#33250,
#33251,#33252,#33253,#33254,#33255,#33256,#33257,#33258,#33259,#33260,#33261,
#33262),.UNSPECIFIED.,.F.,.F.,(4,1,1,1,1,1,1,1,1,1,1,1,1,1,4),(40.8407044966672,
40.962134354744,41.4602038876995,41.958273420655,42.4563429536105,42.9544124865659,
43.4524820195214,43.9505515524769,44.4486210854324,44.9466906183878,45.4447601513433,
45.9428296842988,46.4408992172543,46.9389687502098,47.1238898038468),
 .UNSPECIFIED.);
#4849=B_SPLINE_CURVE_WITH_KNOTS('',3,(#33267,#33268,#33269,#33270,#33271,
#33272,#33273,#33274,#33275,#33276,#33277,#33278,#33279,#33280,#33281,#33282,
#33283),.UNSPECIFIED.,.F.,.F.,(4,1,1,1,1,1,1,1,1,1,1,1,1,1,4),(34.5575191894876,
34.809161775028,35.3072313079835,35.805300840939,36.3033703738945,36.8014399068499,
37.2995094398054,37.7975789727609,38.2956485057164,38.7937180386719,39.2917875716273,
39.7898571045828,40.2879266375383,40.7859961704938,40.8407044966672),
 .UNSPECIFIED.);
#4850=B_SPLINE_CURVE_WITH_KNOTS('',3,(#33284,#33285,#33286,#33287,#33288,
#33289,#33290,#33291,#33292,#33293,#33294,#33295,#33296,#33297,#33298,#33299),
 .UNSPECIFIED.,.F.,.F.,(4,1,1,1,1,1,1,1,1,1,1,1,1,4),(34.5575191894876,
34.9852999592783,35.4833694922337,35.9814390251892,36.4795085581447,36.9775780911002,
37.4756476240557,37.9737171570111,38.4717866899666,38.9698562229221,39.4679257558776,
39.9659952888331,40.4640648217885,40.8407044966672),.UNSPECIFIED.);
#4851=B_SPLINE_CURVE_WITH_KNOTS('',3,(#33304,#33305,#33306,#33307,#33308,
#33309,#33310,#33311,#33312,#33313,#33314,#33315,#33316,#33317,#33318,#33319,
#33320),.UNSPECIFIED.,.F.,.F.,(4,1,1,1,1,1,1,1,1,1,1,1,1,1,4),(28.2743338823081,
28.3342578466068,28.8323273795623,29.3303969125177,29.8284664454732,30.3265359784287,
30.8246055113842,31.3226750443397,31.8207445772951,32.3188141102506,32.8168836432061,
33.3149531761616,33.8130227091171,34.3110922420725,34.5575191894876),
 .UNSPECIFIED.);
#4852=B_SPLINE_CURVE_WITH_KNOTS('',3,(#33321,#33322,#33323,#33324,#33325,
#33326,#33327,#33328,#33329,#33330,#33331,#33332,#33333,#33334,#33335,#33336,
#33337),.UNSPECIFIED.,.F.,.F.,(4,1,1,1,1,1,1,1,1,1,1,1,1,1,4),(28.274333882308,
28.510396030857,29.0084655638125,29.506535096768,30.0046046297235,30.5026741626789,
31.0007436956344,31.4988132285899,31.9968827615454,32.4949522945009,32.9930218274563,
33.4910913604118,33.9891608933673,34.4872304263228,34.5575191894876),
 .UNSPECIFIED.);
#4853=B_SPLINE_CURVE_WITH_KNOTS('',3,(#33342,#33343,#33344,#33345,#33346,
#33347,#33348,#33349,#33350,#33351,#33352,#33353,#33354,#33355,#33356,#33357),
 .UNSPECIFIED.,.F.,.F.,(4,1,1,1,1,1,1,1,1,1,1,1,1,4),(21.9911485751285,
22.357423451141,22.8554929840965,23.353562517052,23.8516320500075,24.349701582963,
24.8477711159184,25.3458406488739,25.8439101818294,26.3419797147849,26.8400492477403,
27.3381187806958,27.8361883136513,28.2743338823081),.UNSPECIFIED.);
#4854=B_SPLINE_CURVE_WITH_KNOTS('',3,(#33358,#33359,#33360,#33361,#33362,
#33363,#33364,#33365,#33366,#33367,#33368,#33369,#33370,#33371,#33372,#33373,
#33374),.UNSPECIFIED.,.F.,.F.,(4,1,1,1,1,1,1,1,1,1,1,1,1,1,4),(21.9911485751285,
22.0354921024358,22.5335616353913,23.0316311683467,23.5297007013022,24.0277702342577,
24.5258397672132,25.0239093001687,25.5219788331241,26.0200483660796,26.5181178990351,
27.0161874319906,27.5142569649461,28.0123264979015,28.274333882308),
 .UNSPECIFIED.);
#4855=B_SPLINE_CURVE_WITH_KNOTS('',3,(#33379,#33380,#33381,#33382,#33383,
#33384,#33385,#33386,#33387,#33388,#33389,#33390,#33391,#33392,#33393,#33394,
#33395),.UNSPECIFIED.,.F.,.F.,(4,1,1,1,1,1,1,1,1,1,1,1,1,1,4),(15.7079632679489,
15.8825195227198,16.3805890556753,16.8786585886308,17.3767281215862,17.8747976545417,
18.3728671874972,18.8709367204527,19.3690062534082,19.8670757863636,20.3651453193191,
20.8632148522746,21.3612843852301,21.8593539181856,21.9911485751285),
 .UNSPECIFIED.);
#4856=B_SPLINE_CURVE_WITH_KNOTS('',3,(#33396,#33397,#33398,#33399,#33400,
#33401,#33402,#33403,#33404,#33405,#33406,#33407,#33408,#33409,#33410,#33411),
 .UNSPECIFIED.,.F.,.F.,(4,1,1,1,1,1,1,1,1,1,1,1,1,4),(15.7079632679489,
16.05865770697,16.5567272399255,17.054796772881,17.5528663058365,18.0509358387919,
18.5490053717474,19.0470749047029,19.5451444376584,20.0432139706139,20.5412835035693,
21.0393530365248,21.5374225694803,21.9911485751285),.UNSPECIFIED.);
#4857=B_SPLINE_CURVE_WITH_KNOTS('',3,(#33417,#33418,#33419,#33420,#33421,
#33422,#33423),.UNSPECIFIED.,.F.,.F.,(4,3,4),(405.265452313083,405.559874952706,
406.482000549955),.UNSPECIFIED.);
#4858=B_SPLINE_CURVE_WITH_KNOTS('',3,(#33429,#33430,#33431,#33432,#33433,
#33434,#33435,#33436,#33437,#33438,#33439,#33440),.UNSPECIFIED.,.F.,.F.,
(4,1,1,1,1,1,1,1,1,4),(398.982267005904,399.572906010296,400.570734167364,
401.568562324433,402.067476402967,402.566390481501,403.065304560035,403.564218638569,
404.562046795637,405.265452313083),.UNSPECIFIED.);
#4859=B_SPLINE_CURVE_WITH_KNOTS('',3,(#33443,#33444,#33445,#33446,#33447,
#33448,#33449,#33450,#33451,#33452,#33453,#33454,#33455),.UNSPECIFIED.,
 .F.,.F.,(4,1,1,1,1,1,1,1,1,1,4),(398.982267005904,399.256041935063,399.754956013597,
400.253870092131,401.251698249199,402.249526406267,403.247354563336,403.74626864187,
404.245182720404,404.744096798938,405.243010877472),.UNSPECIFIED.);
#4860=B_SPLINE_CURVE_WITH_KNOTS('',3,(#33460,#33461,#33462,#33463,#33464,
#33465,#33466,#33467,#33468,#33469,#33470,#33471),.UNSPECIFIED.,.F.,.F.,
(4,1,1,1,1,1,1,1,1,4),(392.699081698724,393.585937067887,394.583765224955,
395.082679303489,395.581593382023,396.080507460557,396.579421539091,397.57724969616,
398.575077853228,398.982267005904),.UNSPECIFIED.);
#4861=B_SPLINE_CURVE_WITH_KNOTS('',3,(#33472,#33473,#33474,#33475,#33476,
#33477,#33478,#33479,#33480,#33481,#33482,#33483),.UNSPECIFIED.,.F.,.F.,
(4,1,1,1,1,1,1,1,1,4),(392.699081698724,392.770158914119,393.269072992653,
394.266901149721,395.26472930679,396.262557463858,397.260385620926,398.258213777994,
398.757127856529,398.982267005904),.UNSPECIFIED.);
#4862=B_SPLINE_CURVE_WITH_KNOTS('',3,(#33488,#33489,#33490,#33491,#33492,
#33493,#33494,#33495,#33496,#33497,#33498,#33499,#33500),.UNSPECIFIED.,
 .F.,.F.,(4,1,1,1,1,1,1,1,1,1,4),(386.415896391544,386.601139968409,387.598968125477,
388.097882204011,388.596796282545,389.095710361079,389.594624439613,390.592452596682,
391.59028075375,392.588108910818,392.699081698724),.UNSPECIFIED.);
#4863=B_SPLINE_CURVE_WITH_KNOTS('',3,(#33501,#33502,#33503,#33504,#33505,
#33506,#33507,#33508,#33509,#33510,#33511),.UNSPECIFIED.,.F.,.F.,(4,1,1,
1,1,1,1,1,4),(386.415896391545,387.282104050244,388.279932207312,389.27776036438,
390.275588521448,391.273416678517,391.772330757051,392.271244835585,392.699081698724),
 .UNSPECIFIED.);
#4864=B_SPLINE_CURVE_WITH_KNOTS('',3,(#33516,#33517,#33518,#33519,#33520,
#33521,#33522,#33523,#33524,#33525,#33526,#33527),.UNSPECIFIED.,.F.,.F.,
(4,1,1,1,1,1,1,1,1,4),(380.132711084365,380.614171025999,381.113085104533,
381.611999183067,382.110913261602,382.609827340136,383.607655497204,384.605483654272,
385.60331181134,386.415896391544),.UNSPECIFIED.);
#4865=B_SPLINE_CURVE_WITH_KNOTS('',3,(#33528,#33529,#33530,#33531,#33532,
#33533,#33534,#33535,#33536,#33537,#33538,#33539,#33540,#33541,#33542,#33543,
#33544,#33545,#33546,#33547,#33548,#33549,#33550,#33551,#33552),
 .UNSPECIFIED.,.F.,.F.,(4,3,3,3,3,3,3,3,4),(380.132711084365,381.019390447226,
381.906069810087,382.792749172948,383.679428535808,384.566107898669,385.45278726153,
386.339466624391,386.415896391545),.UNSPECIFIED.);
#4866=B_SPLINE_CURVE_WITH_KNOTS('',3,(#33557,#33558,#33559,#33560,#33561,
#33562,#33563,#33564,#33565,#33566,#33567,#33568,#33569,#33570,#33571,#33572,
#33573,#33574,#33575,#33576,#33577,#33578,#33579,#33580,#33581),
 .UNSPECIFIED.,.F.,.F.,(4,3,3,3,3,3,3,3,4),(373.849525777185,374.736205140046,
375.622884502907,376.509563865768,377.396243228629,378.28292259149,379.16960195435,
380.056281317211,380.132711084365),.UNSPECIFIED.);
#4867=B_SPLINE_CURVE_WITH_KNOTS('',3,(#33582,#33583,#33584,#33585,#33586,
#33587,#33588,#33589,#33590,#33591,#33592,#33593),.UNSPECIFIED.,.F.,.F.,
(4,1,1,1,1,1,1,1,1,4),(373.849525777185,374.310338008356,375.308166165424,
376.305994322493,377.303822479561,377.802736558095,378.301650636629,378.800564715163,
379.299478793698,380.132711084365),.UNSPECIFIED.);
#4868=B_SPLINE_CURVE_WITH_KNOTS('',3,(#33598,#33599,#33600,#33601,#33602,
#33603,#33604,#33605,#33606,#33607,#33608,#33609),.UNSPECIFIED.,.F.,.F.,
(4,1,1,1,1,1,1,1,1,4),(367.566340470006,367.642404984112,368.141319062646,
368.64023314118,369.638061298248,370.635889455317,371.633717612385,372.631545769453,
373.629373926521,373.849525777185),.UNSPECIFIED.);
#4869=B_SPLINE_CURVE_WITH_KNOTS('',3,(#33610,#33611,#33612,#33613,#33614,
#33615,#33616,#33617,#33618,#33619,#33620,#33621),.UNSPECIFIED.,.F.,.F.,
(4,1,1,1,1,1,1,1,1,4),(367.566340470006,368.323369065947,369.321197223015,
370.319025380083,370.817939458617,371.316853537151,371.815767615686,372.31468169422,
373.312509851288,373.849525777185),.UNSPECIFIED.);
#4870=B_SPLINE_CURVE_WITH_KNOTS('',3,(#33626,#33627,#33628,#33629,#33630,
#33631,#33632,#33633,#33634,#33635,#33636),.UNSPECIFIED.,.F.,.F.,(4,1,1,
1,1,1,1,1,4),(361.283155162826,361.655436041702,362.653264198771,363.651092355839,
364.648920512907,365.646748669975,366.644576827044,367.143490905578,367.566340470006),
 .UNSPECIFIED.);
#4871=B_SPLINE_CURVE_WITH_KNOTS('',3,(#33637,#33638,#33639,#33640,#33641,
#33642,#33643,#33644,#33645,#33646,#33647,#33648,#33649),.UNSPECIFIED.,
 .F.,.F.,(4,1,1,1,1,1,1,1,1,1,4),(361.283155162826,361.338571966469,362.336400123537,
363.334228280605,363.83314235914,364.332056437674,364.830970516208,365.329884594742,
366.32771275181,367.325540908878,367.566340470006),.UNSPECIFIED.);
#4872=B_SPLINE_CURVE_WITH_KNOTS('',3,(#33654,#33655,#33656,#33657,#33658,
#33659,#33660,#33661,#33662,#33663,#33664,#33665,#33666,#33667,#33668,#33669,
#33670,#33671,#33672,#33673,#33674,#33675,#33676,#33677,#33678),
 .UNSPECIFIED.,.F.,.F.,(4,3,3,3,3,3,3,3,4),(354.999969855647,355.886649218508,
356.773328581368,357.660007944229,358.54668730709,359.433366669951,360.320046032812,
361.206725395673,361.283155162826),.UNSPECIFIED.);
#4873=B_SPLINE_CURVE_WITH_KNOTS('',3,(#33679,#33680,#33681,#33682,#33683,
#33684,#33685,#33686,#33687,#33688,#33689,#33690),.UNSPECIFIED.,.F.,.F.,
(4,1,1,1,1,1,1,1,1,4),(354.999969855647,355.351603024059,356.349431181128,
356.848345259662,357.347259338196,357.84617341673,358.345087495264,359.342915652332,
360.340743809401,361.283155162826),.UNSPECIFIED.);
#4874=B_SPLINE_CURVE_WITH_KNOTS('',3,(#33695,#33696,#33697,#33698,#33699,
#33700,#33701,#33702,#33703,#33704,#33705,#33706),.UNSPECIFIED.,.F.,.F.,
(4,1,1,1,1,1,1,1,1,4),(348.716784548467,349.681498156883,350.679326313951,
351.67715447102,352.674982628088,353.173896706622,353.672810785156,354.17172486369,
354.670638942224,354.999969855647),.UNSPECIFIED.);
#4875=B_SPLINE_CURVE_WITH_KNOTS('',3,(#33707,#33708,#33709,#33710,#33711,
#33712,#33713,#33714,#33715,#33716,#33717,#33718,#33719,#33720,#33721,#33722,
#33723,#33724,#33725,#33726,#33727,#33728,#33729,#33730,#33731),
 .UNSPECIFIED.,.F.,.F.,(4,3,3,3,3,3,3,3,4),(348.716784548467,349.603463911328,
350.490143274189,351.37682263705,352.26350199991,353.150181362771,354.036860725632,
354.923540088493,354.999969855647),.UNSPECIFIED.);
#4876=B_SPLINE_CURVE_WITH_KNOTS('',3,(#33736,#33737,#33738,#33739,#33740,
#33741,#33742,#33743,#33744,#33745,#33746,#33747,#33748),.UNSPECIFIED.,
 .F.,.F.,(4,1,1,1,1,1,1,1,1,1,4),(342.433599241288,342.696701057405,343.694529214474,
344.692357371542,345.69018552861,346.189099607144,346.688013685678,347.186927764213,
347.685841842747,348.683669999815,348.716784548467),.UNSPECIFIED.);
#4877=B_SPLINE_CURVE_WITH_KNOTS('',3,(#33749,#33750,#33751,#33752,#33753,
#33754,#33755,#33756,#33757,#33758,#33759,#33760),.UNSPECIFIED.,.F.,.F.,
(4,1,1,1,1,1,1,1,1,4),(342.433599241288,342.878751060706,343.37766513924,
343.876579217774,344.375493296308,345.373321453377,346.371149610445,347.368977767513,
348.366805924582,348.716784548467),.UNSPECIFIED.);
#4878=B_SPLINE_CURVE_WITH_KNOTS('',3,(#33765,#33766,#33767,#33768,#33769,
#33770,#33771,#33772,#33773,#33774,#33775,#33776),.UNSPECIFIED.,.F.,.F.,
(4,1,1,1,1,1,1,1,1,4),(336.150413934108,336.709732114996,337.707560272064,
338.705388429132,339.204302507666,339.703216586201,340.202130664735,340.701044743269,
341.698872900337,342.433599241288),.UNSPECIFIED.);
#4879=B_SPLINE_CURVE_WITH_KNOTS('',3,(#33777,#33778,#33779,#33780,#33781,
#33782,#33783,#33784,#33785,#33786,#33787,#33788),.UNSPECIFIED.,.F.,.F.,
(4,1,1,1,1,1,1,1,1,4),(336.150413934108,336.392868039762,336.891782118297,
337.390696196831,338.388524353899,339.386352510967,340.384180668035,341.382008825104,
342.379836982172,342.433599241288),.UNSPECIFIED.);
#4880=B_SPLINE_CURVE_WITH_KNOTS('',3,(#33793,#33794,#33795,#33796,#33797,
#33798,#33799,#33800,#33801,#33802,#33803,#33804),.UNSPECIFIED.,.F.,.F.,
(4,1,1,1,1,1,1,1,1,4),(329.867228626928,330.722763172586,331.720591329655,
332.219505408189,332.718419486723,333.217333565257,333.716247643791,334.714075800859,
335.711903957928,336.150413934108),.UNSPECIFIED.);
#4881=B_SPLINE_CURVE_WITH_KNOTS('',3,(#33805,#33806,#33807,#33808,#33809,
#33810,#33811,#33812,#33813,#33814,#33815,#33816),.UNSPECIFIED.,.F.,.F.,
(4,1,1,1,1,1,1,1,1,4),(329.867228626929,329.906985018819,330.405899097353,
331.403727254421,332.401555411489,333.399383568558,334.397211725626,335.395039882694,
335.893953961228,336.150413934108),.UNSPECIFIED.);
#4882=B_SPLINE_CURVE_WITH_KNOTS('',3,(#33821,#33822,#33823,#33824,#33825,
#33826,#33827,#33828,#33829,#33830,#33831,#33832,#33833),.UNSPECIFIED.,
 .F.,.F.,(4,1,1,1,1,1,1,1,1,1,4),(323.584043319749,323.737966073108,324.735794230177,
325.234708308711,325.733622387245,326.232536465779,326.731450544313,327.729278701381,
328.72710685845,329.724935015518,329.867228626928),.UNSPECIFIED.);
#4883=B_SPLINE_CURVE_WITH_KNOTS('',3,(#33834,#33835,#33836,#33837,#33838,
#33839,#33840,#33841,#33842,#33843,#33844),.UNSPECIFIED.,.F.,.F.,(4,1,1,
1,1,1,1,1,4),(323.584043319749,324.418930154943,325.416758312012,326.41458646908,
327.412414626148,328.410242783216,328.90915686175,329.408070940285,329.867228626929),
 .UNSPECIFIED.);
#4884=B_SPLINE_CURVE_WITH_KNOTS('',3,(#33849,#33850,#33851,#33852,#33853,
#33854,#33855,#33856,#33857,#33858,#33859,#33860),.UNSPECIFIED.,.F.,.F.,
(4,1,1,1,1,1,1,1,1,4),(317.300858012569,317.750997130699,318.249911209233,
318.748825287767,319.247739366301,319.746653444835,320.744481601904,321.742309758972,
322.74013791604,323.584043319749),.UNSPECIFIED.);
#4885=B_SPLINE_CURVE_WITH_KNOTS('',3,(#33861,#33862,#33863,#33864,#33865,
#33866,#33867,#33868,#33869,#33870,#33871,#33872,#33873,#33874,#33875,#33876,
#33877,#33878,#33879,#33880,#33881,#33882,#33883,#33884,#33885),
 .UNSPECIFIED.,.F.,.F.,(4,3,3,3,3,3,3,3,4),(317.300858012569,318.18753737543,
319.074216738291,319.960896101152,320.847575464013,321.734254826873,322.620934189734,
323.507613552595,323.584043319749),.UNSPECIFIED.);
#4886=B_SPLINE_CURVE_WITH_KNOTS('',3,(#33890,#33891,#33892,#33893,#33894,
#33895,#33896,#33897,#33898,#33899,#33900,#33901,#33902,#33903,#33904,#33905,
#33906,#33907,#33908,#33909,#33910,#33911,#33912,#33913,#33914),
 .UNSPECIFIED.,.F.,.F.,(4,3,3,3,3,3,3,3,4),(311.01767270539,311.90435206825,
312.791031431111,313.677710793972,314.564390156833,315.451069519694,316.337748882555,
317.224428245415,317.300858012569),.UNSPECIFIED.);
#4887=B_SPLINE_CURVE_WITH_KNOTS('',3,(#33915,#33916,#33917,#33918,#33919,
#33920,#33921,#33922,#33923,#33924,#33925,#33926),.UNSPECIFIED.,.F.,.F.,
(4,1,1,1,1,1,1,1,1,4),(311.01767270539,311.447164113056,312.444992270124,
313.442820427192,314.440648584261,314.939562662795,315.438476741329,315.937390819863,
316.436304898397,317.300858012569),.UNSPECIFIED.);
#4888=B_SPLINE_CURVE_WITH_KNOTS('',3,(#33931,#33932,#33933,#33934,#33935,
#33936,#33937,#33938,#33939,#33940,#33941,#33942),.UNSPECIFIED.,.F.,.F.,
(4,1,1,1,1,1,1,1,1,4),(304.73448739821,304.779231088812,305.278145167346,
305.77705924588,306.774887402948,307.772715560016,308.770543717085,309.768371874153,
310.766200031221,311.01767270539),.UNSPECIFIED.);
#4889=B_SPLINE_CURVE_WITH_KNOTS('',3,(#33943,#33944,#33945,#33946,#33947,
#33948,#33949,#33950,#33951,#33952,#33953,#33954),.UNSPECIFIED.,.F.,.F.,
(4,1,1,1,1,1,1,1,1,4),(304.73448739821,305.460195170646,306.458023327715,
307.455851484783,307.954765563317,308.453679641851,308.952593720385,309.451507798919,
310.449335955988,311.01767270539),.UNSPECIFIED.);
#4890=B_SPLINE_CURVE_WITH_KNOTS('',3,(#33959,#33960,#33961,#33962,#33963,
#33964,#33965,#33966,#33967,#33968,#33969),.UNSPECIFIED.,.F.,.F.,(4,1,1,
1,1,1,1,1,4),(298.451302091031,298.792262146402,299.79009030347,300.787918460539,
301.785746617607,302.783574774675,303.781402931743,304.280317010277,304.73448739821),
 .UNSPECIFIED.);
#4891=B_SPLINE_CURVE_WITH_KNOTS('',3,(#33970,#33971,#33972,#33973,#33974,
#33975,#33976,#33977,#33978,#33979,#33980,#33981,#33982),.UNSPECIFIED.,
 .F.,.F.,(4,1,1,1,1,1,1,1,1,1,4),(298.451302091031,298.475398071169,299.473226228237,
300.471054385305,300.969968463839,301.468882542373,301.967796620908,302.466710699442,
303.46453885651,304.462367013578,304.73448739821),.UNSPECIFIED.);
#4892=B_SPLINE_CURVE_WITH_KNOTS('',3,(#33987,#33988,#33989,#33990,#33991,
#33992,#33993,#33994,#33995,#33996,#33997,#33998,#33999,#34000,#34001,#34002,
#34003,#34004,#34005,#34006,#34007,#34008,#34009,#34010,#34011),
 .UNSPECIFIED.,.F.,.F.,(4,3,3,3,3,3,3,3,4),(292.168116783851,293.054796146712,
293.941475509573,294.828154872434,295.714834235294,296.601513598155,297.488192961016,
298.374872323877,298.451302091031),.UNSPECIFIED.);
#4893=B_SPLINE_CURVE_WITH_KNOTS('',3,(#34012,#34013,#34014,#34015,#34016,
#34017,#34018,#34019,#34020,#34021,#34022,#34023),.UNSPECIFIED.,.F.,.F.,
(4,1,1,1,1,1,1,1,1,4),(292.168116783851,292.488429128759,293.486257285827,
293.985171364361,294.484085442896,294.98299952143,295.481913599964,296.479741757032,
297.4775699141,298.451302091031),.UNSPECIFIED.);
#4894=B_SPLINE_CURVE_WITH_KNOTS('',3,(#34028,#34029,#34030,#34031,#34032,
#34033,#34034,#34035,#34036,#34037,#34038,#34039),.UNSPECIFIED.,.F.,.F.,
(4,1,1,1,1,1,1,1,1,4),(285.884931476671,286.818324261583,287.816152418651,
288.813980575719,289.811808732788,290.310722811322,290.809636889856,291.30855096839,
291.807465046924,292.168116783851),.UNSPECIFIED.);
#4895=B_SPLINE_CURVE_WITH_KNOTS('',3,(#34040,#34041,#34042,#34043,#34044,
#34045,#34046,#34047,#34048,#34049,#34050,#34051,#34052,#34053,#34054,#34055,
#34056,#34057,#34058,#34059,#34060,#34061,#34062,#34063,#34064),
 .UNSPECIFIED.,.F.,.F.,(4,3,3,3,3,3,3,3,4),(285.884931476672,286.771610839532,
287.658290202393,288.544969565254,289.431648928115,290.318328290976,291.205007653837,
292.091687016697,292.168116783851),.UNSPECIFIED.);
#4896=B_SPLINE_CURVE_WITH_KNOTS('',3,(#34069,#34070,#34071,#34072,#34073,
#34074,#34075,#34076,#34077,#34078,#34079,#34080,#34081),.UNSPECIFIED.,
 .F.,.F.,(4,1,1,1,1,1,1,1,1,1,4),(279.601746169492,279.833527162105,280.831355319173,
281.829183476242,282.82701163331,283.325925711844,283.824839790378,284.323753868912,
284.822667947446,285.820496104515,285.884931476671),.UNSPECIFIED.);
#4897=B_SPLINE_CURVE_WITH_KNOTS('',3,(#34082,#34083,#34084,#34085,#34086,
#34087,#34088,#34089,#34090,#34091,#34092,#34093),.UNSPECIFIED.,.F.,.F.,
(4,1,1,1,1,1,1,1,1,4),(279.601746169492,280.015577165406,280.51449124394,
281.013405322474,281.512319401008,282.510147558077,283.507975715145,284.505803872213,
285.503632029281,285.884931476672),.UNSPECIFIED.);
#4898=B_SPLINE_CURVE_WITH_KNOTS('',3,(#34098,#34099,#34100,#34101,#34102,
#34103,#34104,#34105,#34106,#34107,#34108,#34109),.UNSPECIFIED.,.F.,.F.,
(4,1,1,1,1,1,1,1,1,4),(273.318560862312,273.846558219696,274.844386376764,
275.842214533832,276.341128612366,276.8400426909,277.338956769435,277.837870847969,
278.835699005037,279.601746169492),.UNSPECIFIED.);
#4899=B_SPLINE_CURVE_WITH_KNOTS('',3,(#34110,#34111,#34112,#34113,#34114,
#34115,#34116,#34117,#34118,#34119,#34120,#34121),.UNSPECIFIED.,.F.,.F.,
(4,1,1,1,1,1,1,1,1,4),(273.318560862312,273.529694144462,274.028608222996,
274.52752230153,275.525350458599,276.523178615667,277.521006772735,278.518834929803,
279.516663086872,279.601746169492),.UNSPECIFIED.);
#4900=B_SPLINE_CURVE_WITH_KNOTS('',3,(#34126,#34127,#34128,#34129,#34130,
#34131,#34132,#34133,#34134,#34135,#34136,#34137),.UNSPECIFIED.,.F.,.F.,
(4,1,1,1,1,1,1,1,1,4),(267.035375555133,267.859589277286,268.857417434354,
269.356331512888,269.855245591423,270.354159669957,270.853073748491,271.850901905559,
272.848730062627,273.318560862312),.UNSPECIFIED.);
#4901=B_SPLINE_CURVE_WITH_KNOTS('',3,(#34138,#34139,#34140,#34141,#34142,
#34143,#34144,#34145,#34146,#34147,#34148,#34149),.UNSPECIFIED.,.F.,.F.,
(4,1,1,1,1,1,1,1,1,4),(267.035375555133,267.043811123519,267.542725202053,
268.540553359121,269.538381516189,270.536209673257,271.534037830326,272.531865987394,
273.030780065928,273.318560862312),.UNSPECIFIED.);
#4902=B_SPLINE_CURVE_WITH_KNOTS('',3,(#34154,#34155,#34156,#34157,#34158,
#34159,#34160,#34161,#34162,#34163,#34164,#34165,#34166),.UNSPECIFIED.,
 .F.,.F.,(4,1,1,1,1,1,1,1,1,1,4),(260.752190247953,260.874792177808,261.872620334877,
262.371534413411,262.870448491945,263.369362570479,263.868276649013,264.866104806081,
265.86393296315,266.861761120218,267.035375555133),.UNSPECIFIED.);
#4903=B_SPLINE_CURVE_WITH_KNOTS('',3,(#34167,#34168,#34169,#34170,#34171,
#34172,#34173,#34174,#34175,#34176,#34177),.UNSPECIFIED.,.F.,.F.,(4,1,1,
1,1,1,1,1,4),(260.752190247953,261.555756259643,262.553584416711,263.55141257378,
264.549240730848,265.547068887916,266.04598296645,266.544897044984,267.035375555133),
 .UNSPECIFIED.);
#4904=B_SPLINE_CURVE_WITH_KNOTS('',3,(#34182,#34183,#34184,#34185,#34186,
#34187,#34188,#34189,#34190,#34191,#34192,#34193),.UNSPECIFIED.,.F.,.F.,
(4,1,1,1,1,1,1,1,1,4),(254.469004940774,254.887823235399,255.386737313933,
255.885651392467,256.384565471001,256.883479549535,257.881307706603,258.879135863672,
259.87696402074,260.752190247953),.UNSPECIFIED.);
#4905=B_SPLINE_CURVE_WITH_KNOTS('',3,(#34194,#34195,#34196,#34197,#34198,
#34199,#34200,#34201,#34202,#34203,#34204,#34205,#34206,#34207,#34208,#34209,
#34210,#34211,#34212,#34213,#34214,#34215,#34216,#34217,#34218),
 .UNSPECIFIED.,.F.,.F.,(4,3,3,3,3,3,3,3,4),(254.469004940774,255.355684303635,
256.242363666495,257.129043029356,258.015722392217,258.902401755078,259.789081117939,
260.6757604808,260.752190247953),.UNSPECIFIED.);
#4906=B_SPLINE_CURVE_WITH_KNOTS('',3,(#34223,#34224,#34225,#34226,#34227,
#34228,#34229,#34230,#34231,#34232,#34233,#34234,#34235,#34236,#34237,#34238,
#34239,#34240,#34241,#34242,#34243,#34244,#34245,#34246,#34247),
 .UNSPECIFIED.,.F.,.F.,(4,3,3,3,3,3,3,3,4),(248.185819633594,249.072498996455,
249.959178359316,250.845857722176,251.732537085037,252.619216447898,253.505895810759,
254.392575173619,254.469004940774),.UNSPECIFIED.);
#4907=B_SPLINE_CURVE_WITH_KNOTS('',3,(#34248,#34249,#34250,#34251,#34252,
#34253,#34254,#34255,#34256,#34257,#34258,#34259),.UNSPECIFIED.,.F.,.F.,
(4,1,1,1,1,1,1,1,1,4),(248.185819633594,248.583990217756,249.581818374824,
250.579646531892,251.577474688961,252.076388767495,252.575302846029,253.074216924563,
253.573131003097,254.469004940774),.UNSPECIFIED.);
#4908=B_SPLINE_CURVE_WITH_KNOTS('',3,(#34264,#34265,#34266,#34267,#34268,
#34269,#34270,#34271,#34272,#34273,#34274,#34275),.UNSPECIFIED.,.F.,.F.,
(4,1,1,1,1,1,1,1,1,4),(241.902634326414,241.916057193511,242.414971272045,
242.91388535058,243.911713507648,244.909541664716,245.907369821784,246.905197978853,
247.903026135921,248.185819633594),.UNSPECIFIED.);
#4909=B_SPLINE_CURVE_WITH_KNOTS('',3,(#34276,#34277,#34278,#34279,#34280,
#34281,#34282,#34283,#34284,#34285,#34286,#34287),.UNSPECIFIED.,.F.,.F.,
(4,1,1,1,1,1,1,1,1,4),(241.902634326415,242.597021275346,243.594849432414,
244.592677589483,245.091591668017,245.590505746551,246.089419825085,246.588333903619,
247.586162060688,248.185819633594),.UNSPECIFIED.);
#4910=B_SPLINE_CURVE_WITH_KNOTS('',3,(#34292,#34293,#34294,#34295,#34296,
#34297,#34298,#34299,#34300,#34301,#34302),.UNSPECIFIED.,.F.,.F.,(4,1,1,
1,1,1,1,1,4),(235.619449019235,235.929088251102,236.92691640817,237.924744565238,
238.922572722307,239.920400879375,240.918229036443,241.417143114977,241.902634326414),
 .UNSPECIFIED.);
#4911=B_SPLINE_CURVE_WITH_KNOTS('',3,(#34303,#34304,#34305,#34306,#34307,
#34308,#34309,#34310,#34311,#34312,#34313,#34314),.UNSPECIFIED.,.F.,.F.,
(4,1,1,1,1,1,1,1,1,4),(235.619449019235,236.610052332937,237.607880490005,
238.106794568539,238.605708647073,239.104622725607,239.603536804141,240.60136496121,
241.599193118278,241.902634326415),.UNSPECIFIED.);
#4912=B_SPLINE_CURVE_WITH_KNOTS('',3,(#34319,#34320,#34321,#34322,#34323,
#34324,#34325,#34326,#34327,#34328,#34329,#34330,#34331,#34332,#34333,#34334,
#34335,#34336,#34337,#34338,#34339,#34340,#34341,#34342,#34343),
 .UNSPECIFIED.,.F.,.F.,(4,3,3,3,3,3,3,3,4),(229.336263712055,230.222943074916,
231.109622437777,231.996301800638,232.882981163499,233.769660526359,234.65633988922,
235.543019252081,235.619449019235),.UNSPECIFIED.);
#4913=B_SPLINE_CURVE_WITH_KNOTS('',3,(#34344,#34345,#34346,#34347,#34348,
#34349,#34350,#34351,#34352,#34353,#34354,#34355,#34356),.UNSPECIFIED.,
 .F.,.F.,(4,1,1,1,1,1,1,1,1,1,4),(229.336263712055,229.625255233459,230.623083390527,
231.121997469061,231.620911547595,232.11982562613,232.618739704664,233.616567861732,
234.6143960188,235.612224175868,235.619449019235),.UNSPECIFIED.);
#4914=B_SPLINE_CURVE_WITH_KNOTS('',3,(#34361,#34362,#34363,#34364,#34365,
#34366,#34367,#34368,#34369,#34370,#34371,#34372),.UNSPECIFIED.,.F.,.F.,
(4,1,1,1,1,1,1,1,1,4),(223.053078404876,223.955150366283,224.952978523351,
225.950806680419,226.948634837488,227.447548916022,227.946462994556,228.44537707309,
228.944291151624,229.336263712055),.UNSPECIFIED.);
#4915=B_SPLINE_CURVE_WITH_KNOTS('',3,(#34373,#34374,#34375,#34376,#34377,
#34378,#34379,#34380,#34381,#34382,#34383,#34384,#34385,#34386,#34387,#34388,
#34389,#34390,#34391,#34392,#34393,#34394,#34395,#34396,#34397),
 .UNSPECIFIED.,.F.,.F.,(4,3,3,3,3,3,3,3,4),(223.053078404876,223.939757767737,
224.826437130597,225.713116493458,226.599795856319,227.48647521918,228.373154582041,
229.259833944901,229.336263712055),.UNSPECIFIED.);
#4916=B_SPLINE_CURVE_WITH_KNOTS('',3,(#34402,#34403,#34404,#34405,#34406,
#34407,#34408,#34409,#34410,#34411,#34412,#34413,#34414),.UNSPECIFIED.,
 .F.,.F.,(4,1,1,1,1,1,1,1,1,1,4),(216.769893097696,216.970353266805,217.968181423873,
218.966009580941,219.96383773801,220.462751816544,220.961665895078,221.460579973612,
221.959494052146,222.957322209214,223.053078404876),.UNSPECIFIED.);
#4917=B_SPLINE_CURVE_WITH_KNOTS('',3,(#34415,#34416,#34417,#34418,#34419,
#34420,#34421,#34422,#34423,#34424,#34425,#34426),.UNSPECIFIED.,.F.,.F.,
(4,1,1,1,1,1,1,1,1,4),(216.769893097696,217.152403270106,217.65131734864,
218.150231427174,218.649145505708,219.646973662776,220.644801819845,221.642629976913,
222.640458133981,223.053078404876),.UNSPECIFIED.);
#4918=B_SPLINE_CURVE_WITH_KNOTS('',3,(#34431,#34432,#34433,#34434,#34435,
#34436,#34437,#34438,#34439,#34440,#34441),.UNSPECIFIED.,.F.,.F.,(4,1,1,
1,1,1,1,1,4),(210.486707790517,210.983384324395,211.981212481464,212.979040638532,
213.9768687956,214.974696952668,215.972525109737,216.471439188271,216.769893097696),
 .UNSPECIFIED.);
#4919=B_SPLINE_CURVE_WITH_KNOTS('',3,(#34442,#34443,#34444,#34445,#34446,
#34447,#34448,#34449,#34450,#34451,#34452,#34453),.UNSPECIFIED.,.F.,.F.,
(4,1,1,1,1,1,1,1,1,4),(210.486707790517,210.666520249162,211.66434840623,
212.662176563298,213.161090641833,213.660004720367,214.657832877435,215.655661034503,
216.653489191572,216.769893097696),.UNSPECIFIED.);
#4920=B_SPLINE_CURVE_WITH_KNOTS('',3,(#34458,#34459,#34460,#34461,#34462,
#34463,#34464,#34465,#34466,#34467,#34468,#34469,#34470,#34471,#34472,#34473,
#34474,#34475,#34476,#34477,#34478,#34479,#34480,#34481,#34482),
 .UNSPECIFIED.,.F.,.F.,(4,3,3,3,3,3,3,3,4),(204.203522483337,205.090201846198,
205.976881209059,206.86356057192,207.75023993478,208.636919297641,209.523598660502,
210.410278023363,210.486707790517),.UNSPECIFIED.);
#4921=B_SPLINE_CURVE_WITH_KNOTS('',3,(#34483,#34484,#34485,#34486,#34487,
#34488,#34489,#34490,#34491,#34492,#34493,#34494),.UNSPECIFIED.,.F.,.F.,
(4,1,1,1,1,1,1,1,1,4),(204.203522483337,204.679551306752,205.178465385287,
205.677379463821,206.176293542355,206.675207620889,207.673035777957,208.670863935025,
209.668692092094,210.486707790517),.UNSPECIFIED.);
#4922=B_SPLINE_CURVE_WITH_KNOTS('',3,(#34499,#34500,#34501,#34502,#34503,
#34504,#34505,#34506,#34507,#34508,#34509,#34510,#34511),.UNSPECIFIED.,
 .F.,.F.,(4,1,1,1,1,1,1,1,1,1,4),(197.920337176158,198.011618282508,199.009446439576,
200.007274596645,201.005102753713,201.504016832247,202.002930910781,202.501844989315,
203.000759067849,203.998587224918,204.203522483337),.UNSPECIFIED.);
#4923=B_SPLINE_CURVE_WITH_KNOTS('',3,(#34512,#34513,#34514,#34515,#34516,
#34517,#34518,#34519,#34520,#34521,#34522,#34523,#34524,#34525,#34526,#34527,
#34528,#34529,#34530,#34531,#34532,#34533,#34534,#34535,#34536),
 .UNSPECIFIED.,.F.,.F.,(4,3,3,3,3,3,3,3,4),(197.920337176158,198.807016539019,
199.693695901879,200.58037526474,201.467054627601,202.353733990462,203.240413353323,
204.127092716184,204.203522483337),.UNSPECIFIED.);
#4924=B_SPLINE_CURVE_WITH_KNOTS('',3,(#34541,#34542,#34543,#34544,#34545,
#34546,#34547,#34548,#34549,#34550,#34551,#34552),.UNSPECIFIED.,.F.,.F.,
(4,1,1,1,1,1,1,1,1,4),(191.637151868978,192.024649340099,193.022477497167,
194.020305654235,194.519219732769,195.018133811303,195.517047889837,196.015961968372,
197.01379012544,197.920337176158),.UNSPECIFIED.);
#4925=B_SPLINE_CURVE_WITH_KNOTS('',3,(#34553,#34554,#34555,#34556,#34557,
#34558,#34559,#34560,#34561,#34562,#34563,#34564),.UNSPECIFIED.,.F.,.F.,
(4,1,1,1,1,1,1,1,1,4),(191.637151868978,191.707785264865,192.206699343399,
192.705613421933,193.703441579002,194.70126973607,195.699097893138,196.696926050206,
197.694754207275,197.920337176158),.UNSPECIFIED.);
#4926=B_SPLINE_CURVE_WITH_KNOTS('',3,(#34569,#34570,#34571,#34572,#34573,
#34574,#34575,#34576,#34577,#34578,#34579,#34580),.UNSPECIFIED.,.F.,.F.,
(4,1,1,1,1,1,1,1,1,4),(185.353966561798,186.037680397689,187.035508554757,
187.534422633291,188.033336711825,188.53225079036,189.031164868894,190.028993025962,
191.02682118303,191.637151868978),.UNSPECIFIED.);
#4927=B_SPLINE_CURVE_WITH_KNOTS('',3,(#34581,#34582,#34583,#34584,#34585,
#34586,#34587,#34588,#34589,#34590,#34591),.UNSPECIFIED.,.F.,.F.,(4,1,1,
1,1,1,1,1,4),(185.353966561799,185.720816322456,186.718644479524,187.716472636592,
188.71430079366,189.712128950729,190.709957107797,191.208871186331,191.637151868978),
 .UNSPECIFIED.);
#4928=B_SPLINE_CURVE_WITH_KNOTS('',3,(#34596,#34597,#34598,#34599,#34600,
#34601,#34602,#34603,#34604,#34605,#34606,#34607),.UNSPECIFIED.,.F.,.F.,
(4,1,1,1,1,1,1,1,1,4),(179.070781254619,180.050711455279,180.549625533814,
181.048539612348,181.547453690882,182.046367769416,183.044195926484,184.042024083552,
185.039852240621,185.353966561798),.UNSPECIFIED.);
#4929=B_SPLINE_CURVE_WITH_KNOTS('',3,(#34608,#34609,#34610,#34611,#34612,
#34613,#34614,#34615,#34616,#34617,#34618,#34619,#34620,#34621,#34622,#34623,
#34624,#34625,#34626,#34627,#34628,#34629,#34630,#34631,#34632),
 .UNSPECIFIED.,.F.,.F.,(4,3,3,3,3,3,3,3,4),(179.070781254619,179.95746061748,
180.844139980341,181.730819343202,182.617498706062,183.504178068923,184.390857431784,
185.277536794645,185.353966561799),.UNSPECIFIED.);
#4930=B_SPLINE_CURVE_WITH_KNOTS('',3,(#34637,#34638,#34639,#34640,#34641,
#34642,#34643,#34644,#34645,#34646,#34647,#34648,#34649),.UNSPECIFIED.,
 .F.,.F.,(4,1,1,1,1,1,1,1,1,1,4),(172.787595947439,173.065914355802,173.564828434336,
174.06374251287,174.562656591404,175.061570669938,176.059398827006,177.057226984075,
178.055055141143,179.052883298211,179.070781254619),.UNSPECIFIED.);
#4931=B_SPLINE_CURVE_WITH_KNOTS('',3,(#34650,#34651,#34652,#34653,#34654,
#34655,#34656,#34657,#34658,#34659,#34660,#34661),.UNSPECIFIED.,.F.,.F.,
(4,1,1,1,1,1,1,1,1,4),(172.787595947439,173.746878437636,174.744706594705,
175.742534751773,176.740362908841,177.239276987375,177.738191065909,178.237105144444,
178.736019222978,179.070781254619),.UNSPECIFIED.);
#4932=B_SPLINE_CURVE_WITH_KNOTS('',3,(#34666,#34667,#34668,#34669,#34670,
#34671,#34672,#34673,#34674,#34675,#34676,#34677,#34678,#34679,#34680,#34681,
#34682,#34683,#34684,#34685,#34686,#34687,#34688,#34689,#34690),
 .UNSPECIFIED.,.F.,.F.,(4,3,3,3,3,3,3,3,4),(166.50441064026,167.391090003121,
168.277769365981,169.164448728842,170.051128091703,170.937807454564,171.824486817425,
172.711166180286,172.787595947439),.UNSPECIFIED.);
#4933=B_SPLINE_CURVE_WITH_KNOTS('',3,(#34691,#34692,#34693,#34694,#34695,
#34696,#34697,#34698,#34699,#34700,#34701,#34702,#34703),.UNSPECIFIED.,
 .F.,.F.,(4,1,1,1,1,1,1,1,1,1,4),(166.50441064026,166.762081338159,167.759909495227,
168.757737652295,169.755565809363,170.254479887898,170.753393966432,171.252308044966,
171.7512221235,172.749050280568,172.787595947439),.UNSPECIFIED.);
#4934=B_SPLINE_CURVE_WITH_KNOTS('',3,(#34708,#34709,#34710,#34711,#34712,
#34713,#34714,#34715,#34716,#34717,#34718),.UNSPECIFIED.,.F.,.F.,(4,1,1,
1,1,1,1,1,4),(160.22122533308,160.593062392448,161.091976470983,162.089804628051,
163.087632785119,164.085460942187,165.083289099256,166.081117256324,166.50441064026),
 .UNSPECIFIED.);
#4935=B_SPLINE_CURVE_WITH_KNOTS('',3,(#34719,#34720,#34721,#34722,#34723,
#34724,#34725,#34726,#34727,#34728,#34729,#34730),.UNSPECIFIED.,.F.,.F.,
(4,1,1,1,1,1,1,1,1,4),(160.22122533308,160.775112395749,161.772940552817,
162.770768709886,163.26968278842,163.768596866954,164.267510945488,164.766425024022,
165.76425318109,166.50441064026),.UNSPECIFIED.);
#4936=B_SPLINE_CURVE_WITH_KNOTS('',3,(#34735,#34736,#34737,#34738,#34739,
#34740,#34741,#34742,#34743,#34744,#34745,#34746,#34747,#34748,#34749,#34750,
#34751,#34752,#34753,#34754,#34755,#34756,#34757,#34758,#34759),
 .UNSPECIFIED.,.F.,.F.,(4,3,3,3,3,3,3,3,4),(153.938040025901,154.824719388761,
155.711398751622,156.598078114483,157.484757477344,158.371436840205,159.258116203066,
160.144795565927,160.22122533308),.UNSPECIFIED.);
#4937=B_SPLINE_CURVE_WITH_KNOTS('',3,(#34760,#34761,#34762,#34763,#34764,
#34765,#34766,#34767,#34768,#34769,#34770,#34771),.UNSPECIFIED.,.F.,.F.,
(4,1,1,1,1,1,1,1,1,4),(153.938040025901,154.78814345334,155.785971610408,
156.284885688942,156.783799767476,157.28271384601,157.781627924544,158.779456081613,
159.777284238681,160.22122533308),.UNSPECIFIED.);
#4938=B_SPLINE_CURVE_WITH_KNOTS('',3,(#34776,#34777,#34778,#34779,#34780,
#34781,#34782,#34783,#34784,#34785,#34786,#34787),.UNSPECIFIED.,.F.,.F.,
(4,1,1,1,1,1,1,1,1,4),(147.654854718721,148.120210429095,149.118038586163,
150.115866743232,151.1136949003,152.111523057368,152.610437135902,153.109351214436,
153.608265292971,153.938040025901),.UNSPECIFIED.);
#4939=B_SPLINE_CURVE_WITH_KNOTS('',3,(#34788,#34789,#34790,#34791,#34792,
#34793,#34794,#34795,#34796,#34797,#34798,#34799,#34800),.UNSPECIFIED.,
 .F.,.F.,(4,1,1,1,1,1,1,1,1,1,4),(147.654854718721,147.803346353862,148.80117451093,
149.300088589464,149.799002667998,150.297916746532,150.796830825067,151.794658982135,
152.792487139203,153.790315296271,153.938040025901),.UNSPECIFIED.);
#4940=B_SPLINE_CURVE_WITH_KNOTS('',3,(#34805,#34806,#34807,#34808,#34809,
#34810,#34811,#34812,#34813,#34814,#34815,#34816,#34817,#34818,#34819,#34820,
#34821,#34822,#34823,#34824,#34825,#34826,#34827,#34828,#34829),
 .UNSPECIFIED.,.F.,.F.,(4,3,3,3,3,3,3,3,4),(141.371669411541,142.258348774402,
143.145028137263,144.031707500124,144.918386862985,145.805066225846,146.691745588707,
147.578424951567,147.654854718721),.UNSPECIFIED.);
#4941=B_SPLINE_CURVE_WITH_KNOTS('',3,(#34830,#34831,#34832,#34833,#34834,
#34835,#34836,#34837,#34838,#34839,#34840,#34841),.UNSPECIFIED.,.F.,.F.,
(4,1,1,1,1,1,1,1,1,4),(141.371669411542,141.816377411452,142.315291489986,
142.81420556852,143.313119647055,143.812033725589,144.809861882657,145.807690039725,
146.805518196793,147.654854718721),.UNSPECIFIED.);
#4942=B_SPLINE_CURVE_WITH_KNOTS('',3,(#34846,#34847,#34848,#34849,#34850,
#34851,#34852,#34853,#34854,#34855,#34856,#34857,#34858),.UNSPECIFIED.,
 .F.,.F.,(4,1,1,1,1,1,1,1,1,1,4),(135.088484104362,135.148444387208,136.146272544276,
137.144100701344,138.141928858413,138.640842936947,139.139757015481,139.638671094015,
140.137585172549,141.135413329617,141.371669411541),.UNSPECIFIED.);
#4943=B_SPLINE_CURVE_WITH_KNOTS('',3,(#34859,#34860,#34861,#34862,#34863,
#34864,#34865,#34866,#34867,#34868,#34869,#34870,#34871,#34872,#34873,#34874,
#34875,#34876,#34877,#34878,#34879,#34880,#34881,#34882,#34883),
 .UNSPECIFIED.,.F.,.F.,(4,3,3,3,3,3,3,3,4),(135.088484104362,135.975163467223,
136.861842830084,137.748522192945,138.635201555806,139.521880918667,140.408560281528,
141.295239644388,141.371669411542),.UNSPECIFIED.);
#4944=B_SPLINE_CURVE_WITH_KNOTS('',3,(#34888,#34889,#34890,#34891,#34892,
#34893,#34894,#34895,#34896,#34897,#34898,#34899),.UNSPECIFIED.,.F.,.F.,
(4,1,1,1,1,1,1,1,1,4),(128.805298797182,129.161475444798,130.159303601867,
131.157131758935,131.656045837469,132.154959916003,132.653873994537,133.152788073071,
134.15061623014,135.088484104362),.UNSPECIFIED.);
#4945=B_SPLINE_CURVE_WITH_KNOTS('',3,(#34900,#34901,#34902,#34903,#34904,
#34905,#34906,#34907,#34908,#34909,#34910,#34911),.UNSPECIFIED.,.F.,.F.,
(4,1,1,1,1,1,1,1,1,4),(128.805298797182,128.844611369565,129.343525448099,
129.842439526633,130.840267683701,131.83809584077,132.835923997838,133.833752154906,
134.831580311974,135.088484104362),.UNSPECIFIED.);
#4946=B_SPLINE_CURVE_WITH_KNOTS('',3,(#34916,#34917,#34918,#34919,#34920,
#34921,#34922,#34923,#34924,#34925,#34926,#34927),.UNSPECIFIED.,.F.,.F.,
(4,1,1,1,1,1,1,1,1,4),(122.522113490003,123.174506502389,124.172334659457,
124.671248737991,125.170162816525,125.669076895059,126.167990973594,127.165819130662,
128.16364728773,128.805298797182),.UNSPECIFIED.);
#4947=B_SPLINE_CURVE_WITH_KNOTS('',3,(#34928,#34929,#34930,#34931,#34932,
#34933,#34934,#34935,#34936,#34937,#34938),.UNSPECIFIED.,.F.,.F.,(4,1,1,
1,1,1,1,1,4),(122.522113490003,122.857642427155,123.855470584224,124.853298741292,
125.85112689836,126.848955055428,127.846783212497,128.345697291031,128.805298797182),
 .UNSPECIFIED.);
#4948=B_SPLINE_CURVE_WITH_KNOTS('',3,(#34943,#34944,#34945,#34946,#34947,
#34948,#34949,#34950,#34951,#34952,#34953,#34954),.UNSPECIFIED.,.F.,.F.,
(4,1,1,1,1,1,1,1,1,4),(116.238928182823,117.187537559979,117.686451638513,
118.185365717047,118.684279795582,119.183193874116,120.181022031184,121.178850188252,
122.17667834532,122.522113490003),.UNSPECIFIED.);
#4949=B_SPLINE_CURVE_WITH_KNOTS('',3,(#34955,#34956,#34957,#34958,#34959,
#34960,#34961,#34962,#34963,#34964,#34965,#34966,#34967,#34968,#34969,#34970,
#34971,#34972,#34973,#34974,#34975,#34976,#34977,#34978,#34979),
 .UNSPECIFIED.,.F.,.F.,(4,3,3,3,3,3,3,3,4),(116.238928182823,117.125607545684,
118.012286908545,118.898966271406,119.785645634267,120.672324997128,121.559004359989,
122.445683722849,122.522113490003),.UNSPECIFIED.);
#4950=B_SPLINE_CURVE_WITH_KNOTS('',3,(#34984,#34985,#34986,#34987,#34988,
#34989,#34990,#34991,#34992,#34993,#34994,#34995,#34996),.UNSPECIFIED.,
 .F.,.F.,(4,1,1,1,1,1,1,1,1,1,4),(109.955742875644,110.202740460501,110.701654539036,
111.20056861757,111.699482696104,112.198396774638,113.196224931706,114.194053088774,
115.191881245843,116.189709402911,116.238928182823),.UNSPECIFIED.);
#4951=B_SPLINE_CURVE_WITH_KNOTS('',3,(#34997,#34998,#34999,#35000,#35001,
#35002,#35003,#35004,#35005,#35006,#35007,#35008),.UNSPECIFIED.,.F.,.F.,
(4,1,1,1,1,1,1,1,1,4),(109.955742875644,110.883704542336,111.881532699404,
112.879360856473,113.877189013541,114.376103092075,114.875017170609,115.373931249143,
115.872845327677,116.238928182823),.UNSPECIFIED.);
#4952=B_SPLINE_CURVE_WITH_KNOTS('',3,(#35013,#35014,#35015,#35016,#35017,
#35018,#35019,#35020,#35021,#35022,#35023,#35024),.UNSPECIFIED.,.F.,.F.,
(4,1,1,1,1,1,1,1,1,4),(103.672557568464,103.716857439558,104.215771518092,
104.714685596626,105.21359967516,106.211427832228,107.209255989297,108.207084146365,
109.204912303433,109.955742875644),.UNSPECIFIED.);
#4953=B_SPLINE_CURVE_WITH_KNOTS('',3,(#35025,#35026,#35027,#35028,#35029,
#35030,#35031,#35032,#35033,#35034,#35035,#35036,#35037),.UNSPECIFIED.,
 .F.,.F.,(4,1,1,1,1,1,1,1,1,1,4),(103.672557568464,103.898907442858,104.896735599927,
105.894563756995,106.892391914063,107.391305992597,107.890220071131,108.389134149666,
108.8880482282,109.885876385268,109.955742875644),.UNSPECIFIED.);
#4954=B_SPLINE_CURVE_WITH_KNOTS('',3,(#35042,#35043,#35044,#35045,#35046,
#35047,#35048,#35049,#35050,#35051,#35052),.UNSPECIFIED.,.F.,.F.,(4,1,1,
1,1,1,1,1,4),(97.3893722612844,97.7298884971482,98.2288025756823,99.2266307327506,
100.224458889819,101.222287046887,102.220115203955,103.217943361024,103.672557568464),
 .UNSPECIFIED.);
#4955=B_SPLINE_CURVE_WITH_KNOTS('',3,(#35053,#35054,#35055,#35056,#35057,
#35058,#35059,#35060,#35061,#35062,#35063,#35064),.UNSPECIFIED.,.F.,.F.,
(4,1,1,1,1,1,1,1,1,4),(97.3893722612845,97.9119385004489,98.9097666575171,
99.9075948145854,100.406508893119,100.905422971654,101.404337050188,101.903251128722,
102.90107928579,103.672557568464),.UNSPECIFIED.);
#4956=B_SPLINE_CURVE_WITH_KNOTS('',3,(#35069,#35070,#35071,#35072,#35073,
#35074,#35075,#35076,#35077,#35078,#35079,#35080,#35081,#35082,#35083,#35084,
#35085,#35086,#35087,#35088,#35089,#35090,#35091,#35092,#35093),
 .UNSPECIFIED.,.F.,.F.,(4,3,3,3,3,3,3,3,4),(91.1061869541048,91.9928663169656,
92.8795456798265,93.7662250426873,94.6529044055482,95.539583768409,96.4262631312698,
97.3129424941307,97.3893722612844),.UNSPECIFIED.);
#4957=B_SPLINE_CURVE_WITH_KNOTS('',3,(#35094,#35095,#35096,#35097,#35098,
#35099,#35100,#35101,#35102,#35103,#35104,#35105),.UNSPECIFIED.,.F.,.F.,
(4,1,1,1,1,1,1,1,1,4),(91.1061869541048,91.9249695580393,92.9227977151076,
93.4217117936417,93.9206258721758,94.4195399507099,94.9184540292441,95.9162821863123,
96.9141103433806,97.3893722612845),.UNSPECIFIED.);
#4958=B_SPLINE_CURVE_WITH_KNOTS('',3,(#35110,#35111,#35112,#35113,#35114,
#35115,#35116,#35117,#35118,#35119,#35120,#35121),.UNSPECIFIED.,.F.,.F.,
(4,1,1,1,1,1,1,1,1,4),(84.8230016469252,85.257036533795,86.2548646908632,
87.2526928479315,88.2505210049997,89.248349162068,89.7472632406021,90.2461773191363,
90.7450913976704,91.1061869541048),.UNSPECIFIED.);
#4959=B_SPLINE_CURVE_WITH_KNOTS('',3,(#35122,#35123,#35124,#35125,#35126,
#35127,#35128,#35129,#35130,#35131,#35132,#35133,#35134),.UNSPECIFIED.,
 .F.,.F.,(4,1,1,1,1,1,1,1,1,1,4),(84.8230016469253,84.9401724585615,85.9380006156298,
86.4369146941639,86.935828772698,87.4347428512321,87.9336569297663,88.9314850868345,
89.9293132439028,90.927141400971,91.1061869541048),.UNSPECIFIED.);
#4960=B_SPLINE_CURVE_WITH_KNOTS('',3,(#35139,#35140,#35141,#35142,#35143,
#35144,#35145,#35146,#35147,#35148,#35149,#35150,#35151,#35152,#35153,#35154,
#35155,#35156,#35157,#35158,#35159,#35160,#35161,#35162,#35163),
 .UNSPECIFIED.,.F.,.F.,(4,3,3,3,3,3,3,3,4),(78.5398163397456,79.4264957026064,
80.3131750654673,81.1998544283281,82.086533791189,82.9732131540499,83.8598925169107,
84.7465718797716,84.8230016469252),.UNSPECIFIED.);
#4961=B_SPLINE_CURVE_WITH_KNOTS('',3,(#35164,#35165,#35166,#35167,#35168,
#35169,#35170,#35171,#35172,#35173,#35174,#35175),.UNSPECIFIED.,.F.,.F.,
(4,1,1,1,1,1,1,1,1,4),(78.5398163397457,78.953203516152,79.4521175946861,
79.9510316732202,80.4499457517543,80.9488598302885,81.9466879873567,82.944516144425,
83.9423443014932,84.8230016469253),.UNSPECIFIED.);
#4962=B_SPLINE_CURVE_WITH_KNOTS('',3,(#35180,#35181,#35182,#35183,#35184,
#35185,#35186,#35187,#35188,#35189,#35190,#35191,#35192),.UNSPECIFIED.,
 .F.,.F.,(4,1,1,1,1,1,1,1,1,1,4),(72.256631032566,72.2852704919076,73.2830986489759,
74.2809268060441,75.2787549631124,75.7776690416465,76.2765831201806,76.7754971987148,
77.2744112772489,78.2722394343172,78.5398163397456),.UNSPECIFIED.);
#4963=B_SPLINE_CURVE_WITH_KNOTS('',3,(#35193,#35194,#35195,#35196,#35197,
#35198,#35199,#35200,#35201,#35202,#35203,#35204,#35205,#35206,#35207,#35208,
#35209,#35210,#35211,#35212,#35213,#35214,#35215,#35216,#35217),
 .UNSPECIFIED.,.F.,.F.,(4,3,3,3,3,3,3,3,4),(72.2566310325661,73.143310395427,
74.0299897582878,74.9166691211487,75.8033484840095,76.6900278468704,77.5767072097313,
78.4633865725921,78.5398163397457),.UNSPECIFIED.);
#4964=B_SPLINE_CURVE_WITH_KNOTS('',3,(#35222,#35223,#35224,#35225,#35226,
#35227,#35228,#35229,#35230,#35231,#35232,#35233),.UNSPECIFIED.,.F.,.F.,
(4,1,1,1,1,1,1,1,1,4),(65.9734457253864,66.2983015494981,67.2961297065663,
68.2939578636346,68.7928719421687,69.2917860207028,69.790700099237,70.2896141777711,
71.2874423348394,72.256631032566),.UNSPECIFIED.);
#4965=B_SPLINE_CURVE_WITH_KNOTS('',3,(#35234,#35235,#35236,#35237,#35238,
#35239,#35240,#35241,#35242,#35243,#35244,#35245),.UNSPECIFIED.,.F.,.F.,
(4,1,1,1,1,1,1,1,1,4),(65.9734457253865,65.9814374742646,66.4803515527987,
66.9792656313329,67.9770937884011,68.9749219454694,69.9727501025376,70.9705782596059,
71.9684064166742,72.2566310325661),.UNSPECIFIED.);
#4966=B_SPLINE_CURVE_WITH_KNOTS('',3,(#35250,#35251,#35252,#35253,#35254,
#35255,#35256,#35257,#35258,#35259,#35260,#35261),.UNSPECIFIED.,.F.,.F.,
(4,1,1,1,1,1,1,1,1,4),(59.6902604182068,60.3113326070885,61.3091607641568,
61.8080748426909,62.306988921225,62.8059029997592,63.3048170782933,64.3026452353616,
65.3004733924298,65.9734457253864),.UNSPECIFIED.);
#4967=B_SPLINE_CURVE_WITH_KNOTS('',3,(#35262,#35263,#35264,#35265,#35266,
#35267,#35268,#35269,#35270,#35271,#35272),.UNSPECIFIED.,.F.,.F.,(4,1,1,
1,1,1,1,1,4),(59.6902604182069,59.9944685318551,60.9922966889233,61.9901248459916,
62.9879530030598,63.9857811601281,64.9836093171964,65.4825233957305,65.9734457253865),
 .UNSPECIFIED.);
#4968=B_SPLINE_CURVE_WITH_KNOTS('',3,(#35277,#35278,#35279,#35280,#35281,
#35282,#35283,#35284,#35285,#35286,#35287,#35288),.UNSPECIFIED.,.F.,.F.,
(4,1,1,1,1,1,1,1,1,4),(53.4070751110272,54.324363664679,54.8232777432131,
55.3221918217472,55.8211059002814,56.3200199788155,57.3178481358838,58.315676292952,
59.3135044500203,59.6902604182068),.UNSPECIFIED.);
#4969=B_SPLINE_CURVE_WITH_KNOTS('',3,(#35289,#35290,#35291,#35292,#35293,
#35294,#35295,#35296,#35297,#35298,#35299,#35300,#35301,#35302,#35303,#35304,
#35305,#35306,#35307,#35308,#35309,#35310,#35311,#35312,#35313),
 .UNSPECIFIED.,.F.,.F.,(4,3,3,3,3,3,3,3,4),(53.4070751110273,54.2937544738882,
55.180433836749,56.0671131996099,56.9537925624707,57.8404719253316,58.7271512881924,
59.6138306510532,59.6902604182069),.UNSPECIFIED.);
#4970=B_SPLINE_CURVE_WITH_KNOTS('',3,(#35318,#35319,#35320,#35321,#35322,
#35323,#35324,#35325,#35326,#35327,#35328,#35329,#35330),.UNSPECIFIED.,
 .F.,.F.,(4,1,1,1,1,1,1,1,1,1,4),(47.1238898038476,47.3395665652012,47.8384806437353,
48.3373947222694,48.8363088008036,49.3352228793377,50.333051036406,51.3308791934742,
52.3287073505425,53.3265355076107,53.4070751110272),.UNSPECIFIED.);
#4971=B_SPLINE_CURVE_WITH_KNOTS('',3,(#35331,#35332,#35333,#35334,#35335,
#35336,#35337,#35338,#35339,#35340,#35341,#35342),.UNSPECIFIED.,.F.,.F.,
(4,1,1,1,1,1,1,1,1,4),(47.1238898038477,48.020530647036,49.0183588041042,
50.0161869611725,51.0140151182407,51.5129291967749,52.011843275309,52.5107573538431,
53.0096714323773,53.4070751110273),.UNSPECIFIED.);
#4972=B_SPLINE_CURVE_WITH_KNOTS('',3,(#35347,#35348,#35349,#35350,#35351,
#35352,#35353,#35354,#35355,#35356,#35357,#35358),.UNSPECIFIED.,.F.,.F.,
(4,1,1,1,1,1,1,1,1,4),(40.840704496668,40.8536835442575,41.3525976227916,
41.8515117013258,42.3504257798599,43.3482539369282,44.3460820939964,45.3439102510647,
46.3417384081329,47.1238898038476),.UNSPECIFIED.);
#4973=B_SPLINE_CURVE_WITH_KNOTS('',3,(#35359,#35360,#35361,#35362,#35363,
#35364,#35365,#35366,#35367,#35368,#35369,#35370,#35371),.UNSPECIFIED.,
 .F.,.F.,(4,1,1,1,1,1,1,1,1,1,4),(40.8407044966681,41.0357335475582,42.0335617046264,
43.0313898616947,44.0292180187629,44.5281320972971,45.0270461758312,45.5259602543653,
46.0248743328995,47.0227024899677,47.1238898038477),.UNSPECIFIED.);
#4974=B_SPLINE_CURVE_WITH_KNOTS('',3,(#35376,#35377,#35378,#35379,#35380,
#35381,#35382,#35383,#35384,#35385,#35386),.UNSPECIFIED.,.F.,.F.,(4,1,1,
1,1,1,1,1,4),(34.5575191894884,34.866714601848,35.3656286803821,36.3634568374504,
37.3612849945186,38.3591131515869,39.3569413086551,40.3547694657234,40.840704496668),
 .UNSPECIFIED.);
#4975=B_SPLINE_CURVE_WITH_KNOTS('',3,(#35387,#35388,#35389,#35390,#35391,
#35392,#35393,#35394,#35395,#35396,#35397,#35398),.UNSPECIFIED.,.F.,.F.,
(4,1,1,1,1,1,1,1,1,4),(34.5575191894886,35.0487646051486,36.0465927622169,
37.0444209192851,37.5433349978193,38.0422490763534,38.5411631548875,39.0400772334217,
40.0379053904899,40.8407044966681),.UNSPECIFIED.);
#4976=B_SPLINE_CURVE_WITH_KNOTS('',3,(#35403,#35404,#35405,#35406,#35407,
#35408,#35409,#35410,#35411,#35412,#35413,#35414),.UNSPECIFIED.,.F.,.F.,
(4,1,1,1,1,1,1,1,1,4),(28.2743338823088,28.3808315809043,29.3786597379725,
30.3764878950408,31.3743160521091,32.3721442091773,33.3699723662456,33.8688864447797,
34.3678005233138,34.5575191894884),.UNSPECIFIED.);
#4977=B_SPLINE_CURVE_WITH_KNOTS('',3,(#35415,#35416,#35417,#35418,#35419,
#35420,#35421,#35422,#35423,#35424,#35425,#35426),.UNSPECIFIED.,.F.,.F.,
(4,1,1,1,1,1,1,1,1,4),(28.274333882309,29.0617956627391,30.0596238198073,
30.5585378983415,31.0574519768756,31.5563660554097,32.0552801339438,33.0531082910121,
34.0509364480804,34.5575191894886),.UNSPECIFIED.);
#4978=B_SPLINE_CURVE_WITH_KNOTS('',3,(#35431,#35432,#35433,#35434,#35435,
#35436,#35437,#35438,#35439,#35440,#35441,#35442),.UNSPECIFIED.,.F.,.F.,
(4,1,1,1,1,1,1,1,1,4),(21.9911485751293,22.3938626384947,23.391690795563,
24.3895189526313,25.3873471096995,26.3851752667678,26.8840893453019,27.383003423836,
27.8819175023702,28.2743338823088),.UNSPECIFIED.);
#4979=B_SPLINE_CURVE_WITH_KNOTS('',3,(#35443,#35444,#35445,#35446,#35447,
#35448,#35449,#35450,#35451,#35452,#35453,#35454,#35455),.UNSPECIFIED.,
 .F.,.F.,(4,1,1,1,1,1,1,1,1,1,4),(21.9911485751294,22.0769985632613,23.0748267203295,
23.5737407988637,24.0726548773978,24.5715689559319,25.070483034466,26.0683111915343,
27.0661393486026,28.0639675056708,28.274333882309),.UNSPECIFIED.);
#4980=B_SPLINE_CURVE_WITH_KNOTS('',3,(#35460,#35461,#35462,#35463,#35464,
#35465,#35466,#35467,#35468,#35469,#35470,#35471,#35472,#35473,#35474,#35475,
#35476,#35477,#35478,#35479,#35480,#35481,#35482,#35483,#35484),
 .UNSPECIFIED.,.F.,.F.,(4,3,3,3,3,3,3,3,4),(15.7079632679497,16.5946426308105,
17.4813219936714,18.3680013565322,19.2546807193931,20.1413600822539,21.0280394451148,
21.9147188079757,21.9911485751293),.UNSPECIFIED.);
#4981=B_SPLINE_CURVE_WITH_KNOTS('',3,(#35485,#35486,#35487,#35488,#35489,
#35490,#35491,#35492,#35493,#35494,#35495,#35496),.UNSPECIFIED.,.F.,.F.,
(4,1,1,1,1,1,1,1,1,4),(15.7079632679498,16.0900296208517,16.5889436993859,
17.08785777792,17.5867718564541,18.0856859349882,19.0835140920565,20.0813422491248,
21.079170406193,21.9911485751294),.UNSPECIFIED.);
#4982=B_SPLINE_CURVE_WITH_KNOTS('',3,(#35507,#35508,#35509,#35510,#35511,
#35512,#35513,#35514,#35515,#35516,#35517,#35518,#35519,#35520,#35521,#35522,
#35523,#35524,#35525,#35526,#35527,#35528,#35529,#35530,#35531,#35532,#35533,
#35534,#35535,#35536,#35537,#35538,#35539,#35540,#35541,#35542,#35543,#35544,
#35545,#35546,#35547,#35548,#35549,#35550,#35551,#35552,#35553,#35554,#35555,
#35556,#35557,#35558,#35559,#35560,#35561,#35562,#35563,#35564,#35565,#35566,
#35567,#35568,#35569,#35570,#35571,#35572,#35573,#35574,#35575,#35576,#35577,
#35578,#35579,#35580,#35581,#35582,#35583,#35584,#35585,#35586,#35587,#35588,
#35589,#35590,#35591,#35592,#35593,#35594,#35595,#35596,#35597,#35598,#35599,
#35600,#35601,#35602,#35603,#35604,#35605,#35606,#35607,#35608,#35609,#35610,
#35611,#35612,#35613,#35614,#35615,#35616,#35617,#35618,#35619,#35620,#35621),
 .UNSPECIFIED.,.F.,.F.,(4,3,3,3,3,3,3,3,3,3,3,3,3,3,3,3,3,3,3,3,3,3,3,3,
3,3,3,3,3,3,3,3,3,3,3,3,3,3,4),(-1.3692760959275,-1.32188407678287,-1.27030325921837,
-1.23707822338629,-1.21785653354885,-1.20762469097439,-1.20007327221632,
-1.14735554371125,-1.09412617639606,-1.04931457447893,-1.04159068760046,
-1.03430007797452,-1.0045029725618,-0.950888266579126,-0.89680471903519,
-0.84212054701269,-0.801107417995814,-0.789867050271914,-0.783408395715883,
-0.728461154792874,-0.678068030945187,-0.623694406368148,-0.568930241759064,
-0.540708132249945,-0.532050528924746,-0.526074465104164,-0.470965504745358,
-0.415386731915167,-0.359836412129592,-0.343153365686116,-0.300259194975351,
-0.281492995289392,-0.271248085886408,-0.263224158006185,-0.207778571458046,
-0.151390901540102,-0.0948961475607414,-0.0389343418850663,0.),
 .UNSPECIFIED.);
#4983=B_SPLINE_CURVE_WITH_KNOTS('',3,(#35626,#35627,#35628,#35629,#35630,
#35631,#35632,#35633,#35634,#35635,#35636,#35637,#35638,#35639,#35640,#35641,
#35642,#35643,#35644,#35645,#35646,#35647,#35648,#35649,#35650,#35651,#35652,
#35653,#35654,#35655,#35656,#35657,#35658,#35659,#35660,#35661,#35662,#35663,
#35664,#35665,#35666,#35667,#35668,#35669,#35670,#35671,#35672,#35673,#35674,
#35675,#35676,#35677,#35678,#35679,#35680,#35681,#35682,#35683,#35684,#35685,
#35686,#35687,#35688,#35689,#35690,#35691,#35692,#35693,#35694,#35695,#35696,
#35697,#35698,#35699,#35700,#35701,#35702,#35703,#35704,#35705,#35706,#35707,
#35708,#35709,#35710,#35711,#35712,#35713,#35714,#35715,#35716,#35717,#35718,
#35719,#35720,#35721,#35722,#35723,#35724,#35725,#35726,#35727,#35728,#35729,
#35730,#35731,#35732,#35733,#35734,#35735,#35736,#35737,#35738,#35739,#35740),
 .UNSPECIFIED.,.F.,.F.,(4,3,3,3,3,3,3,3,3,3,3,3,3,3,3,3,3,3,3,3,3,3,3,3,
3,3,3,3,3,3,3,3,3,3,3,3,3,3,4),(-1.36616069392048,-1.3137619280474,-1.25760160850714,
-1.22204589932935,-1.20367987885411,-1.19122237291581,-1.18211951562472,
-1.12620867774649,-1.07028337971536,-1.02171965740005,-1.01246054855555,
-1.00560804218958,-0.973155935084748,-0.917891839945078,-0.862525668265144,
-0.806980972162821,-0.765322450086079,-0.751609718974351,-0.744373329264913,
-0.690070032077305,-0.640346883855853,-0.585898585520381,-0.531637706409828,
-0.504668943522143,-0.497129766489843,-0.490727294658046,-0.437156215864939,
-0.383621580535774,-0.330780907748743,-0.315887603308346,-0.276401652894803,
-0.259126549588878,-0.248755897899905,-0.240651076682722,-0.188174524652693,
-0.135375645330914,-0.0828505825103873,-0.0312642022900974,0.),
 .UNSPECIFIED.);
#4984=B_SPLINE_CURVE_WITH_KNOTS('',3,(#37793,#37794,#37795,#37796,#37797,
#37798,#37799,#37800,#37801,#37802,#37803,#37804,#37805,#37806,#37807,#37808,
#37809,#37810,#37811),.UNSPECIFIED.,.F.,.F.,(4,3,3,3,3,3,4),(387.881378170394,
388.155153099552,388.654067178086,389.152981256621,390.150809413689,391.148637570757,
392.070763168006),.UNSPECIFIED.);
#4985=B_SPLINE_CURVE_WITH_KNOTS('',3,(#37813,#37814,#37815,#37816,#37817,
#37818,#37819,#37820,#37821,#37822,#37823,#37824,#37825,#37826,#37827,#37828,
#37829,#37830,#37831,#37832,#37833,#37834,#37835,#37836,#37837,#37838,#37839,
#37840,#37841,#37842,#37843,#37844,#37845,#37846,#37847,#37848,#37849,#37850,
#37851,#37852,#37853,#37854,#37855,#37856,#37857,#37858,#37859,#37860,#37861,
#37862,#37863,#37864,#37865,#37866,#37867,#37868,#37869,#37870,#37871,#37872,
#37873,#37874,#37875,#37876,#37877,#37878,#37879,#37880,#37881,#37882,#37883,
#37884,#37885,#37886,#37887,#37888,#37889,#37890,#37891,#37892,#37893,#37894,
#37895,#37896,#37897,#37898,#37899,#37900,#37901,#37902,#37903,#37904,#37905,
#37906,#37907,#37908,#37909,#37910,#37911,#37912,#37913,#37914,#37915,#37916,
#37917,#37918,#37919,#37920,#37921,#37922,#37923,#37924,#37925,#37926,#37927),
 .UNSPECIFIED.,.F.,.F.,(4,3,3,3,3,3,3,3,3,3,3,3,3,3,3,3,3,3,3,3,3,3,3,3,
3,3,3,3,3,3,3,3,3,3,3,3,3,3,4),(-1.36927609592744,-1.32188407678276,-1.27030325921983,
-1.23707822338756,-1.21785653354656,-1.20762469155833,-1.20007327197696,
-1.14735554346642,-1.09412617616831,-1.04931457436499,-1.04159068704494,
-1.03430007789804,-1.00450297256166,-0.950888266553232,-0.896804719012292,
-0.84212054699549,-0.801107417982889,-0.789867050267934,-0.783408395762924,
-0.728461154848662,-0.678068030945084,-0.623694406361887,-0.56893024176975,
-0.540708132259289,-0.532050527890794,-0.526074465591946,-0.47096550523936,
-0.415386732454638,-0.359836412657358,-0.34315336568606,-0.300259194975303,
-0.281492995289346,-0.271248085891861,-0.263224157987078,-0.207778571445273,
-0.151390901525645,-0.0948961475312077,-0.0389343418600114,0.),
 .UNSPECIFIED.);
#4986=B_SPLINE_CURVE_WITH_KNOTS('',3,(#37928,#37929,#37930,#37931,#37932,
#37933),.UNSPECIFIED.,.F.,.F.,(4,1,1,4),(13.172247709466,14.0943733067152,
15.0922014637835,15.7079632679498),.UNSPECIFIED.);
#4987=B_SPLINE_CURVE_WITH_KNOTS('',3,(#37936,#37937,#37938,#37939,#37940,
#37941,#37942,#37943,#37944,#37945,#37946,#37947,#37948,#37949,#37950,#37951,
#37952,#37953,#37954,#37955,#37956,#37957,#37958,#37959,#37960,#37961,#37962,
#37963,#37964,#37965,#37966,#37967,#37968,#37969,#37970,#37971,#37972,#37973,
#37974,#37975,#37976,#37977,#37978,#37979,#37980,#37981,#37982,#37983,#37984,
#37985,#37986,#37987,#37988,#37989,#37990,#37991,#37992,#37993,#37994,#37995,
#37996,#37997,#37998,#37999,#38000,#38001,#38002,#38003,#38004,#38005,#38006,
#38007,#38008,#38009,#38010,#38011,#38012,#38013,#38014,#38015,#38016,#38017,
#38018,#38019,#38020,#38021,#38022,#38023,#38024,#38025,#38026,#38027,#38028,
#38029,#38030,#38031,#38032,#38033,#38034,#38035,#38036,#38037,#38038,#38039,
#38040,#38041,#38042,#38043,#38044,#38045,#38046,#38047,#38048,#38049,#38050),
 .UNSPECIFIED.,.F.,.F.,(4,3,3,3,3,3,3,3,3,3,3,3,3,3,3,3,3,3,3,3,3,3,3,3,
3,3,3,3,3,3,3,3,3,3,3,3,3,3,4),(-1.36616069392051,-1.31376192804741,-1.25760160853096,
-1.2220458993502,-1.20367987891242,-1.19122237324406,-1.1821195135026,-1.12620867561135,
-1.07028337760104,-1.02171965634293,-1.01246054749485,-1.00560804142907,
-0.973155935084823,-0.917891839934146,-0.862525668228774,-0.806980972135536,
-0.765322450065607,-0.75160971907717,-0.74437332928858,-0.690070032095365,
-0.64034688385582,-0.585898585517151,-0.531637706406087,-0.504668943518871,
-0.497129767239748,-0.490727295531997,-0.437156216738527,-0.383621581401278,
-0.330780908606657,-0.315887603308359,-0.276401652894814,-0.259126549588888,
-0.248755897909084,-0.240651077132608,-0.188174525113787,-0.135375645789863,
-0.0828505829447398,-0.0312642027293569,0.),.UNSPECIFIED.);
#4988=B_SPLINE_CURVE_WITH_KNOTS('',3,(#38053,#38054,#38055,#38056,#38057,
#38058),.UNSPECIFIED.,.F.,.F.,(4,1,1,4),(14.4112373819487,14.9101514604828,
15.4090655390169,15.7079632679497),.UNSPECIFIED.);
#4989=B_SPLINE_CURVE_WITH_KNOTS('',3,(#40111,#40112,#40113,#40114,#40115,
#40116,#40117,#40118,#40119,#40120,#40121,#40122,#40123,#40124,#40125,#40126,
#40127,#40128,#40129),.UNSPECIFIED.,.F.,.F.,(4,3,3,3,3,3,4),(-394.142122041962,
-393.643207963428,-393.144293884893,-392.645379806359,-392.146465727825,
-391.148637570757,-390.854214931135),.UNSPECIFIED.);
#4990=B_SPLINE_CURVE_WITH_KNOTS('',3,(#40132,#40133,#40134,#40135,#40136,
#40137,#40138,#40139,#40140,#40141,#40142,#40143,#40144,#40145,#40146,#40147,
#40148,#40149,#40150,#40151,#40152,#40153,#40154,#40155,#40156,#40157,#40158,
#40159,#40160,#40161,#40162,#40163,#40164,#40165,#40166,#40167,#40168,#40169,
#40170,#40171,#40172,#40173,#40174,#40175,#40176,#40177,#40178,#40179,#40180,
#40181,#40182,#40183,#40184,#40185,#40186,#40187,#40188,#40189,#40190,#40191,
#40192,#40193,#40194,#40195,#40196,#40197,#40198,#40199,#40200,#40201,#40202,
#40203,#40204,#40205,#40206,#40207,#40208,#40209,#40210,#40211,#40212,#40213,
#40214,#40215,#40216,#40217,#40218,#40219,#40220,#40221,#40222,#40223,#40224,
#40225,#40226,#40227,#40228,#40229,#40230,#40231,#40232,#40233,#40234,#40235,
#40236,#40237,#40238,#40239,#40240,#40241,#40242,#40243),.UNSPECIFIED.,
 .F.,.F.,(4,3,3,3,3,3,3,3,3,3,3,3,3,3,3,3,3,3,3,3,3,3,3,3,3,3,3,3,3,3,3,
3,3,3,3,3,3,4),(-1.36927609592741,-1.31976302467547,-1.2674742744568,-1.23439849328534,
-1.21163835138631,-1.20085128479468,-1.14769397227967,-1.09436197408657,
-1.04861499958584,-1.04164621982373,-1.03428540169754,-1.00286802508512,
-0.949812476279694,-0.896070170266004,-0.841289386086885,-0.800203797952546,
-0.788785995023541,-0.782022675529197,-0.727256626595045,-0.67694703354953,
-0.622431301271701,-0.567625470663003,-0.539494668235961,-0.53224730158684,
-0.526366577252169,-0.471123972311258,-0.415492601545496,-0.359953143368869,
-0.342579051246667,-0.299756669840834,-0.281021877975781,-0.270604933475851,
-0.263553420126647,-0.20815816146705,-0.151770314335523,-0.0952750360977028,
-0.03935989507387,0.),.UNSPECIFIED.);
#4991=B_SPLINE_CURVE_WITH_KNOTS('',3,(#40248,#40249,#40250,#40251,#40252,
#40253,#40254,#40255,#40256,#40257,#40258,#40259,#40260,#40261,#40262,#40263,
#40264,#40265,#40266,#40267,#40268,#40269,#40270,#40271,#40272,#40273,#40274,
#40275,#40276,#40277,#40278,#40279,#40280,#40281,#40282,#40283,#40284,#40285,
#40286,#40287,#40288,#40289,#40290,#40291,#40292,#40293,#40294,#40295,#40296,
#40297,#40298,#40299,#40300,#40301,#40302,#40303,#40304,#40305,#40306,#40307,
#40308,#40309,#40310,#40311,#40312,#40313,#40314,#40315,#40316,#40317,#40318,
#40319,#40320,#40321,#40322,#40323,#40324,#40325,#40326,#40327,#40328,#40329,
#40330,#40331,#40332,#40333,#40334,#40335,#40336,#40337,#40338,#40339,#40340,
#40341,#40342,#40343,#40344,#40345,#40346,#40347,#40348,#40349,#40350,#40351,
#40352,#40353,#40354,#40355,#40356,#40357,#40358,#40359,#40360,#40361,#40362),
 .UNSPECIFIED.,.F.,.F.,(4,3,3,3,3,3,3,3,3,3,3,3,3,3,3,3,3,3,3,3,3,3,3,3,
3,3,3,3,3,3,3,3,3,3,3,3,3,3,4),(-1.36616069392046,-1.31142638897199,-1.25498626984362,
-1.21954375073289,-1.19734069803303,-1.18767642039703,-1.17959396109305,
-1.12369342935424,-1.06807187425649,-1.01975899560714,-1.01204767220352,
-1.00441384808788,-0.97144611695779,-0.91645908715266,-0.861167890840583,
-0.805684136616207,-0.764071320947925,-0.752912961187079,-0.746308512839135,
-0.691965003401675,-0.63923287394308,-0.584768581393643,-0.530513315239903,
-0.503617313135893,-0.496026441221278,-0.48914350076485,-0.435553954734991,
-0.382024894959837,-0.329152210381291,-0.315345298407825,-0.275927136106847,
-0.258681690100169,-0.24846788515743,-0.240610235241747,-0.188114192777283,
-0.135324807824555,-0.0828541010340507,-0.0314047502190577,0.),
 .UNSPECIFIED.);
#4992=B_SPLINE_CURVE_WITH_KNOTS('',3,(#41199,#41200,#41201,#41202,#41203,
#41204,#41205,#41206,#41207,#41208,#41209,#41210,#41211,#41212,#41213,#41214,
#41215,#41216,#41217,#41218,#41219,#41220,#41221,#41222,#41223,#41224,#41225,
#41226,#41227,#41228,#41229,#41230,#41231,#41232,#41233,#41234,#41235),
 .UNSPECIFIED.,.F.,.F.,(4,3,3,3,3,3,3,3,3,3,3,3,4),(95.0849428558252,95.1312807944966,
95.6293503274521,96.1274198604076,96.6254893933631,97.1235589263185,97.621628459274,
98.1196979922295,98.617767525185,99.1158370581404,99.6139065910959,100.111976124051,
100.530964914873),.UNSPECIFIED.);
#4993=B_SPLINE_CURVE_WITH_KNOTS('',3,(#41237,#41238,#41239,#41240,#41241,
#41242,#41243,#41244,#41245,#41246,#41247,#41248,#41249,#41250,#41251,#41252,
#41253,#41254,#41255,#41256,#41257,#41258,#41259,#41260,#41261,#41262,#41263,
#41264,#41265,#41266,#41267,#41268,#41269,#41270,#41271,#41272,#41273,#41274,
#41275,#41276,#41277,#41278,#41279,#41280,#41281,#41282,#41283,#41284,#41285,
#41286,#41287,#41288,#41289,#41290,#41291,#41292,#41293,#41294,#41295,#41296,
#41297,#41298,#41299,#41300,#41301,#41302,#41303,#41304,#41305,#41306,#41307,
#41308,#41309,#41310,#41311,#41312,#41313,#41314,#41315,#41316,#41317,#41318,
#41319,#41320,#41321,#41322,#41323,#41324,#41325,#41326,#41327,#41328,#41329,
#41330,#41331,#41332,#41333,#41334,#41335,#41336,#41337,#41338,#41339,#41340,
#41341,#41342,#41343,#41344,#41345,#41346,#41347,#41348),.UNSPECIFIED.,
 .F.,.F.,(4,3,3,3,3,3,3,3,3,3,3,3,3,3,3,3,3,3,3,3,3,3,3,3,3,3,3,3,3,3,3,
3,3,3,3,3,3,4),(-1.3692760959275,-1.31976302467557,-1.26747427578708,-1.23439849444934,
-1.21163835086635,-1.20085128503299,-1.14769397303989,-1.09436197457134,
-1.04861499982825,-1.04164622051909,-1.03428540176251,-1.00286802508516,
-0.949812474675958,-0.896070168269673,-0.841289384589646,-0.800203796829625,
-0.788785992753292,-0.782022674895381,-0.727256625791858,-0.676947033549563,
-0.622431298515392,-0.567625467803214,-0.539494665733644,-0.532247290384895,
-0.526366563048055,-0.471123955098454,-0.415492583526853,-0.359953130535847,
-0.342579051246657,-0.299756669840825,-0.281021877975773,-0.270604933188539,
-0.263553420220014,-0.208158173018763,-0.151770330552895,-0.0952750507295094,
-0.0393598974769998,0.),.UNSPECIFIED.);
#4994=B_SPLINE_CURVE_WITH_KNOTS('',3,(#41349,#41350,#41351,#41352,#41353,
#41354,#41355,#41356,#41357,#41358,#41359,#41360,#41361,#41362),
 .UNSPECIFIED.,.F.,.F.,(4,1,1,1,1,1,1,1,1,1,1,4),(10.6589735865933,11.0779623774152,
11.5760319103707,12.0741014433262,12.5721709762817,13.0702405092372,13.5683100421926,
14.0663795751481,14.5644491081036,15.0625186410591,15.5605881740146,15.7079632679489),
 .UNSPECIFIED.);
#4995=B_SPLINE_CURVE_WITH_KNOTS('',3,(#41365,#41366,#41367,#41368,#41369,
#41370,#41371,#41372,#41373,#41374,#41375,#41376,#41377,#41378,#41379,#41380,
#41381,#41382,#41383,#41384,#41385,#41386,#41387,#41388,#41389,#41390,#41391,
#41392,#41393,#41394,#41395,#41396,#41397,#41398,#41399,#41400,#41401,#41402,
#41403,#41404,#41405,#41406,#41407,#41408,#41409,#41410,#41411,#41412,#41413,
#41414,#41415,#41416,#41417,#41418,#41419,#41420,#41421,#41422,#41423,#41424,
#41425,#41426,#41427,#41428,#41429,#41430,#41431,#41432,#41433,#41434,#41435,
#41436,#41437,#41438,#41439,#41440,#41441,#41442,#41443,#41444,#41445,#41446,
#41447,#41448,#41449,#41450,#41451,#41452,#41453,#41454,#41455,#41456,#41457,
#41458,#41459,#41460,#41461,#41462,#41463,#41464,#41465,#41466,#41467,#41468,
#41469,#41470,#41471,#41472,#41473,#41474,#41475,#41476,#41477,#41478,#41479),
 .UNSPECIFIED.,.F.,.F.,(4,3,3,3,3,3,3,3,3,3,3,3,3,3,3,3,3,3,3,3,3,3,3,3,
3,3,3,3,3,3,3,3,3,3,3,3,3,3,4),(-1.36616069392038,-1.31142638897197,-1.25498626979377,
-1.21954375068927,-1.19734069753713,-1.18767641877559,-1.17959396063584,
-1.12369342906595,-1.06807187393295,-1.01975899544537,-1.01204767193382,
-1.00441384808241,-0.971446116957786,-0.916459086968053,-0.861167891330158,
-0.805684136983392,-0.764071321223317,-0.752912961782954,-0.746308513132906,
-0.691965005739893,-0.639232873943093,-0.584768580907417,-0.53051330855053,
-0.50361730728269,-0.496026418883006,-0.489143497419182,-0.435553950836429,
-0.382024885820224,-0.329152189052059,-0.315345298407804,-0.275927136106829,
-0.258681690100152,-0.248467885303507,-0.240610235431388,-0.188114185716531,
-0.135324804513882,-0.082854107800741,-0.0314047741919013,0.),
 .UNSPECIFIED.);
#4996=B_SPLINE_CURVE_WITH_KNOTS('',3,(#41482,#41483,#41484,#41485,#41486,
#41487,#41488,#41489,#41490,#41491,#41492),.UNSPECIFIED.,.F.,.F.,(4,1,1,
1,1,1,1,1,4),(11.897963259076,12.3960327920314,12.8941023249869,13.3921718579424,
13.8902413908979,14.3883109238534,14.8863804568088,15.3844499897643,15.7079632679489),
 .UNSPECIFIED.);
#4997=B_SPLINE_CURVE_WITH_KNOTS('',3,(#42329,#42330,#42331,#42332,#42333,
#42334,#42335,#42336,#42337,#42338,#42339,#42340,#42341,#42342,#42343,#42344,
#42345,#42346,#42347,#42348,#42349,#42350,#42351,#42352,#42353,#42354,#42355,
#42356,#42357,#42358,#42359),.UNSPECIFIED.,.F.,.F.,(4,3,3,3,3,3,3,3,3,3,
4),(-102.602323788829,-102.104254255873,-101.606184722918,-101.108115189962,
-100.610045657007,-100.111976124051,-99.6139065910959,-99.1158370581404,
-98.6177675251849,-98.1196979922295,-98.0577796165668),.UNSPECIFIED.);
#4998=B_SPLINE_CURVE_WITH_KNOTS('',3,(#42504,#42505,#42506,#42507),
 .UNSPECIFIED.,.F.,.F.,(4,4),(0.,0.0936682560791196),.UNSPECIFIED.);
#4999=B_SPLINE_CURVE_WITH_KNOTS('',3,(#42537,#42538,#42539,#42540,#42541,
#42542),.UNSPECIFIED.,.F.,.F.,(4,2,4),(0.664134112378609,0.666288650481674,
0.834782922241236),.UNSPECIFIED.);
#5000=B_SPLINE_CURVE_WITH_KNOTS('',3,(#42543,#42544,#42545,#42546),
 .UNSPECIFIED.,.F.,.F.,(4,4),(0.,1.5),.UNSPECIFIED.);
#5001=B_SPLINE_CURVE_WITH_KNOTS('',3,(#42632,#42633,#42634,#42635,#42636,
#42637,#42638),.UNSPECIFIED.,.F.,.F.,(4,3,4),(0.00777826218664459,0.048552619044639,
0.0850249535915979),.UNSPECIFIED.);
#5002=B_SPLINE_CURVE_WITH_KNOTS('',3,(#42640,#42641,#42642,#42643),
 .UNSPECIFIED.,.F.,.F.,(4,4),(0.,1.5),.UNSPECIFIED.);
#5003=B_SPLINE_CURVE_WITH_KNOTS('',3,(#42645,#42646,#42647,#42648,#42649,
#42650,#42651),.UNSPECIFIED.,.F.,.F.,(4,3,4),(0.,0.0468232933785311,0.0773537975132304),
 .UNSPECIFIED.);
#5004=B_SPLINE_CURVE_WITH_KNOTS('',3,(#42687,#42688,#42689,#42690),
 .UNSPECIFIED.,.F.,.F.,(4,4),(0.0949433903987894,0.171326334486879),
 .UNSPECIFIED.);
#5005=B_SPLINE_CURVE_WITH_KNOTS('',3,(#42696,#42697,#42698,#42699),
 .UNSPECIFIED.,.F.,.F.,(4,4),(0.,0.0936682560793217),.UNSPECIFIED.);
#5006=B_SPLINE_CURVE_WITH_KNOTS('',3,(#42704,#42705,#42706,#42707),
 .UNSPECIFIED.,.F.,.F.,(4,4),(0.,1.5),.UNSPECIFIED.);
#5007=B_SPLINE_CURVE_WITH_KNOTS('',3,(#42711,#42712,#42713,#42714),
 .UNSPECIFIED.,.F.,.F.,(4,4),(0.,0.0771717558746826),.UNSPECIFIED.);
#5008=B_SPLINE_CURVE_WITH_KNOTS('',3,(#42856,#42857,#42858,#42859),
 .UNSPECIFIED.,.F.,.F.,(4,4),(0.,0.0936682560792406),.UNSPECIFIED.);
#5009=B_SPLINE_CURVE_WITH_KNOTS('',3,(#42889,#42890,#42891,#42892,#42893,
#42894),.UNSPECIFIED.,.F.,.F.,(4,2,4),(0.66413411238557,0.666288650489319,
0.834782922257957),.UNSPECIFIED.);
#5010=B_SPLINE_CURVE_WITH_KNOTS('',3,(#42895,#42896,#42897,#42898),
 .UNSPECIFIED.,.F.,.F.,(4,4),(0.,1.5),.UNSPECIFIED.);
#5011=B_SPLINE_CURVE_WITH_KNOTS('',3,(#43018,#43019,#43020,#43021),
 .UNSPECIFIED.,.F.,.F.,(4,4),(0.0949433903987529,0.171326334486776),
 .UNSPECIFIED.);
#5012=B_SPLINE_CURVE_WITH_KNOTS('',3,(#43026,#43027,#43028,#43029),
 .UNSPECIFIED.,.F.,.F.,(4,4),(0.,1.5),.UNSPECIFIED.);
#5013=B_SPLINE_CURVE_WITH_KNOTS('',3,(#43033,#43034,#43035,#43036),
 .UNSPECIFIED.,.F.,.F.,(4,4),(0.,0.0771717558741193),.UNSPECIFIED.);
#5014=B_SPLINE_CURVE_WITH_KNOTS('',3,(#43178,#43179,#43180,#43181),
 .UNSPECIFIED.,.F.,.F.,(4,4),(0.,0.0936682560792162),.UNSPECIFIED.);
#5015=B_SPLINE_CURVE_WITH_KNOTS('',3,(#43211,#43212,#43213,#43214,#43215,
#43216),.UNSPECIFIED.,.F.,.F.,(4,2,4),(0.664134112375963,0.666288650477681,
0.834782922235844),.UNSPECIFIED.);
#5016=B_SPLINE_CURVE_WITH_KNOTS('',3,(#43217,#43218,#43219,#43220),
 .UNSPECIFIED.,.F.,.F.,(4,4),(0.,1.5),.UNSPECIFIED.);
#5017=B_SPLINE_CURVE_WITH_KNOTS('',3,(#43340,#43341,#43342,#43343),
 .UNSPECIFIED.,.F.,.F.,(4,4),(0.0895792937411446,0.166038797206149),
 .UNSPECIFIED.);
#5018=B_SPLINE_CURVE_WITH_KNOTS('',3,(#43348,#43349,#43350,#43351),
 .UNSPECIFIED.,.F.,.F.,(4,4),(0.,1.5),.UNSPECIFIED.);
#5019=B_SPLINE_CURVE_WITH_KNOTS('',3,(#43355,#43356,#43357,#43358),
 .UNSPECIFIED.,.F.,.F.,(4,4),(0.,0.0771946366775442),.UNSPECIFIED.);
#5020=B_SPLINE_CURVE_WITH_KNOTS('',3,(#43500,#43501,#43502,#43503),
 .UNSPECIFIED.,.F.,.F.,(4,4),(0.,0.0936682560793148),.UNSPECIFIED.);
#5021=B_SPLINE_CURVE_WITH_KNOTS('',3,(#43533,#43534,#43535,#43536,#43537,
#43538),.UNSPECIFIED.,.F.,.F.,(4,2,4),(0.646941188901376,0.687030553871696,
0.838090507429105),.UNSPECIFIED.);
#5022=B_SPLINE_CURVE_WITH_KNOTS('',3,(#43539,#43540,#43541,#43542),
 .UNSPECIFIED.,.F.,.F.,(4,4),(0.,1.5),.UNSPECIFIED.);
#5023=B_SPLINE_CURVE_WITH_KNOTS('',3,(#43662,#43663,#43664,#43665),
 .UNSPECIFIED.,.F.,.F.,(4,4),(0.027979075972516,0.105105315913476),
 .UNSPECIFIED.);
#5024=B_SPLINE_CURVE_WITH_KNOTS('',3,(#43670,#43671,#43672,#43673),
 .UNSPECIFIED.,.F.,.F.,(4,4),(0.,1.5),.UNSPECIFIED.);
#5025=B_SPLINE_CURVE_WITH_KNOTS('',3,(#43677,#43678,#43679,#43680),
 .UNSPECIFIED.,.F.,.F.,(4,4),(0.,0.0773597620762172),.UNSPECIFIED.);
#5026=B_SPLINE_CURVE_WITH_KNOTS('',3,(#43822,#43823,#43824,#43825),
 .UNSPECIFIED.,.F.,.F.,(4,4),(0.,0.093668256079297),.UNSPECIFIED.);
#5027=B_SPLINE_CURVE_WITH_KNOTS('',3,(#43855,#43856,#43857,#43858,#43859,
#43860,#43861,#43862,#43863,#43864,#43865,#43866,#43867,#43868,#43869,#43870,
#43871,#43872,#43873),.UNSPECIFIED.,.F.,.F.,(4,3,3,3,3,3,4),(0.648956304782129,
0.690807645944959,0.735062548516529,0.758873076278325,0.788602851685956,
0.813152022949223,0.816613420545173),.UNSPECIFIED.);
#5028=B_SPLINE_CURVE_WITH_KNOTS('',3,(#43874,#43875,#43876,#43877),
 .UNSPECIFIED.,.F.,.F.,(4,4),(0.,1.5),.UNSPECIFIED.);
#5029=B_SPLINE_CURVE_WITH_KNOTS('',3,(#43997,#43998,#43999,#44000),
 .UNSPECIFIED.,.F.,.F.,(4,4),(0.0949433903987678,0.171326334486587),
 .UNSPECIFIED.);
#5030=B_SPLINE_CURVE_WITH_KNOTS('',3,(#44005,#44006,#44007,#44008),
 .UNSPECIFIED.,.F.,.F.,(4,4),(0.,1.5),.UNSPECIFIED.);
#5031=B_SPLINE_CURVE_WITH_KNOTS('',3,(#44012,#44013,#44014,#44015),
 .UNSPECIFIED.,.F.,.F.,(4,4),(0.,0.0771717558746195),.UNSPECIFIED.);
#5032=B_SPLINE_CURVE_WITH_KNOTS('',3,(#44157,#44158,#44159,#44160),
 .UNSPECIFIED.,.F.,.F.,(4,4),(0.,0.0936682560791507),.UNSPECIFIED.);
#5033=B_SPLINE_CURVE_WITH_KNOTS('',3,(#44190,#44191,#44192,#44193,#44194,
#44195),.UNSPECIFIED.,.F.,.F.,(4,2,4),(0.664134112375084,0.66628865047855,
0.834782922233775),.UNSPECIFIED.);
#5034=B_SPLINE_CURVE_WITH_KNOTS('',3,(#44196,#44197,#44198,#44199),
 .UNSPECIFIED.,.F.,.F.,(4,4),(0.,1.5),.UNSPECIFIED.);
#5035=B_SPLINE_CURVE_WITH_KNOTS('',3,(#44319,#44320,#44321,#44322),
 .UNSPECIFIED.,.F.,.F.,(4,4),(0.0949433904009592,0.171326334491679),
 .UNSPECIFIED.);
#5036=B_SPLINE_CURVE_WITH_KNOTS('',3,(#44327,#44328,#44329,#44330),
 .UNSPECIFIED.,.F.,.F.,(4,4),(0.,1.5),.UNSPECIFIED.);
#5037=B_SPLINE_CURVE_WITH_KNOTS('',3,(#44334,#44335,#44336,#44337),
 .UNSPECIFIED.,.F.,.F.,(4,4),(0.,0.0771717558747488),.UNSPECIFIED.);
#5038=B_SPLINE_CURVE_WITH_KNOTS('',3,(#44479,#44480,#44481,#44482),
 .UNSPECIFIED.,.F.,.F.,(4,4),(0.,0.0936682560792248),.UNSPECIFIED.);
#5039=B_SPLINE_CURVE_WITH_KNOTS('',3,(#44512,#44513,#44514,#44515,#44516,
#44517),.UNSPECIFIED.,.F.,.F.,(4,2,4),(0.664134112390545,0.666288650493472,
0.834782922267389),.UNSPECIFIED.);
#5040=B_SPLINE_CURVE_WITH_KNOTS('',3,(#44518,#44519,#44520,#44521),
 .UNSPECIFIED.,.F.,.F.,(4,4),(0.,1.5),.UNSPECIFIED.);
#5041=B_SPLINE_CURVE_WITH_KNOTS('',3,(#44641,#44642,#44643,#44644),
 .UNSPECIFIED.,.F.,.F.,(4,4),(0.0415520628988323,0.118563606137955),
 .UNSPECIFIED.);
#5042=B_SPLINE_CURVE_WITH_KNOTS('',3,(#44649,#44650,#44651,#44652),
 .UNSPECIFIED.,.F.,.F.,(4,4),(0.,1.5),.UNSPECIFIED.);
#5043=B_SPLINE_CURVE_WITH_KNOTS('',3,(#44656,#44657,#44658,#44659),
 .UNSPECIFIED.,.F.,.F.,(4,4),(0.,0.0773423902580483),.UNSPECIFIED.);
#5044=B_SPLINE_CURVE_WITH_KNOTS('',3,(#44803,#44804,#44805,#44806,#44807,
#44808),.UNSPECIFIED.,.F.,.F.,(4,2,4),(0.,0.0823790100552426,0.0949061944490219),
 .UNSPECIFIED.);
#5045=B_SPLINE_CURVE_WITH_KNOTS('',3,(#44838,#44839,#44840,#44841,#44842,
#44843),.UNSPECIFIED.,.F.,.F.,(4,2,4),(0.0444437679303765,0.055294838243425,
0.103828820469121),.UNSPECIFIED.);
#5046=B_SPLINE_CURVE_WITH_KNOTS('',3,(#44844,#44845,#44846,#44847),
 .UNSPECIFIED.,.F.,.F.,(4,4),(0.,1.5),.UNSPECIFIED.);
#5047=B_SPLINE_CURVE_WITH_KNOTS('',3,(#44969,#44970,#44971,#44972),
 .UNSPECIFIED.,.F.,.F.,(4,4),(0.060413669704354,0.137235209115667),
 .UNSPECIFIED.);
#5048=B_SPLINE_CURVE_WITH_KNOTS('',3,(#44977,#44978,#44979,#44980),
 .UNSPECIFIED.,.F.,.F.,(4,4),(0.,1.5),.UNSPECIFIED.);
#5049=B_SPLINE_CURVE_WITH_KNOTS('',3,(#44984,#44985,#44986,#44987),
 .UNSPECIFIED.,.F.,.F.,(4,4),(0.,0.0772979364659118),.UNSPECIFIED.);
#5050=B_SPLINE_CURVE_WITH_KNOTS('',3,(#45129,#45130,#45131,#45132),
 .UNSPECIFIED.,.F.,.F.,(4,4),(0.,0.0936682560792101),.UNSPECIFIED.);
#5051=B_SPLINE_CURVE_WITH_KNOTS('',3,(#45162,#45163,#45164,#45165,#45166,
#45167),.UNSPECIFIED.,.F.,.F.,(4,2,4),(0.640100729216595,0.692644753706222,
0.794134458427311),.UNSPECIFIED.);
#5052=B_SPLINE_CURVE_WITH_KNOTS('',3,(#45168,#45169,#45170,#45171),
 .UNSPECIFIED.,.F.,.F.,(4,4),(0.,1.5),.UNSPECIFIED.);
#5053=B_SPLINE_CURVE_WITH_KNOTS('',3,(#45291,#45292,#45293,#45294),
 .UNSPECIFIED.,.F.,.F.,(4,4),(0.0949433903984102,0.17132633448589),
 .UNSPECIFIED.);
#5054=B_SPLINE_CURVE_WITH_KNOTS('',3,(#45299,#45300,#45301,#45302),
 .UNSPECIFIED.,.F.,.F.,(4,4),(0.,1.5),.UNSPECIFIED.);
#5055=B_SPLINE_CURVE_WITH_KNOTS('',3,(#45306,#45307,#45308,#45309),
 .UNSPECIFIED.,.F.,.F.,(4,4),(0.,0.0771717558744038),.UNSPECIFIED.);
#5056=B_SPLINE_CURVE_WITH_KNOTS('',3,(#45451,#45452,#45453,#45454),
 .UNSPECIFIED.,.F.,.F.,(4,4),(0.,0.0936682560792258),.UNSPECIFIED.);
#5057=B_SPLINE_CURVE_WITH_KNOTS('',3,(#45484,#45485,#45486,#45487,#45488,
#45489),.UNSPECIFIED.,.F.,.F.,(4,2,4),(0.664134112379071,0.666288650482174,
0.834782922244795),.UNSPECIFIED.);
#5058=B_SPLINE_CURVE_WITH_KNOTS('',3,(#45490,#45491,#45492,#45493),
 .UNSPECIFIED.,.F.,.F.,(4,4),(0.,1.5),.UNSPECIFIED.);
#5059=B_SPLINE_CURVE_WITH_KNOTS('',3,(#45613,#45614,#45615,#45616),
 .UNSPECIFIED.,.F.,.F.,(4,4),(0.0949433903977092,0.171326334484129),
 .UNSPECIFIED.);
#5060=B_SPLINE_CURVE_WITH_KNOTS('',3,(#45621,#45622,#45623,#45624),
 .UNSPECIFIED.,.F.,.F.,(4,4),(0.,1.5),.UNSPECIFIED.);
#5061=B_SPLINE_CURVE_WITH_KNOTS('',3,(#45628,#45629,#45630,#45631),
 .UNSPECIFIED.,.F.,.F.,(4,4),(0.,0.0771717558746607),.UNSPECIFIED.);
#5062=B_SPLINE_CURVE_WITH_KNOTS('',3,(#45773,#45774,#45775,#45776),
 .UNSPECIFIED.,.F.,.F.,(4,4),(0.,0.093668256079299),.UNSPECIFIED.);
#5063=B_SPLINE_CURVE_WITH_KNOTS('',3,(#45806,#45807,#45808,#45809,#45810,
#45811),.UNSPECIFIED.,.F.,.F.,(4,2,4),(0.664134112381964,0.666288650485371,
0.834782922251792),.UNSPECIFIED.);
#5064=B_SPLINE_CURVE_WITH_KNOTS('',3,(#45812,#45813,#45814,#45815),
 .UNSPECIFIED.,.F.,.F.,(4,4),(0.,1.5),.UNSPECIFIED.);
#5065=B_SPLINE_CURVE_WITH_KNOTS('',3,(#45935,#45936,#45937,#45938,#45939,
#45940,#45941),.UNSPECIFIED.,.F.,.F.,(4,3,4),(0.010983168869138,0.0518472130937835,
0.0882158993716873),.UNSPECIFIED.);
#5066=B_SPLINE_CURVE_WITH_KNOTS('',3,(#45946,#45947,#45948,#45949),
 .UNSPECIFIED.,.F.,.F.,(4,4),(0.,1.5),.UNSPECIFIED.);
#5067=B_SPLINE_CURVE_WITH_KNOTS('',3,(#45953,#45954,#45955,#45956,#45957,
#45958,#45959),.UNSPECIFIED.,.F.,.F.,(4,3,4),(0.,0.0437124803990652,0.0773577392014732),
 .UNSPECIFIED.);
#5068=B_SPLINE_CURVE_WITH_KNOTS('',3,(#46101,#46102,#46103,#46104),
 .UNSPECIFIED.,.F.,.F.,(4,4),(0.,0.0936682560792125),.UNSPECIFIED.);
#5069=B_SPLINE_CURVE_WITH_KNOTS('',3,(#46134,#46135,#46136,#46137,#46138,
#46139),.UNSPECIFIED.,.F.,.F.,(4,2,4),(0.610800819740342,0.676516947854421,
0.787792634400649),.UNSPECIFIED.);
#5070=B_SPLINE_CURVE_WITH_KNOTS('',3,(#46140,#46141,#46142,#46143),
 .UNSPECIFIED.,.F.,.F.,(4,4),(0.,1.5),.UNSPECIFIED.);
#5071=B_SPLINE_CURVE_WITH_KNOTS('',3,(#46263,#46264,#46265,#46266),
 .UNSPECIFIED.,.F.,.F.,(4,4),(0.0949433903987918,0.171326334487022),
 .UNSPECIFIED.);
#5072=B_SPLINE_CURVE_WITH_KNOTS('',3,(#46271,#46272,#46273,#46274),
 .UNSPECIFIED.,.F.,.F.,(4,4),(0.,1.5),.UNSPECIFIED.);
#5073=B_SPLINE_CURVE_WITH_KNOTS('',3,(#46278,#46279,#46280,#46281),
 .UNSPECIFIED.,.F.,.F.,(4,4),(0.,0.0771717558745271),.UNSPECIFIED.);
#5074=B_SPLINE_CURVE_WITH_KNOTS('',3,(#46423,#46424,#46425,#46426),
 .UNSPECIFIED.,.F.,.F.,(4,4),(0.,0.0936682560791833),.UNSPECIFIED.);
#5075=B_SPLINE_CURVE_WITH_KNOTS('',3,(#46456,#46457,#46458,#46459,#46460,
#46461),.UNSPECIFIED.,.F.,.F.,(4,2,4),(0.666123023340529,0.674012769702091,
0.844667464106696),.UNSPECIFIED.);
#5076=B_SPLINE_CURVE_WITH_KNOTS('',3,(#46462,#46463,#46464,#46465),
 .UNSPECIFIED.,.F.,.F.,(4,4),(0.,1.5),.UNSPECIFIED.);
#5077=B_SPLINE_CURVE_WITH_KNOTS('',3,(#46585,#46586,#46587,#46588),
 .UNSPECIFIED.,.F.,.F.,(4,4),(0.0949433904001744,0.171326334490195),
 .UNSPECIFIED.);
#5078=B_SPLINE_CURVE_WITH_KNOTS('',3,(#46593,#46594,#46595,#46596),
 .UNSPECIFIED.,.F.,.F.,(4,4),(0.,1.5),.UNSPECIFIED.);
#5079=B_SPLINE_CURVE_WITH_KNOTS('',3,(#46600,#46601,#46602,#46603),
 .UNSPECIFIED.,.F.,.F.,(4,4),(0.,0.0771717558751156),.UNSPECIFIED.);
#5080=B_SPLINE_CURVE_WITH_KNOTS('',3,(#46745,#46746,#46747,#46748),
 .UNSPECIFIED.,.F.,.F.,(4,4),(0.,0.0936682560791758),.UNSPECIFIED.);
#5081=B_SPLINE_CURVE_WITH_KNOTS('',3,(#46778,#46779,#46780,#46781,#46782,
#46783),.UNSPECIFIED.,.F.,.F.,(4,2,4),(0.6641341123862,0.666288650490994,
0.83478292226001),.UNSPECIFIED.);
#5082=B_SPLINE_CURVE_WITH_KNOTS('',3,(#46784,#46785,#46786,#46787),
 .UNSPECIFIED.,.F.,.F.,(4,4),(0.,1.5),.UNSPECIFIED.);
#5083=B_SPLINE_CURVE_WITH_KNOTS('',3,(#46907,#46908,#46909,#46910),
 .UNSPECIFIED.,.F.,.F.,(4,4),(0.0949433903985646,0.171326334486267),
 .UNSPECIFIED.);
#5084=B_SPLINE_CURVE_WITH_KNOTS('',3,(#46915,#46916,#46917,#46918),
 .UNSPECIFIED.,.F.,.F.,(4,4),(0.,1.5),.UNSPECIFIED.);
#5085=B_SPLINE_CURVE_WITH_KNOTS('',3,(#46922,#46923,#46924,#46925),
 .UNSPECIFIED.,.F.,.F.,(4,4),(0.,0.0771717558742884),.UNSPECIFIED.);
#5086=B_SPLINE_CURVE_WITH_KNOTS('',3,(#47182,#47183,#47184,#47185,#47186,
#47187),.UNSPECIFIED.,.F.,.F.,(4,2,4),(0.6641341123769,0.666288650478339,
0.834782922237864),.UNSPECIFIED.);
#5087=B_SPLINE_CURVE_WITH_KNOTS('',3,(#47188,#47189,#47190,#47191),
 .UNSPECIFIED.,.F.,.F.,(4,4),(0.,1.5),.UNSPECIFIED.);
#5088=B_SPLINE_CURVE_WITH_KNOTS('',3,(#47337,#47338,#47339,#47340,#47341,
#47342),.UNSPECIFIED.,.F.,.F.,(4,2,4),(0.30198667152271,0.315892269007964,
0.319082038667528),.UNSPECIFIED.);
#5089=B_SPLINE_CURVE_WITH_KNOTS('',3,(#47393,#47394,#47395,#47396,#47397,
#47398,#47399,#47400,#47401,#47402,#47403),.UNSPECIFIED.,.F.,.F.,(4,2,2,
3,4),(-0.0419712710900813,-0.0313437335457433,-0.0138874725471006,0.,0.00645492300733996),
 .UNSPECIFIED.);
#5090=B_SPLINE_CURVE_WITH_KNOTS('',3,(#47454,#47455,#47456,#47457,#47458,
#47459),.UNSPECIFIED.,.F.,.F.,(4,2,4),(0.471466566294365,0.474656335953928,
0.488561933439089),.UNSPECIFIED.);
#5091=B_SPLINE_CURVE_WITH_KNOTS('',3,(#47474,#47475,#47476,#47477),
 .UNSPECIFIED.,.F.,.F.,(4,4),(0.964631000010127,1.09925463072705),
 .UNSPECIFIED.);
#5092=B_SPLINE_CURVE_WITH_KNOTS('',3,(#47480,#47481,#47482,#47483),
 .UNSPECIFIED.,.F.,.F.,(4,4),(1.86383746795727,1.99846109867419),
 .UNSPECIFIED.);
#5093=B_SPLINE_CURVE_WITH_KNOTS('',3,(#47493,#47494,#47495,#47496,#47497,
#47498,#47499,#47500,#47501,#47502,#47503),.UNSPECIFIED.,.F.,.F.,(4,3,2,
2,4),(-0.00645830092897804,0.,0.0122190666797987,0.0290968711311065,0.0419019462529983),
 .UNSPECIFIED.);
#5094=B_SPLINE_CURVE_WITH_KNOTS('',3,(#47602,#47603,#47604,#47605,#47606,
#47607,#47608,#47609,#47610,#47611,#47612),.UNSPECIFIED.,.F.,.F.,(4,3,2,
2,4),(-0.00645830092897708,0.,0.012219066679791,0.0290968711310762,0.041901946252941),
 .UNSPECIFIED.);
#5095=B_SPLINE_CURVE_WITH_KNOTS('',3,(#47633,#47634,#47635,#47636),
 .UNSPECIFIED.,.F.,.F.,(4,4),(0.964631000010129,1.09925463072705),
 .UNSPECIFIED.);
#5096=B_SPLINE_CURVE_WITH_KNOTS('',3,(#47640,#47641,#47642,#47643),
 .UNSPECIFIED.,.F.,.F.,(4,4),(1.86383746795727,1.99846109867419),
 .UNSPECIFIED.);
#5097=B_SPLINE_CURVE_WITH_KNOTS('',3,(#47654,#47655,#47656,#47657,#47658,
#47659,#47660,#47661,#47662,#47663,#47664),.UNSPECIFIED.,.F.,.F.,(4,2,2,
3,4),(-0.0419712710901671,-0.031343733545801,-0.0138874725471113,0.,0.00645492300734379),
 .UNSPECIFIED.);
#5098=B_SPLINE_CURVE_WITH_KNOTS('',3,(#47717,#47718,#47719,#47720,#47721,
#47722,#47723,#47724),.UNSPECIFIED.,.F.,.F.,(4,2,2,4),(0.169835657785507,
0.171492731661375,0.184845562376643,0.187089348107769),.UNSPECIFIED.);
#5099=B_SPLINE_CURVE_WITH_KNOTS('',3,(#47913,#47914,#47915,#47916),
 .UNSPECIFIED.,.F.,.F.,(4,4),(0.0456172479668645,0.054374780828201),
 .UNSPECIFIED.);
#5100=B_SPLINE_CURVE_WITH_KNOTS('',3,(#47923,#47924,#47925,#47926,#47927,
#47928,#47929,#47930),.UNSPECIFIED.,.F.,.F.,(4,2,2,4),(0.339943055200166,
0.342186840931291,0.35553967164656,0.357196745522428),.UNSPECIFIED.);
#5101=B_SPLINE_CURVE_WITH_KNOTS('',3,(#47937,#47938,#47939,#47940,#47941,
#47942,#47943,#47944,#47945,#47946,#47947),.UNSPECIFIED.,.F.,.F.,(4,2,2,
3,4),(-0.0419712710900602,-0.0313437335457316,-0.0138874725471015,0.,0.0064549230073403),
 .UNSPECIFIED.);
#5102=B_SPLINE_CURVE_WITH_KNOTS('',3,(#48014,#48015,#48016,#48017,#48018,
#48019,#48020,#48021,#48022,#48023),.UNSPECIFIED.,.F.,.F.,(4,2,2,2,4),(0.23372232720254,
0.240645165240831,0.255490442096141,0.27033571895145,0.287205208370036),
 .UNSPECIFIED.);
#5103=B_SPLINE_CURVE_WITH_KNOTS('',3,(#48030,#48031,#48032,#48033,#48034,
#48035,#48036,#48037,#48038,#48039),.UNSPECIFIED.,.F.,.F.,(4,2,2,2,4),(-0.0417111144051926,
-0.0413742569498193,-0.0219183984840148,-0.00139787181587547,-0.000254064777074337),
 .UNSPECIFIED.);
#5104=B_SPLINE_CURVE_WITH_KNOTS('',3,(#48094,#48095,#48096,#48097),
 .UNSPECIFIED.,.F.,.F.,(4,4),(0.363335998515663,0.499634934734419),
 .UNSPECIFIED.);
#5105=B_SPLINE_CURVE_WITH_KNOTS('',3,(#48098,#48099,#48100,#48101),
 .UNSPECIFIED.,.F.,.F.,(4,4),(-0.499634934734419,-0.363335998515663),
 .UNSPECIFIED.);
#5106=B_SPLINE_CURVE_WITH_KNOTS('',3,(#48137,#48138,#48139,#48140),
 .UNSPECIFIED.,.F.,.F.,(4,4),(-0.0923903836946144,0.),.UNSPECIFIED.);
#5107=B_SPLINE_CURVE_WITH_KNOTS('',3,(#48148,#48149,#48150,#48151,#48152,
#48153,#48154,#48155,#48156,#48157,#48158,#48159,#48160,#48161),
 .UNSPECIFIED.,.F.,.F.,(4,2,2,2,2,2,4),(-0.224987174815843,-0.22451346339712,
-0.196761712223143,-0.16971876072295,-0.144143929728093,-0.124672759657506,
-0.107525143255139),.UNSPECIFIED.);
#5108=B_SPLINE_CURVE_WITH_KNOTS('',3,(#48165,#48166,#48167,#48168,#48169,
#48170,#48171,#48172,#48173,#48174),.UNSPECIFIED.,.F.,.F.,(4,2,2,2,4),(0.233722327202539,
0.24064516524083,0.255490442096139,0.270335718951448,0.287205208370034),
 .UNSPECIFIED.);
#5109=B_SPLINE_CURVE_WITH_KNOTS('',3,(#48178,#48179,#48180,#48181,#48182,
#48183,#48184,#48185,#48186,#48187),.UNSPECIFIED.,.F.,.F.,(4,2,2,2,4),(-0.0417109259698474,
-0.0413740649215941,-0.021971461689753,-0.00144737185821615,-0.000254064846037182),
 .UNSPECIFIED.);
#5110=B_SPLINE_CURVE_WITH_KNOTS('',3,(#48194,#48195,#48196,#48197,#48198,
#48199),.UNSPECIFIED.,.F.,.F.,(4,2,4),(-0.190951927958331,0.,0.00159258460364357),
 .UNSPECIFIED.);
#5111=B_SPLINE_CURVE_WITH_KNOTS('',3,(#48209,#48210,#48211,#48212),
 .UNSPECIFIED.,.F.,.F.,(4,4),(0.112297946941942,0.113633052740004),
 .UNSPECIFIED.);
#5112=B_SPLINE_CURVE_WITH_KNOTS('',3,(#48220,#48221,#48222,#48223),
 .UNSPECIFIED.,.F.,.F.,(4,4),(0.0372440833740091,0.041304702596258),
 .UNSPECIFIED.);
#5113=B_SPLINE_CURVE_WITH_KNOTS('',3,(#48227,#48228,#48229,#48230,#48231,
#48232),.UNSPECIFIED.,.F.,.F.,(4,2,4),(0.0372440833834408,0.0623721844208971,
0.0947431788431503),.UNSPECIFIED.);
#5114=B_SPLINE_CURVE_WITH_KNOTS('',3,(#48238,#48239,#48240,#48241,#48242,
#48243,#48244,#48245,#48246,#48247),.UNSPECIFIED.,.F.,.F.,(4,2,2,2,4),(0.133960440718842,
0.134063881015114,0.159415678018092,0.18476747502107,0.205333050889553),
 .UNSPECIFIED.);
#5115=B_SPLINE_CURVE_WITH_KNOTS('',3,(#48254,#48255,#48256,#48257,#48258,
#48259,#48260,#48261,#48262,#48263,#48264,#48265,#48266,#48267),
 .UNSPECIFIED.,.F.,.F.,(4,2,2,2,2,2,4),(-0.224987174750142,-0.224513463331962,
-0.196761712162241,-0.169718760666431,-0.144143929682433,-0.124672759619459,
-0.107525143228149),.UNSPECIFIED.);
#5116=B_SPLINE_CURVE_WITH_KNOTS('',3,(#48268,#48269,#48270,#48271,#48272,
#48273,#48274,#48275,#48276,#48277),.UNSPECIFIED.,.F.,.F.,(4,2,2,2,4),(-0.0530664398487118,
-0.0526203138668234,-0.0265376315324865,-0.00211254843584519,-0.000314678867370228),
 .UNSPECIFIED.);
#5117=B_SPLINE_CURVE_WITH_KNOTS('',3,(#48309,#48310,#48311,#48312),
 .UNSPECIFIED.,.F.,.F.,(4,4),(-0.136299039595008,0.),.UNSPECIFIED.);
#5118=B_SPLINE_CURVE_WITH_KNOTS('',3,(#48315,#48316,#48317,#48318),
 .UNSPECIFIED.,.F.,.F.,(4,4),(0.,0.136299039595008),.UNSPECIFIED.);
#5119=B_SPLINE_CURVE_WITH_KNOTS('',3,(#48323,#48324,#48325,#48326,#48327,
#48328,#48329,#48330,#48331,#48332,#48333,#48334,#48335,#48336),
 .UNSPECIFIED.,.F.,.F.,(4,2,2,2,2,2,4),(-0.224987174736304,-0.224513463317212,
-0.196761712147415,-0.169718760651608,-0.144143929670733,-0.124672759609814,
-0.107525143222326),.UNSPECIFIED.);
#5120=B_SPLINE_CURVE_WITH_KNOTS('',3,(#48353,#48354,#48355,#48356),
 .UNSPECIFIED.,.F.,.F.,(4,4),(0.0372440833740096,0.0413047025962583),
 .UNSPECIFIED.);
#5121=B_SPLINE_CURVE_WITH_KNOTS('',3,(#48360,#48361,#48362,#48363,#48364,
#48365),.UNSPECIFIED.,.F.,.F.,(4,2,4),(0.0372440833834404,0.0623721844208965,
0.0947431788431497),.UNSPECIFIED.);
#5122=B_SPLINE_CURVE_WITH_KNOTS('',3,(#48372,#48373,#48374,#48375,#48376,
#48377,#48378,#48379),.UNSPECIFIED.,.F.,.F.,(4,2,2,4),(-0.000448465708050994,
0.,0.0249528266048236,0.0484519800048465),.UNSPECIFIED.);
#5123=B_SPLINE_CURVE_WITH_KNOTS('',3,(#48381,#48382,#48383,#48384,#48385,
#48386,#48387,#48388),.UNSPECIFIED.,.F.,.F.,(4,2,2,4),(-0.0487006899272012,
-0.0286121652027313,0.,0.000200219383804073),.UNSPECIFIED.);
#5124=B_SPLINE_CURVE_WITH_KNOTS('',3,(#48394,#48395,#48396,#48397,#48398,
#48399,#48400,#48401),.UNSPECIFIED.,.F.,.F.,(4,2,2,4),(-0.00044846570820805,
0.,0.0249528266047917,0.0484519800048519),.UNSPECIFIED.);
#5125=B_SPLINE_CURVE_WITH_KNOTS('',3,(#48403,#48404,#48405,#48406,#48407,
#48408,#48409,#48410),.UNSPECIFIED.,.F.,.F.,(4,2,2,4),(-0.0487006899269451,
-0.028612165202599,0.,0.000200219383555375),.UNSPECIFIED.);
#5126=B_SPLINE_CURVE_WITH_KNOTS('',3,(#48435,#48436,#48437,#48438),
 .UNSPECIFIED.,.F.,.F.,(4,4),(0.,0.0923903836946144),.UNSPECIFIED.);
#5127=B_SPLINE_CURVE_WITH_KNOTS('',3,(#48451,#48452,#48453,#48454,#48455,
#48456),.UNSPECIFIED.,.F.,.F.,(4,2,4),(0.0372440833834417,0.0623721844208971,
0.0947431788431506),.UNSPECIFIED.);
#5128=B_SPLINE_CURVE_WITH_KNOTS('',3,(#48461,#48462,#48463,#48464,#48465,
#48466,#48467,#48468),.UNSPECIFIED.,.F.,.F.,(4,2,2,4),(-0.0487006899272249,
-0.0286121652027421,0.,0.000200219383468989),.UNSPECIFIED.);
#5129=B_SPLINE_CURVE_WITH_KNOTS('',3,(#48473,#48474,#48475,#48476,#48477,
#48478,#48479,#48480),.UNSPECIFIED.,.F.,.F.,(4,2,2,4),(-0.0487006899264554,
-0.0286121652025119,0.,0.000200219383993128),.UNSPECIFIED.);
#5130=B_SPLINE_CURVE_WITH_KNOTS('',3,(#48502,#48503,#48504,#48505),
 .UNSPECIFIED.,.F.,.F.,(4,4),(-0.0923903843306348,0.),.UNSPECIFIED.);
#5131=B_SPLINE_CURVE_WITH_KNOTS('',3,(#48507,#48508,#48509,#48510),
 .UNSPECIFIED.,.F.,.F.,(4,4),(0.,0.0923903843306348),.UNSPECIFIED.);
#5132=B_SPLINE_CURVE_WITH_KNOTS('',3,(#48523,#48524,#48525,#48526),
 .UNSPECIFIED.,.F.,.F.,(4,4),(-0.136298877173929,0.),.UNSPECIFIED.);
#5133=B_SPLINE_CURVE_WITH_KNOTS('',3,(#48530,#48531,#48532,#48533,#48534,
#48535),.UNSPECIFIED.,.F.,.F.,(4,2,4),(0.0372440833834397,0.0623721844208972,
0.0947431788431508),.UNSPECIFIED.);
#5134=B_SPLINE_CURVE_WITH_KNOTS('',3,(#48578,#48579,#48580,#48581),
 .UNSPECIFIED.,.F.,.F.,(4,4),(0.,0.136298877173929),.UNSPECIFIED.);
#5135=B_SPLINE_CURVE_WITH_KNOTS('',3,(#48584,#48585,#48586,#48587,#48588,
#48589,#48590,#48591,#48592,#48593,#48594,#48595,#48596,#48597),
 .UNSPECIFIED.,.F.,.F.,(4,2,2,2,2,2,4),(-0.224987174812291,-0.224513463393476,
-0.196761712220003,-0.169718760720331,-0.144143929725999,-0.124672759655815,
-0.107525143253847),.UNSPECIFIED.);
#5136=B_SPLINE_CURVE_WITH_KNOTS('',3,(#48717,#48718,#48719,#48720,#48721,
#48722),.UNSPECIFIED.,.F.,.F.,(4,2,4),(0.435389141045337,0.443174934764026,
0.444151928712643),.UNSPECIFIED.);
#5137=B_SPLINE_CURVE_WITH_KNOTS('',3,(#48998,#48999,#49000,#49001),
 .UNSPECIFIED.,.F.,.F.,(4,4),(0.964631000010116,1.09925463072705),
 .UNSPECIFIED.);
#5138=B_SPLINE_CURVE_WITH_KNOTS('',3,(#49005,#49006,#49007,#49008,#49009,
#49010,#49011,#49012),.UNSPECIFIED.,.F.,.F.,(4,2,2,4),(1.86383746795725,
2.02276765578846,2.10223274970406,2.12738029118256),.UNSPECIFIED.);
#5139=B_SPLINE_CURVE_WITH_KNOTS('',3,(#49019,#49020,#49021,#49022,#49023,
#49024,#49025,#49026,#49027,#49028,#49029),.UNSPECIFIED.,.F.,.F.,(4,3,2,
2,4),(-0.00645830092897787,0.,0.0122190666797978,0.0290968711310892,0.0419019462529432),
 .UNSPECIFIED.);
#5140=B_SPLINE_CURVE_WITH_KNOTS('',3,(#49139,#49140,#49141,#49142),
 .UNSPECIFIED.,.F.,.F.,(4,4),(1.86383746795727,1.99846109867419),
 .UNSPECIFIED.);
#5141=B_SPLINE_CURVE_WITH_KNOTS('',3,(#49145,#49146,#49147,#49148,#49149,
#49150,#49151,#49152),.UNSPECIFIED.,.F.,.F.,(4,2,2,4),(0.835711807501242,
0.860859348980241,0.940324442895844,1.09925463072705),.UNSPECIFIED.);
#5142=B_SPLINE_CURVE_WITH_KNOTS('',3,(#51694,#51695,#51696,#51697,#51698,
#51699,#51700),.UNSPECIFIED.,.F.,.F.,(4,3,4),(0.,0.0297140756221973,0.0782401718747037),
 .UNSPECIFIED.);
#5143=B_SPLINE_CURVE_WITH_KNOTS('',3,(#51738,#51739,#51740,#51741,#51742,
#51743),.UNSPECIFIED.,.F.,.F.,(4,2,4),(0.,1.45,2.85),.UNSPECIFIED.);
#5144=B_SPLINE_CURVE_WITH_KNOTS('',3,(#51829,#51830,#51831,#51832,#51833,
#51834),.UNSPECIFIED.,.F.,.F.,(4,2,4),(0.924746809899207,0.981018841216537,
1.21342818548362),.UNSPECIFIED.);
#5145=B_SPLINE_CURVE_WITH_KNOTS('',3,(#51836,#51837,#51838,#51839,#51840,
#51841),.UNSPECIFIED.,.F.,.F.,(4,2,4),(0.,1.45,2.85),.UNSPECIFIED.);
#5146=B_SPLINE_CURVE_WITH_KNOTS('',3,(#51874,#51875,#51876,#51877,#51878,
#51879),.UNSPECIFIED.,.F.,.F.,(4,2,4),(0.924746809879486,0.981018841193929,
1.21342818544405),.UNSPECIFIED.);
#5147=B_SPLINE_CURVE_WITH_KNOTS('',3,(#51883,#51884,#51885,#51886,#51887,
#51888),.UNSPECIFIED.,.F.,.F.,(4,2,4),(0.,1.45,2.85),.UNSPECIFIED.);
#5148=B_SPLINE_CURVE_WITH_KNOTS('',3,(#51971,#51972,#51973,#51974,#51975,
#51976),.UNSPECIFIED.,.F.,.F.,(4,2,4),(0.,1.45,2.85),.UNSPECIFIED.);
#5149=B_SPLINE_CURVE_WITH_KNOTS('',3,(#52008,#52009,#52010,#52011,#52012,
#52013),.UNSPECIFIED.,.F.,.F.,(4,2,4),(0.924746809888898,0.981018841204197,
1.21342818545661),.UNSPECIFIED.);
#5150=B_SPLINE_CURVE_WITH_KNOTS('',3,(#52100,#52101,#52102,#52103,#52104,
#52105),.UNSPECIFIED.,.F.,.F.,(4,2,4),(0.,1.45,2.85),.UNSPECIFIED.);
#5151=B_SPLINE_CURVE_WITH_KNOTS('',3,(#52106,#52107,#52108,#52109),
 .UNSPECIFIED.,.F.,.F.,(4,4),(0.,0.0536817275864003),.UNSPECIFIED.);
#5152=B_SPLINE_CURVE_WITH_KNOTS('',3,(#54501,#54502,#54503,#54504,#54505,
#54506),.UNSPECIFIED.,.F.,.F.,(4,2,4),(0.,1.45,2.85),.UNSPECIFIED.);
#5153=B_SPLINE_CURVE_WITH_KNOTS('',3,(#54508,#54509,#54510,#54511),
 .UNSPECIFIED.,.F.,.F.,(4,4),(0.,0.0536817275781464),.UNSPECIFIED.);
#5154=B_SPLINE_CURVE_WITH_KNOTS('',3,(#54676,#54677,#54678,#54679,#54680,
#54681),.UNSPECIFIED.,.F.,.F.,(4,2,4),(0.924746809879285,0.981018841193106,
1.21342818543858),.UNSPECIFIED.);
#5155=B_SPLINE_CURVE_WITH_KNOTS('',3,(#54682,#54683,#54684,#54685,#54686,
#54687),.UNSPECIFIED.,.F.,.F.,(4,2,4),(0.,1.45,2.85),.UNSPECIFIED.);
#5156=B_SPLINE_CURVE_WITH_KNOTS('',3,(#54772,#54773,#54774,#54775,#54776,
#54777),.UNSPECIFIED.,.F.,.F.,(4,2,4),(0.,1.45,2.85),.UNSPECIFIED.);
#5157=B_SPLINE_CURVE_WITH_KNOTS('',3,(#54779,#54780,#54781,#54782,#54783,
#54784),.UNSPECIFIED.,.F.,.F.,(4,2,4),(0.0895985967037025,0.107791487575302,
0.178841206013496),.UNSPECIFIED.);
#5158=B_SPLINE_CURVE_WITH_KNOTS('',3,(#54868,#54869,#54870,#54871,#54872,
#54873),.UNSPECIFIED.,.F.,.F.,(4,2,4),(0.,1.45,2.85),.UNSPECIFIED.);
#5159=B_SPLINE_CURVE_WITH_KNOTS('',3,(#54874,#54875,#54876,#54877),
 .UNSPECIFIED.,.F.,.F.,(4,4),(0.,0.0782778812827931),.UNSPECIFIED.);
#5160=B_SPLINE_CURVE_WITH_KNOTS('',3,(#54881,#54882,#54883,#54884,#54885,
#54886),.UNSPECIFIED.,.F.,.F.,(4,2,4),(0.,1.45,2.85),.UNSPECIFIED.);
#5161=B_SPLINE_CURVE_WITH_KNOTS('',3,(#54888,#54889,#54890,#54891,#54892,
#54893,#54894,#54895,#54896,#54897),.UNSPECIFIED.,.F.,.F.,(4,3,3,4),(0.,
0.0272825353841119,0.0540089361834485,0.0724627707915405),.UNSPECIFIED.);
#5162=B_SPLINE_CURVE_WITH_KNOTS('',3,(#55062,#55063,#55064,#55065,#55066,
#55067),.UNSPECIFIED.,.F.,.F.,(4,2,4),(0.791208984971947,0.837333988005476,
1.0275823715977),.UNSPECIFIED.);
#5163=B_SPLINE_CURVE_WITH_KNOTS('',3,(#55068,#55069,#55070,#55071,#55072,
#55073),.UNSPECIFIED.,.F.,.F.,(4,2,4),(0.,1.45,2.85),.UNSPECIFIED.);
#5164=B_SPLINE_CURVE_WITH_KNOTS('',3,(#55158,#55159,#55160,#55161,#55162,
#55163),.UNSPECIFIED.,.F.,.F.,(4,2,4),(0.,1.45,2.85),.UNSPECIFIED.);
#5165=B_SPLINE_CURVE_WITH_KNOTS('',3,(#55165,#55166,#55167,#55168,#55169,
#55170),.UNSPECIFIED.,.F.,.F.,(4,2,4),(0.924746809891892,0.981018841208115,
1.21342818547153),.UNSPECIFIED.);
#5166=B_SPLINE_CURVE_WITH_KNOTS('',3,(#55254,#55255,#55256,#55257,#55258,
#55259),.UNSPECIFIED.,.F.,.F.,(4,2,4),(0.,1.45,2.85),.UNSPECIFIED.);
#5167=B_SPLINE_CURVE_WITH_KNOTS('',3,(#55260,#55261,#55262,#55263),
 .UNSPECIFIED.,.F.,.F.,(4,4),(0.,0.0536817275837366),.UNSPECIFIED.);
#5168=B_SPLINE_CURVE_WITH_KNOTS('',3,(#55267,#55268,#55269,#55270,#55271,
#55272),.UNSPECIFIED.,.F.,.F.,(4,2,4),(0.,1.45,2.85),.UNSPECIFIED.);
#5169=B_SPLINE_CURVE_WITH_KNOTS('',3,(#55274,#55275,#55276,#55277),
 .UNSPECIFIED.,.F.,.F.,(4,4),(0.,0.0536817275826949),.UNSPECIFIED.);
#5170=B_SPLINE_CURVE_WITH_KNOTS('',3,(#55442,#55443,#55444,#55445,#55446,
#55447),.UNSPECIFIED.,.F.,.F.,(4,2,4),(0.924746809881685,0.981018841196878,
1.2134281854522),.UNSPECIFIED.);
#5171=B_SPLINE_CURVE_WITH_KNOTS('',3,(#55448,#55449,#55450,#55451,#55452,
#55453),.UNSPECIFIED.,.F.,.F.,(4,2,4),(0.,1.45,2.85),.UNSPECIFIED.);
#5172=B_SPLINE_CURVE_WITH_KNOTS('',3,(#55538,#55539,#55540,#55541,#55542,
#55543),.UNSPECIFIED.,.F.,.F.,(4,2,4),(0.,1.45,2.85),.UNSPECIFIED.);
#5173=B_SPLINE_CURVE_WITH_KNOTS('',3,(#55545,#55546,#55547,#55548,#55549,
#55550),.UNSPECIFIED.,.F.,.F.,(4,2,4),(0.92474680987975,0.981018841194028,
1.21342818544147),.UNSPECIFIED.);
#5174=B_SPLINE_CURVE_WITH_KNOTS('',3,(#55634,#55635,#55636,#55637,#55638,
#55639),.UNSPECIFIED.,.F.,.F.,(4,2,4),(0.,1.45,2.85),.UNSPECIFIED.);
#5175=B_SPLINE_CURVE_WITH_KNOTS('',3,(#55640,#55641,#55642,#55643,#55644,
#55645,#55646),.UNSPECIFIED.,.F.,.F.,(4,3,4),(0.,0.0297140756203395,0.0782401718741553),
 .UNSPECIFIED.);
#5176=B_SPLINE_CURVE_WITH_KNOTS('',3,(#55650,#55651,#55652,#55653,#55654,
#55655),.UNSPECIFIED.,.F.,.F.,(4,2,4),(0.,1.45,2.85),.UNSPECIFIED.);
#5177=B_SPLINE_CURVE_WITH_KNOTS('',3,(#55657,#55658,#55659,#55660),
 .UNSPECIFIED.,.F.,.F.,(4,4),(0.,0.0536817275848442),.UNSPECIFIED.);
#5178=B_SPLINE_CURVE_WITH_KNOTS('',3,(#55825,#55826,#55827,#55828,#55829,
#55830),.UNSPECIFIED.,.F.,.F.,(4,2,4),(0.924746809894682,0.981018841211385,
1.21342818547561),.UNSPECIFIED.);
#5179=B_SPLINE_CURVE_WITH_KNOTS('',3,(#55831,#55832,#55833,#55834,#55835,
#55836),.UNSPECIFIED.,.F.,.F.,(4,2,4),(0.,1.45,2.85),.UNSPECIFIED.);
#5180=B_SPLINE_CURVE_WITH_KNOTS('',3,(#55921,#55922,#55923,#55924,#55925,
#55926),.UNSPECIFIED.,.F.,.F.,(4,2,4),(0.,1.45,2.85),.UNSPECIFIED.);
#5181=B_SPLINE_CURVE_WITH_KNOTS('',3,(#55928,#55929,#55930,#55931,#55932,
#55933),.UNSPECIFIED.,.F.,.F.,(4,2,4),(0.924746809888962,0.98101884120512,
1.21342818546788),.UNSPECIFIED.);
#5182=B_SPLINE_CURVE_WITH_KNOTS('',3,(#56017,#56018,#56019,#56020,#56021,
#56022),.UNSPECIFIED.,.F.,.F.,(4,2,4),(0.,1.45,2.85),.UNSPECIFIED.);
#5183=B_SPLINE_CURVE_WITH_KNOTS('',3,(#56023,#56024,#56025,#56026),
 .UNSPECIFIED.,.F.,.F.,(4,4),(0.,0.0536817275789145),.UNSPECIFIED.);
#5184=B_SPLINE_CURVE_WITH_KNOTS('',3,(#56030,#56031,#56032,#56033,#56034,
#56035),.UNSPECIFIED.,.F.,.F.,(4,2,4),(0.,1.45,2.85),.UNSPECIFIED.);
#5185=B_SPLINE_CURVE_WITH_KNOTS('',3,(#56037,#56038,#56039,#56040),
 .UNSPECIFIED.,.F.,.F.,(4,4),(0.,0.0782778812825522),.UNSPECIFIED.);
#5186=B_SPLINE_CURVE_WITH_KNOTS('',3,(#56205,#56206,#56207,#56208,#56209,
#56210),.UNSPECIFIED.,.F.,.F.,(4,2,4),(0.0895985966900729,0.107791487558596,
0.178841205983874),.UNSPECIFIED.);
#5187=B_SPLINE_CURVE_WITH_KNOTS('',3,(#56211,#56212,#56213,#56214,#56215,
#56216),.UNSPECIFIED.,.F.,.F.,(4,2,4),(0.,1.45,2.85),.UNSPECIFIED.);
#5188=B_SPLINE_CURVE_WITH_KNOTS('',3,(#56301,#56302,#56303,#56304,#56305,
#56306),.UNSPECIFIED.,.F.,.F.,(4,2,4),(0.,1.45,2.85),.UNSPECIFIED.);
#5189=B_SPLINE_CURVE_WITH_KNOTS('',3,(#56308,#56309,#56310,#56311,#56312,
#56313),.UNSPECIFIED.,.F.,.F.,(4,2,4),(0.791208985000826,0.837333988039583,
1.0275823716573),.UNSPECIFIED.);
#5190=B_SPLINE_CURVE_WITH_KNOTS('',3,(#56397,#56398,#56399,#56400,#56401,
#56402),.UNSPECIFIED.,.F.,.F.,(4,2,4),(0.,1.45,2.85),.UNSPECIFIED.);
#5191=B_SPLINE_CURVE_WITH_KNOTS('',3,(#56403,#56404,#56405,#56406,#56407,
#56408,#56409,#56410,#56411,#56412),.UNSPECIFIED.,.F.,.F.,(4,3,3,4),(0.,
0.0272825353828734,0.0540089361863412,0.0724627707912745),.UNSPECIFIED.);
#5192=B_SPLINE_CURVE_WITH_KNOTS('',3,(#56416,#56417,#56418,#56419,#56420,
#56421),.UNSPECIFIED.,.F.,.F.,(4,2,4),(0.,1.45,2.85),.UNSPECIFIED.);
#5193=B_SPLINE_CURVE_WITH_KNOTS('',3,(#56423,#56424,#56425,#56426),
 .UNSPECIFIED.,.F.,.F.,(4,4),(0.,0.0536817275846425),.UNSPECIFIED.);
#5194=B_SPLINE_CURVE_WITH_KNOTS('',3,(#56591,#56592,#56593,#56594,#56595,
#56596),.UNSPECIFIED.,.F.,.F.,(4,2,4),(0.924746809884044,0.981018841198511,
1.21342818544902),.UNSPECIFIED.);
#5195=B_SPLINE_CURVE_WITH_KNOTS('',3,(#56597,#56598,#56599,#56600,#56601,
#56602),.UNSPECIFIED.,.F.,.F.,(4,2,4),(0.,1.45,2.85),.UNSPECIFIED.);
#5196=B_SPLINE_CURVE_WITH_KNOTS('',3,(#56687,#56688,#56689,#56690),
 .UNSPECIFIED.,.F.,.F.,(4,4),(0.,0.053681727571403),.UNSPECIFIED.);
#5197=B_SPLINE_CURVE_WITH_KNOTS('',3,(#56692,#56693,#56694,#56695,#56696,
#56697),.UNSPECIFIED.,.F.,.F.,(4,2,4),(0.,1.45,2.85),.UNSPECIFIED.);
#5198=B_SPLINE_CURVE_WITH_KNOTS('',3,(#56861,#56862,#56863,#56864),
 .UNSPECIFIED.,.F.,.F.,(4,4),(0.,0.0942418390735999),.UNSPECIFIED.);
#5199=B_SPLINE_CURVE_WITH_KNOTS('',3,(#56867,#56868,#56869,#56870,#56871,
#56872),.UNSPECIFIED.,.F.,.F.,(4,2,4),(0.336411782332586,0.341442004890514,
0.473061015913503),.UNSPECIFIED.);
#5200=B_SPLINE_CURVE_WITH_KNOTS('',3,(#56873,#56874,#56875,#56876),
 .UNSPECIFIED.,.F.,.F.,(4,4),(0.,1.5),.UNSPECIFIED.);
#5201=B_SPLINE_CURVE_WITH_KNOTS('',3,(#56960,#56961,#56962,#56963,#56964,
#56965,#56966,#56967,#56968,#56969),.UNSPECIFIED.,.F.,.F.,(4,3,3,4),(0.00555547746779166,
0.0431313379163893,0.0740617625597658,0.080707198364987),.UNSPECIFIED.);
#5202=B_SPLINE_CURVE_WITH_KNOTS('',3,(#56971,#56972,#56973,#56974),
 .UNSPECIFIED.,.F.,.F.,(4,4),(0.,1.5),.UNSPECIFIED.);
#5203=B_SPLINE_CURVE_WITH_KNOTS('',3,(#56975,#56976,#56977,#56978,#56979,
#56980,#56981,#56982,#56983,#56984),.UNSPECIFIED.,.F.,.F.,(4,3,3,4),(0.,
0.0325402337502392,0.0706876468156212,0.074495117381235),.UNSPECIFIED.);
#5204=B_SPLINE_CURVE_WITH_KNOTS('',3,(#56988,#56989,#56990,#56991),
 .UNSPECIFIED.,.F.,.F.,(4,4),(0.100001236859483,0.210043570655993),
 .UNSPECIFIED.);
#5205=B_SPLINE_CURVE_WITH_KNOTS('',3,(#56995,#56996,#56997,#56998),
 .UNSPECIFIED.,.F.,.F.,(4,4),(0.,1.5),.UNSPECIFIED.);
#5206=B_SPLINE_CURVE_WITH_KNOTS('',3,(#57000,#57001,#57002,#57003),
 .UNSPECIFIED.,.F.,.F.,(4,4),(0.,0.0623435089195132),.UNSPECIFIED.);
#5207=B_SPLINE_CURVE_WITH_KNOTS('',3,(#57085,#57086,#57087,#57088),
 .UNSPECIFIED.,.F.,.F.,(4,4),(0.,0.0942418390734902),.UNSPECIFIED.);
#5208=B_SPLINE_CURVE_WITH_KNOTS('',3,(#57091,#57092,#57093,#57094,#57095,
#57096),.UNSPECIFIED.,.F.,.F.,(4,2,4),(0.811792901815019,0.910057458243994,
1.10441658254866),.UNSPECIFIED.);
#5209=B_SPLINE_CURVE_WITH_KNOTS('',3,(#57097,#57098,#57099,#57100),
 .UNSPECIFIED.,.F.,.F.,(4,4),(0.,1.5),.UNSPECIFIED.);
#5210=B_SPLINE_CURVE_WITH_KNOTS('',3,(#57186,#57187,#57188,#57189),
 .UNSPECIFIED.,.F.,.F.,(4,4),(0.102444446506542,0.212752916833154),
 .UNSPECIFIED.);
#5211=B_SPLINE_CURVE_WITH_KNOTS('',3,(#57193,#57194,#57195,#57196),
 .UNSPECIFIED.,.F.,.F.,(4,4),(0.,1.5),.UNSPECIFIED.);
#5212=B_SPLINE_CURVE_WITH_KNOTS('',3,(#57198,#57199,#57200,#57201),
 .UNSPECIFIED.,.F.,.F.,(4,4),(0.,0.0624333513906016),.UNSPECIFIED.);
#5213=B_SPLINE_CURVE_WITH_KNOTS('',3,(#57283,#57284,#57285,#57286),
 .UNSPECIFIED.,.F.,.F.,(4,4),(0.,0.0942418390735364),.UNSPECIFIED.);
#5214=B_SPLINE_CURVE_WITH_KNOTS('',3,(#57289,#57290,#57291,#57292,#57293,
#57294),.UNSPECIFIED.,.F.,.F.,(4,2,4),(0.813847978397809,0.909406578862909,
1.10554196286624),.UNSPECIFIED.);
#5215=B_SPLINE_CURVE_WITH_KNOTS('',3,(#57295,#57296,#57297,#57298),
 .UNSPECIFIED.,.F.,.F.,(4,4),(0.,1.5),.UNSPECIFIED.);
#5216=B_SPLINE_CURVE_WITH_KNOTS('',3,(#57384,#57385,#57386,#57387),
 .UNSPECIFIED.,.F.,.F.,(4,4),(0.102444446504211,0.212752916831367),
 .UNSPECIFIED.);
#5217=B_SPLINE_CURVE_WITH_KNOTS('',3,(#57391,#57392,#57393,#57394),
 .UNSPECIFIED.,.F.,.F.,(4,4),(0.,1.5),.UNSPECIFIED.);
#5218=B_SPLINE_CURVE_WITH_KNOTS('',3,(#57396,#57397,#57398,#57399),
 .UNSPECIFIED.,.F.,.F.,(4,4),(0.,0.0624333513927156),.UNSPECIFIED.);
#5219=B_SPLINE_CURVE_WITH_KNOTS('',3,(#57481,#57482,#57483,#57484),
 .UNSPECIFIED.,.F.,.F.,(4,4),(0.,0.0942418390735309),.UNSPECIFIED.);
#5220=B_SPLINE_CURVE_WITH_KNOTS('',3,(#57487,#57488,#57489,#57490,#57491,
#57492),.UNSPECIFIED.,.F.,.F.,(4,2,4),(0.813847978500005,0.909406579009422,
1.10554196310352),.UNSPECIFIED.);
#5221=B_SPLINE_CURVE_WITH_KNOTS('',3,(#57493,#57494,#57495,#57496),
 .UNSPECIFIED.,.F.,.F.,(4,4),(0.,1.5),.UNSPECIFIED.);
#5222=B_SPLINE_CURVE_WITH_KNOTS('',3,(#57582,#57583,#57584,#57585),
 .UNSPECIFIED.,.F.,.F.,(4,4),(0.102444446507355,0.212752916840295),
 .UNSPECIFIED.);
#5223=B_SPLINE_CURVE_WITH_KNOTS('',3,(#57589,#57590,#57591,#57592),
 .UNSPECIFIED.,.F.,.F.,(4,4),(0.,1.5),.UNSPECIFIED.);
#5224=B_SPLINE_CURVE_WITH_KNOTS('',3,(#57594,#57595,#57596,#57597),
 .UNSPECIFIED.,.F.,.F.,(4,4),(0.,0.0624333513891726),.UNSPECIFIED.);
#5225=B_SPLINE_CURVE_WITH_KNOTS('',3,(#57679,#57680,#57681,#57682),
 .UNSPECIFIED.,.F.,.F.,(4,4),(0.,0.094241839073544),.UNSPECIFIED.);
#5226=B_SPLINE_CURVE_WITH_KNOTS('',3,(#57685,#57686,#57687,#57688,#57689,
#57690),.UNSPECIFIED.,.F.,.F.,(4,2,4),(0.813847978462672,0.909406578962002,
1.10554196303347),.UNSPECIFIED.);
#5227=B_SPLINE_CURVE_WITH_KNOTS('',3,(#57691,#57692,#57693,#57694),
 .UNSPECIFIED.,.F.,.F.,(4,4),(0.,1.5),.UNSPECIFIED.);
#5228=B_SPLINE_CURVE_WITH_KNOTS('',3,(#57780,#57781,#57782,#57783),
 .UNSPECIFIED.,.F.,.F.,(4,4),(0.102444446505091,0.212752916823378),
 .UNSPECIFIED.);
#5229=B_SPLINE_CURVE_WITH_KNOTS('',3,(#57787,#57788,#57789,#57790),
 .UNSPECIFIED.,.F.,.F.,(4,4),(0.,1.5),.UNSPECIFIED.);
#5230=B_SPLINE_CURVE_WITH_KNOTS('',3,(#57792,#57793,#57794,#57795),
 .UNSPECIFIED.,.F.,.F.,(4,4),(0.,0.0624333513861405),.UNSPECIFIED.);
#5231=B_SPLINE_CURVE_WITH_KNOTS('',3,(#57877,#57878,#57879,#57880),
 .UNSPECIFIED.,.F.,.F.,(4,4),(0.,0.0942418390734816),.UNSPECIFIED.);
#5232=B_SPLINE_CURVE_WITH_KNOTS('',3,(#57883,#57884,#57885,#57886,#57887,
#57888),.UNSPECIFIED.,.F.,.F.,(4,2,4),(0.813847978451045,0.909406578940421,
1.10554196299329),.UNSPECIFIED.);
#5233=B_SPLINE_CURVE_WITH_KNOTS('',3,(#57889,#57890,#57891,#57892),
 .UNSPECIFIED.,.F.,.F.,(4,4),(0.,1.5),.UNSPECIFIED.);
#5234=B_SPLINE_CURVE_WITH_KNOTS('',3,(#57978,#57979,#57980,#57981,#57982,
#57983,#57984,#57985,#57986,#57987),.UNSPECIFIED.,.F.,.F.,(4,3,3,4),(0.00477610030196731,
0.0423460197867061,0.0734754921810407,0.079915939271445),.UNSPECIFIED.);
#5235=B_SPLINE_CURVE_WITH_KNOTS('',3,(#57991,#57992,#57993,#57994),
 .UNSPECIFIED.,.F.,.F.,(4,4),(0.,1.5),.UNSPECIFIED.);
#5236=B_SPLINE_CURVE_WITH_KNOTS('',3,(#57996,#57997,#57998,#57999,#58000,
#58001,#58002,#58003,#58004,#58005),.UNSPECIFIED.,.F.,.F.,(4,3,3,4),(0.,
0.0327390254020849,0.0706978041544828,0.0745133058834629),.UNSPECIFIED.);
#5237=B_SPLINE_CURVE_WITH_KNOTS('',3,(#58087,#58088,#58089,#58090,#58091,
#58092),.UNSPECIFIED.,.F.,.F.,(4,2,4),(0.,0.0726060447861878,0.0941220646064719),
 .UNSPECIFIED.);
#5238=B_SPLINE_CURVE_WITH_KNOTS('',3,(#58095,#58096,#58097,#58098,#58099,
#58100,#58101,#58102,#58103,#58104,#58105,#58106,#58107,#58108,#58109,#58110,
#58111,#58112,#58113),.UNSPECIFIED.,.F.,.F.,(4,3,3,3,3,3,4),(0.0359490020947758,
0.0514463139246939,0.0621647509937864,0.0701407164412387,0.0817621854071257,
0.0922147861198435,0.0991326682752126),.UNSPECIFIED.);
#5239=B_SPLINE_CURVE_WITH_KNOTS('',3,(#58114,#58115,#58116,#58117),
 .UNSPECIFIED.,.F.,.F.,(4,4),(0.,1.5),.UNSPECIFIED.);
#5240=B_SPLINE_CURVE_WITH_KNOTS('',3,(#58203,#58204,#58205,#58206),
 .UNSPECIFIED.,.F.,.F.,(4,4),(0.0684253031638949,0.146459794934132),
 .UNSPECIFIED.);
#5241=B_SPLINE_CURVE_WITH_KNOTS('',3,(#58210,#58211,#58212,#58213),
 .UNSPECIFIED.,.F.,.F.,(4,4),(0.,1.5),.UNSPECIFIED.);
#5242=B_SPLINE_CURVE_WITH_KNOTS('',3,(#58215,#58216,#58217,#58218),
 .UNSPECIFIED.,.F.,.F.,(4,4),(0.,0.0743296555811839),.UNSPECIFIED.);
#5243=B_SPLINE_CURVE_WITH_KNOTS('',3,(#58300,#58301,#58302,#58303),
 .UNSPECIFIED.,.F.,.F.,(4,4),(0.,0.0942418390734843),.UNSPECIFIED.);
#5244=B_SPLINE_CURVE_WITH_KNOTS('',3,(#58306,#58307,#58308,#58309,#58310,
#58311),.UNSPECIFIED.,.F.,.F.,(4,2,4),(0.780516546471215,0.880889879619728,
1.03952845678898),.UNSPECIFIED.);
#5245=B_SPLINE_CURVE_WITH_KNOTS('',3,(#58312,#58313,#58314,#58315),
 .UNSPECIFIED.,.F.,.F.,(4,4),(0.,1.5),.UNSPECIFIED.);
#5246=B_SPLINE_CURVE_WITH_KNOTS('',3,(#58401,#58402,#58403,#58404),
 .UNSPECIFIED.,.F.,.F.,(4,4),(0.102444446506539,0.212752916832809),
 .UNSPECIFIED.);
#5247=B_SPLINE_CURVE_WITH_KNOTS('',3,(#58408,#58409,#58410,#58411),
 .UNSPECIFIED.,.F.,.F.,(4,4),(0.,1.5),.UNSPECIFIED.);
#5248=B_SPLINE_CURVE_WITH_KNOTS('',3,(#58413,#58414,#58415,#58416),
 .UNSPECIFIED.,.F.,.F.,(4,4),(0.,0.0624333513889912),.UNSPECIFIED.);
#5249=B_SPLINE_CURVE_WITH_KNOTS('',3,(#58498,#58499,#58500,#58501),
 .UNSPECIFIED.,.F.,.F.,(4,4),(0.,0.0942418390729746),.UNSPECIFIED.);
#5250=B_SPLINE_CURVE_WITH_KNOTS('',3,(#58504,#58505,#58506,#58507,#58508,
#58509),.UNSPECIFIED.,.F.,.F.,(4,2,4),(0.813847978400163,0.909406578867221,
1.10554196287215),.UNSPECIFIED.);
#5251=B_SPLINE_CURVE_WITH_KNOTS('',3,(#58510,#58511,#58512,#58513),
 .UNSPECIFIED.,.F.,.F.,(4,4),(0.,1.5),.UNSPECIFIED.);
#5252=B_SPLINE_CURVE_WITH_KNOTS('',3,(#58599,#58600,#58601,#58602),
 .UNSPECIFIED.,.F.,.F.,(4,4),(0.102444446511599,0.212752916841184),
 .UNSPECIFIED.);
#5253=B_SPLINE_CURVE_WITH_KNOTS('',3,(#58606,#58607,#58608,#58609),
 .UNSPECIFIED.,.F.,.F.,(4,4),(0.,1.5),.UNSPECIFIED.);
#5254=B_SPLINE_CURVE_WITH_KNOTS('',3,(#58611,#58612,#58613,#58614),
 .UNSPECIFIED.,.F.,.F.,(4,4),(0.,0.0624333513921405),.UNSPECIFIED.);
#5255=B_SPLINE_CURVE_WITH_KNOTS('',3,(#58696,#58697,#58698,#58699),
 .UNSPECIFIED.,.F.,.F.,(4,4),(0.,0.0942418390729232),.UNSPECIFIED.);
#5256=B_SPLINE_CURVE_WITH_KNOTS('',3,(#58702,#58703,#58704,#58705,#58706,
#58707),.UNSPECIFIED.,.F.,.F.,(4,2,4),(0.813847978447724,0.909406578934804,
1.10554196297989),.UNSPECIFIED.);
#5257=B_SPLINE_CURVE_WITH_KNOTS('',3,(#58708,#58709,#58710,#58711),
 .UNSPECIFIED.,.F.,.F.,(4,4),(0.,1.5),.UNSPECIFIED.);
#5258=B_SPLINE_CURVE_WITH_KNOTS('',3,(#58797,#58798,#58799,#58800),
 .UNSPECIFIED.,.F.,.F.,(4,4),(0.102444446506069,0.212752916828345),
 .UNSPECIFIED.);
#5259=B_SPLINE_CURVE_WITH_KNOTS('',3,(#58804,#58805,#58806,#58807),
 .UNSPECIFIED.,.F.,.F.,(4,4),(0.,1.5),.UNSPECIFIED.);
#5260=B_SPLINE_CURVE_WITH_KNOTS('',3,(#58809,#58810,#58811,#58812),
 .UNSPECIFIED.,.F.,.F.,(4,4),(0.,0.0624333513925485),.UNSPECIFIED.);
#5261=B_SPLINE_CURVE_WITH_KNOTS('',3,(#58894,#58895,#58896,#58897),
 .UNSPECIFIED.,.F.,.F.,(4,4),(0.,0.0942418390736248),.UNSPECIFIED.);
#5262=B_SPLINE_CURVE_WITH_KNOTS('',3,(#58900,#58901,#58902,#58903,#58904,
#58905),.UNSPECIFIED.,.F.,.F.,(4,2,4),(0.813847978393684,0.909406578861889,
1.10554196287168),.UNSPECIFIED.);
#5263=B_SPLINE_CURVE_WITH_KNOTS('',3,(#58906,#58907,#58908,#58909),
 .UNSPECIFIED.,.F.,.F.,(4,4),(0.,1.5),.UNSPECIFIED.);
#5264=B_SPLINE_CURVE_WITH_KNOTS('',3,(#58995,#58996,#58997,#58998),
 .UNSPECIFIED.,.F.,.F.,(4,4),(0.102444446506724,0.212752916833258),
 .UNSPECIFIED.);
#5265=B_SPLINE_CURVE_WITH_KNOTS('',3,(#59002,#59003,#59004,#59005),
 .UNSPECIFIED.,.F.,.F.,(4,4),(0.,1.5),.UNSPECIFIED.);
#5266=B_SPLINE_CURVE_WITH_KNOTS('',3,(#59007,#59008,#59009,#59010),
 .UNSPECIFIED.,.F.,.F.,(4,4),(0.,0.0624333513889975),.UNSPECIFIED.);
#5267=B_SPLINE_CURVE_WITH_KNOTS('',3,(#59092,#59093,#59094,#59095),
 .UNSPECIFIED.,.F.,.F.,(4,4),(0.,0.0942418390734104),.UNSPECIFIED.);
#5268=B_SPLINE_CURVE_WITH_KNOTS('',3,(#59098,#59099,#59100,#59101,#59102,
#59103),.UNSPECIFIED.,.F.,.F.,(4,2,4),(0.813847978443022,0.909406578934323,
1.10554196299104),.UNSPECIFIED.);
#5269=B_SPLINE_CURVE_WITH_KNOTS('',3,(#59104,#59105,#59106,#59107),
 .UNSPECIFIED.,.F.,.F.,(4,4),(0.,1.5),.UNSPECIFIED.);
#5270=B_SPLINE_CURVE_WITH_KNOTS('',3,(#59193,#59194,#59195,#59196,#59197,
#59198,#59199,#59200,#59201,#59202),.UNSPECIFIED.,.F.,.F.,(4,3,3,4),(0.0202435582116424,
0.0580416628844639,0.0862802856669505,0.0958397675572854),.UNSPECIFIED.);
#5271=B_SPLINE_CURVE_WITH_KNOTS('',3,(#59206,#59207,#59208,#59209),
 .UNSPECIFIED.,.F.,.F.,(4,4),(0.,1.5),.UNSPECIFIED.);
#5272=B_SPLINE_CURVE_WITH_KNOTS('',3,(#59211,#59212,#59213,#59214,#59215,
#59216,#59217,#59218,#59219,#59220),.UNSPECIFIED.,.F.,.F.,(4,3,3,4),(0.,
0.0294422535083819,0.0624658169425315,0.0742491588861056),.UNSPECIFIED.);
#5273=B_SPLINE_CURVE_WITH_KNOTS('',3,(#59302,#59303,#59304,#59305,#59306,
#59307,#59308,#59309),.UNSPECIFIED.,.F.,.F.,(4,2,2,4),(0.,0.0579167605929198,
0.0898095080041945,0.0921865044561621),.UNSPECIFIED.);
#5274=B_SPLINE_CURVE_WITH_KNOTS('',3,(#59312,#59313,#59314,#59315,#59316,
#59317),.UNSPECIFIED.,.F.,.F.,(4,2,4),(0.0188457662145042,0.0323539946370597,
0.0791558368865173),.UNSPECIFIED.);
#5275=B_SPLINE_CURVE_WITH_KNOTS('',3,(#59318,#59319,#59320,#59321),
 .UNSPECIFIED.,.F.,.F.,(4,4),(0.,1.5),.UNSPECIFIED.);
#5276=B_SPLINE_CURVE_WITH_KNOTS('',3,(#59407,#59408,#59409,#59410,#59411,
#59412,#59413,#59414,#59415,#59416),.UNSPECIFIED.,.F.,.F.,(4,3,3,4),(0.0395084943485573,
0.0733345045630657,0.101123500261748,0.116125323696474),.UNSPECIFIED.);
#5277=B_SPLINE_CURVE_WITH_KNOTS('',3,(#59420,#59421,#59422,#59423),
 .UNSPECIFIED.,.F.,.F.,(4,4),(0.,1.5),.UNSPECIFIED.);
#5278=B_SPLINE_CURVE_WITH_KNOTS('',3,(#59425,#59426,#59427,#59428,#59429,
#59430,#59431,#59432,#59433,#59434),.UNSPECIFIED.,.F.,.F.,(4,3,3,4),(0.,
0.0270437474794931,0.0553924043849417,0.0741757654504447),.UNSPECIFIED.);
#5279=B_SPLINE_CURVE_WITH_KNOTS('',3,(#59516,#59517,#59518,#59519),
 .UNSPECIFIED.,.F.,.F.,(4,4),(0.,0.0942418390732598),.UNSPECIFIED.);
#5280=B_SPLINE_CURVE_WITH_KNOTS('',3,(#59522,#59523,#59524,#59525,#59526,
#59527),.UNSPECIFIED.,.F.,.F.,(4,2,4),(0.779548576793953,0.882208032727733,
1.03977959949153),.UNSPECIFIED.);
#5281=B_SPLINE_CURVE_WITH_KNOTS('',3,(#59528,#59529,#59530,#59531),
 .UNSPECIFIED.,.F.,.F.,(4,4),(0.,1.5),.UNSPECIFIED.);
#5282=B_SPLINE_CURVE_WITH_KNOTS('',3,(#59617,#59618,#59619,#59620),
 .UNSPECIFIED.,.F.,.F.,(4,4),(0.102444446506346,0.212752916828858),
 .UNSPECIFIED.);
#5283=B_SPLINE_CURVE_WITH_KNOTS('',3,(#59624,#59625,#59626,#59627),
 .UNSPECIFIED.,.F.,.F.,(4,4),(0.,1.5),.UNSPECIFIED.);
#5284=B_SPLINE_CURVE_WITH_KNOTS('',3,(#59629,#59630,#59631,#59632),
 .UNSPECIFIED.,.F.,.F.,(4,4),(0.,0.0624333513912447),.UNSPECIFIED.);
#5285=B_SPLINE_CURVE_WITH_KNOTS('',3,(#59714,#59715,#59716,#59717),
 .UNSPECIFIED.,.F.,.F.,(4,4),(0.,0.0942418390735563),.UNSPECIFIED.);
#5286=B_SPLINE_CURVE_WITH_KNOTS('',3,(#59720,#59721,#59722,#59723,#59724,
#59725),.UNSPECIFIED.,.F.,.F.,(4,2,4),(0.813847978426091,0.909406578908649,
1.10554196294765),.UNSPECIFIED.);
#5287=B_SPLINE_CURVE_WITH_KNOTS('',3,(#59726,#59727,#59728,#59729),
 .UNSPECIFIED.,.F.,.F.,(4,4),(0.,1.5),.UNSPECIFIED.);
#5288=B_SPLINE_CURVE_WITH_KNOTS('',3,(#59815,#59816,#59817,#59818),
 .UNSPECIFIED.,.F.,.F.,(4,4),(0.10244444650535,0.212752916825456),
 .UNSPECIFIED.);
#5289=B_SPLINE_CURVE_WITH_KNOTS('',3,(#59822,#59823,#59824,#59825),
 .UNSPECIFIED.,.F.,.F.,(4,4),(0.,1.5),.UNSPECIFIED.);
#5290=B_SPLINE_CURVE_WITH_KNOTS('',3,(#59827,#59828,#59829,#59830),
 .UNSPECIFIED.,.F.,.F.,(4,4),(0.,0.0624333513928975),.UNSPECIFIED.);
#5291=B_SPLINE_CURVE_WITH_KNOTS('',3,(#59912,#59913,#59914,#59915),
 .UNSPECIFIED.,.F.,.F.,(4,4),(0.,0.0942418390733905),.UNSPECIFIED.);
#5292=B_SPLINE_CURVE_WITH_KNOTS('',3,(#59918,#59919,#59920,#59921,#59922,
#59923),.UNSPECIFIED.,.F.,.F.,(4,2,4),(0.81384797842961,0.90940657891296,
1.1055419629536),.UNSPECIFIED.);
#5293=B_SPLINE_CURVE_WITH_KNOTS('',3,(#59924,#59925,#59926,#59927),
 .UNSPECIFIED.,.F.,.F.,(4,4),(0.,1.5),.UNSPECIFIED.);
#5294=B_SPLINE_CURVE_WITH_KNOTS('',3,(#60013,#60014,#60015,#60016),
 .UNSPECIFIED.,.F.,.F.,(4,4),(0.102444446506175,0.21275291682957),
 .UNSPECIFIED.);
#5295=B_SPLINE_CURVE_WITH_KNOTS('',3,(#60020,#60021,#60022,#60023),
 .UNSPECIFIED.,.F.,.F.,(4,4),(0.,1.5),.UNSPECIFIED.);
#5296=B_SPLINE_CURVE_WITH_KNOTS('',3,(#60025,#60026,#60027,#60028),
 .UNSPECIFIED.,.F.,.F.,(4,4),(0.,0.0624333513924381),.UNSPECIFIED.);
#5297=B_SPLINE_CURVE_WITH_KNOTS('',3,(#60110,#60111,#60112,#60113),
 .UNSPECIFIED.,.F.,.F.,(4,4),(0.,0.0942418390734806),.UNSPECIFIED.);
#5298=B_SPLINE_CURVE_WITH_KNOTS('',3,(#60116,#60117,#60118,#60119,#60120,
#60121),.UNSPECIFIED.,.F.,.F.,(4,2,4),(0.813847978432191,0.909406578917468,
1.10554196296299),.UNSPECIFIED.);
#5299=B_SPLINE_CURVE_WITH_KNOTS('',3,(#60122,#60123,#60124,#60125),
 .UNSPECIFIED.,.F.,.F.,(4,4),(0.,1.5),.UNSPECIFIED.);
#5300=B_SPLINE_CURVE_WITH_KNOTS('',3,(#60211,#60212,#60213,#60214),
 .UNSPECIFIED.,.F.,.F.,(4,4),(0.10244444650664,0.212752916829421),
 .UNSPECIFIED.);
#5301=B_SPLINE_CURVE_WITH_KNOTS('',3,(#60218,#60219,#60220,#60221),
 .UNSPECIFIED.,.F.,.F.,(4,4),(0.,1.5),.UNSPECIFIED.);
#5302=B_SPLINE_CURVE_WITH_KNOTS('',3,(#60223,#60224,#60225,#60226),
 .UNSPECIFIED.,.F.,.F.,(4,4),(0.,0.0624333513894458),.UNSPECIFIED.);
#5303=B_SPLINE_CURVE_WITH_KNOTS('',3,(#60308,#60309,#60310,#60311),
 .UNSPECIFIED.,.F.,.F.,(4,4),(0.,0.0942418390733715),.UNSPECIFIED.);
#5304=B_SPLINE_CURVE_WITH_KNOTS('',3,(#60314,#60315,#60316,#60317,#60318,
#60319),.UNSPECIFIED.,.F.,.F.,(4,2,4),(0.81384797850735,0.909406579018074,
1.10554196311433),.UNSPECIFIED.);
#5305=B_SPLINE_CURVE_WITH_KNOTS('',3,(#60320,#60321,#60322,#60323),
 .UNSPECIFIED.,.F.,.F.,(4,4),(0.,1.5),.UNSPECIFIED.);
#5306=B_SPLINE_CURVE_WITH_KNOTS('',3,(#60409,#60410,#60411,#60412,#60413,
#60414,#60415,#60416,#60417,#60418),.UNSPECIFIED.,.F.,.F.,(4,3,3,4),(0.0463594297612979,
0.0792638205058534,0.106678138460634,0.123352993578161),.UNSPECIFIED.);
#5307=B_SPLINE_CURVE_WITH_KNOTS('',3,(#60422,#60423,#60424,#60425),
 .UNSPECIFIED.,.F.,.F.,(4,4),(0.,1.5),.UNSPECIFIED.);
#5308=B_SPLINE_CURVE_WITH_KNOTS('',3,(#60427,#60428,#60429,#60430,#60431,
#60432,#60433,#60434,#60435,#60436),.UNSPECIFIED.,.F.,.F.,(4,3,3,4),(0.,
0.0265473416310855,0.0541632094422211,0.0741956218732892),.UNSPECIFIED.);
#5309=B_SPLINE_CURVE_WITH_KNOTS('',3,(#60518,#60519,#60520,#60521,#60522,
#60523),.UNSPECIFIED.,.F.,.F.,(4,2,4),(0.,0.0841859688066849,0.0944738106033242),
 .UNSPECIFIED.);
#5310=B_SPLINE_CURVE_WITH_KNOTS('',3,(#60526,#60527,#60528,#60529,#60530,
#60531),.UNSPECIFIED.,.F.,.F.,(4,2,4),(0.0591715987737748,0.0874825086625098,
0.130961342687466),.UNSPECIFIED.);
#5311=B_SPLINE_CURVE_WITH_KNOTS('',3,(#60532,#60533,#60534,#60535),
 .UNSPECIFIED.,.F.,.F.,(4,4),(0.,1.5),.UNSPECIFIED.);
#5312=B_SPLINE_CURVE_WITH_KNOTS('',3,(#60621,#60622,#60623,#60624,#60625,
#60626,#60627,#60628,#60629,#60630),.UNSPECIFIED.,.F.,.F.,(4,3,3,4),(0.0186187815726518,
0.05638216058415,0.0848432631253004,0.0941455395956483),.UNSPECIFIED.);
#5313=B_SPLINE_CURVE_WITH_KNOTS('',3,(#60634,#60635,#60636,#60637),
 .UNSPECIFIED.,.F.,.F.,(4,4),(0.,1.5),.UNSPECIFIED.);
#5314=B_SPLINE_CURVE_WITH_KNOTS('',3,(#60639,#60640,#60641,#60642,#60643,
#60644,#60645,#60646,#60647,#60648),.UNSPECIFIED.,.F.,.F.,(4,3,3,4),(0.,
0.029729407461831,0.0634621728237244,0.0742674437057334),.UNSPECIFIED.);
#5315=B_SPLINE_CURVE_WITH_KNOTS('',3,(#60730,#60731,#60732,#60733),
 .UNSPECIFIED.,.F.,.F.,(4,4),(0.,0.0942418390732922),.UNSPECIFIED.);
#5316=B_SPLINE_CURVE_WITH_KNOTS('',3,(#60736,#60737,#60738,#60739,#60740,
#60741),.UNSPECIFIED.,.F.,.F.,(4,2,4),(0.78291638968198,0.879991065903176,
1.0497516190461),.UNSPECIFIED.);
#5317=B_SPLINE_CURVE_WITH_KNOTS('',3,(#60742,#60743,#60744,#60745),
 .UNSPECIFIED.,.F.,.F.,(4,4),(0.,1.5),.UNSPECIFIED.);
#5318=B_SPLINE_CURVE_WITH_KNOTS('',3,(#60831,#60832,#60833,#60834),
 .UNSPECIFIED.,.F.,.F.,(4,4),(0.102444446507287,0.212752916834514),
 .UNSPECIFIED.);
#5319=B_SPLINE_CURVE_WITH_KNOTS('',3,(#60838,#60839,#60840,#60841),
 .UNSPECIFIED.,.F.,.F.,(4,4),(0.,1.5),.UNSPECIFIED.);
#5320=B_SPLINE_CURVE_WITH_KNOTS('',3,(#60843,#60844,#60845,#60846),
 .UNSPECIFIED.,.F.,.F.,(4,4),(0.,0.0624333513900251),.UNSPECIFIED.);
#5321=B_SPLINE_CURVE_WITH_KNOTS('',3,(#60928,#60929,#60930,#60931),
 .UNSPECIFIED.,.F.,.F.,(4,4),(0.,0.0942418390732355),.UNSPECIFIED.);
#5322=B_SPLINE_CURVE_WITH_KNOTS('',3,(#60934,#60935,#60936,#60937,#60938,
#60939),.UNSPECIFIED.,.F.,.F.,(4,2,4),(0.813847978423661,0.909406578902529,
1.10554196293435),.UNSPECIFIED.);
#5323=B_SPLINE_CURVE_WITH_KNOTS('',3,(#60940,#60941,#60942,#60943),
 .UNSPECIFIED.,.F.,.F.,(4,4),(0.,1.5),.UNSPECIFIED.);
#5324=B_SPLINE_CURVE_WITH_KNOTS('',3,(#61029,#61030,#61031,#61032),
 .UNSPECIFIED.,.F.,.F.,(4,4),(0.102444446507506,0.212752916837424),
 .UNSPECIFIED.);
#5325=B_SPLINE_CURVE_WITH_KNOTS('',3,(#61036,#61037,#61038,#61039),
 .UNSPECIFIED.,.F.,.F.,(4,4),(0.,1.5),.UNSPECIFIED.);
#5326=B_SPLINE_CURVE_WITH_KNOTS('',3,(#61041,#61042,#61043,#61044),
 .UNSPECIFIED.,.F.,.F.,(4,4),(0.,0.0624333513922893),.UNSPECIFIED.);
#5327=B_SPLINE_CURVE_WITH_KNOTS('',3,(#61126,#61127,#61128,#61129),
 .UNSPECIFIED.,.F.,.F.,(4,4),(0.,0.0942418390731036),.UNSPECIFIED.);
#5328=B_SPLINE_CURVE_WITH_KNOTS('',3,(#61132,#61133,#61134,#61135,#61136,
#61137),.UNSPECIFIED.,.F.,.F.,(4,2,4),(0.813847978416476,0.909406578891062,
1.10554196291473),.UNSPECIFIED.);
#5329=B_SPLINE_CURVE_WITH_KNOTS('',3,(#61138,#61139,#61140,#61141),
 .UNSPECIFIED.,.F.,.F.,(4,4),(0.,1.5),.UNSPECIFIED.);
#5330=B_SPLINE_CURVE_WITH_KNOTS('',3,(#61227,#61228,#61229,#61230),
 .UNSPECIFIED.,.F.,.F.,(4,4),(0.102444446497694,0.212752916802265),
 .UNSPECIFIED.);
#5331=B_SPLINE_CURVE_WITH_KNOTS('',3,(#61234,#61235,#61236,#61237),
 .UNSPECIFIED.,.F.,.F.,(4,4),(0.,1.5),.UNSPECIFIED.);
#5332=B_SPLINE_CURVE_WITH_KNOTS('',3,(#61239,#61240,#61241,#61242),
 .UNSPECIFIED.,.F.,.F.,(4,4),(0.,0.0624333513878915),.UNSPECIFIED.);
#5333=B_SPLINE_CURVE_WITH_KNOTS('',3,(#61324,#61325,#61326,#61327),
 .UNSPECIFIED.,.F.,.F.,(4,4),(0.,0.0942418390734442),.UNSPECIFIED.);
#5334=B_SPLINE_CURVE_WITH_KNOTS('',3,(#61330,#61331,#61332,#61333,#61334,
#61335),.UNSPECIFIED.,.F.,.F.,(4,2,4),(0.813847978408599,0.909406578879065,
1.10554196289057),.UNSPECIFIED.);
#5335=B_SPLINE_CURVE_WITH_KNOTS('',3,(#61336,#61337,#61338,#61339),
 .UNSPECIFIED.,.F.,.F.,(4,4),(0.,1.5),.UNSPECIFIED.);
#5336=B_SPLINE_CURVE_WITH_KNOTS('',3,(#61425,#61426,#61427,#61428),
 .UNSPECIFIED.,.F.,.F.,(4,4),(0.102444446506644,0.212752916832659),
 .UNSPECIFIED.);
#5337=B_SPLINE_CURVE_WITH_KNOTS('',3,(#61432,#61433,#61434,#61435),
 .UNSPECIFIED.,.F.,.F.,(4,4),(0.,1.5),.UNSPECIFIED.);
#5338=B_SPLINE_CURVE_WITH_KNOTS('',3,(#61437,#61438,#61439,#61440),
 .UNSPECIFIED.,.F.,.F.,(4,4),(0.,0.0624333513938403),.UNSPECIFIED.);
#5339=B_SPLINE_CURVE_WITH_KNOTS('',3,(#61522,#61523,#61524,#61525),
 .UNSPECIFIED.,.F.,.F.,(4,4),(0.,0.0942418390734082),.UNSPECIFIED.);
#5340=B_SPLINE_CURVE_WITH_KNOTS('',3,(#61528,#61529,#61530,#61531,#61532,
#61533),.UNSPECIFIED.,.F.,.F.,(4,2,4),(0.813847978438528,0.909406578924881,
1.10554196297139),.UNSPECIFIED.);
#5341=B_SPLINE_CURVE_WITH_KNOTS('',3,(#61534,#61535,#61536,#61537),
 .UNSPECIFIED.,.F.,.F.,(4,4),(0.,1.5),.UNSPECIFIED.);
#5342=B_SPLINE_CURVE_WITH_KNOTS('',3,(#61623,#61624,#61625,#61626),
 .UNSPECIFIED.,.F.,.F.,(4,4),(0.0904405428983144,0.199382706551901),
 .UNSPECIFIED.);
#5343=B_SPLINE_CURVE_WITH_KNOTS('',3,(#61630,#61631,#61632,#61633),
 .UNSPECIFIED.,.F.,.F.,(4,4),(0.,1.5),.UNSPECIFIED.);
#5344=B_SPLINE_CURVE_WITH_KNOTS('',3,(#61635,#61636,#61637,#61638),
 .UNSPECIFIED.,.F.,.F.,(4,4),(0.,0.0619557939569426),.UNSPECIFIED.);
#5345=B_SPLINE_CURVE_WITH_KNOTS('',3,(#61720,#61721,#61722,#61723),
 .UNSPECIFIED.,.F.,.F.,(4,4),(0.,0.0942418390734305),.UNSPECIFIED.);
#5346=B_SPLINE_CURVE_WITH_KNOTS('',3,(#61726,#61727,#61728,#61729,#61730,
#61731),.UNSPECIFIED.,.F.,.F.,(4,2,4),(0.604749643384554,0.619109901140346,
0.773617109883765),.UNSPECIFIED.);
#5347=B_SPLINE_CURVE_WITH_KNOTS('',3,(#61732,#61733,#61734,#61735),
 .UNSPECIFIED.,.F.,.F.,(4,4),(0.,1.5),.UNSPECIFIED.);
#5348=B_SPLINE_CURVE_WITH_KNOTS('',3,(#62004,#62005,#62006,#62007,#62008,
#62009,#62010,#62011,#62012,#62013,#62014,#62015,#62016,#62017,#62018),
 .UNSPECIFIED.,.F.,.F.,(4,3,2,2,2,2,4),(-0.00329079135824289,0.,0.0066432817682188,
0.0172206827634487,0.0289541451570132,0.039919328261124,0.0424908650280393),
 .UNSPECIFIED.);
#5349=B_SPLINE_CURVE_WITH_KNOTS('',3,(#62105,#62106,#62107,#62108,#62109,
#62110,#62111,#62112,#62113,#62114,#62115,#62116,#62117,#62118,#62119),
 .UNSPECIFIED.,.F.,.F.,(4,3,2,2,2,2,4),(-0.00329079135824245,0.,0.00664328176821677,
0.0172206827634322,0.0289541451569808,0.0399193282610819,0.0424908650279941),
 .UNSPECIFIED.);
#5350=B_SPLINE_CURVE_WITH_KNOTS('',3,(#62240,#62241,#62242,#62243,#62244,
#62245,#62246,#62247,#62248,#62249,#62250,#62251,#62252,#62253,#62254),
 .UNSPECIFIED.,.F.,.F.,(4,3,2,2,2,2,4),(-0.00329079135824467,0.,0.00664328176822443,
0.0172206827634871,0.0289541451570832,0.0399193282612205,0.0424908650281417),
 .UNSPECIFIED.);
#5351=B_SPLINE_CURVE_WITH_KNOTS('',3,(#62280,#62281,#62282,#62283,#62284,
#62285,#62286,#62287,#62288,#62289,#62290,#62291,#62292,#62293,#62294),
 .UNSPECIFIED.,.F.,.F.,(4,2,2,2,3,2,4),(-0.042480297745229,-0.0324603624462188,
-0.0213862802599032,-0.0097989641520867,0.,0.00323812560369846,0.00328789213043021),
 .UNSPECIFIED.);
#5352=B_SPLINE_CURVE_WITH_KNOTS('',3,(#62323,#62324,#62325,#62326,#62327,
#62328),.UNSPECIFIED.,.F.,.F.,(4,2,4),(0.0321300733325589,0.0445286131406419,
0.0595369958610961),.UNSPECIFIED.);
#5353=B_SPLINE_CURVE_WITH_KNOTS('',3,(#62339,#62340,#62341,#62342,#62343,
#62344,#62345,#62346,#62347,#62348,#62349,#62350,#62351,#62352,#62353,#62354,
#62355,#62356,#62357,#62358,#62359),.UNSPECIFIED.,.F.,.F.,(4,2,2,2,3,2,
2,2,2,4),(0.173757899546907,0.173876480819041,0.174078751267789,0.174509383268949,
0.177045668856987,0.182861205270908,0.190817433861452,0.200151573933346,
0.210419579997881,0.219485681147617),.UNSPECIFIED.);
#5354=B_SPLINE_CURVE_WITH_KNOTS('',3,(#62363,#62364,#62365,#62366,#62367,
#62368,#62369,#62370,#62371,#62372,#62373,#62374,#62375,#62376,#62377,#62378,
#62379,#62380,#62381,#62382,#62383),.UNSPECIFIED.,.F.,.F.,(4,2,2,2,2,3,
2,2,2,4),(0.134450369378915,0.14123202266608,0.152737468233511,0.161147712982236,
0.166702035392685,0.176890070113637,0.179458084695312,0.179868341709683,
0.180066634123894,0.180178050765678),.UNSPECIFIED.);
#5355=B_SPLINE_CURVE_WITH_KNOTS('',3,(#62386,#62387,#62388,#62389,#62390,
#62391),.UNSPECIFIED.,.F.,.F.,(4,2,4),(0.0321300733325583,0.0445286131406419,
0.0595369958610961),.UNSPECIFIED.);
#5356=B_SPLINE_CURVE_WITH_KNOTS('',3,(#63448,#63449,#63450,#63451,#63452,
#63453,#63454,#63455,#63456,#63457,#63458,#63459,#63460,#63461,#63462,#63463,
#63464,#63465,#63466,#63467,#63468,#63469,#63470,#63471,#63472,#63473,#63474,
#63475,#63476,#63477,#63478,#63479,#63480,#63481,#63482,#63483,#63484,#63485,
#63486,#63487,#63488,#63489,#63490,#63491,#63492,#63493,#63494,#63495,#63496,
#63497,#63498,#63499,#63500,#63501,#63502,#63503,#63504,#63505,#63506,#63507,
#63508,#63509,#63510,#63511,#63512,#63513,#63514,#63515,#63516,#63517,#63518,
#63519,#63520,#63521,#63522,#63523),.UNSPECIFIED.,.F.,.F.,(4,1,1,1,1,1,
1,1,1,1,1,1,1,1,1,1,1,1,1,1,1,1,1,1,1,1,1,1,1,1,1,1,1,1,1,1,1,1,1,1,1,1,
1,1,1,1,1,1,1,1,1,1,1,1,1,1,1,1,1,1,1,1,1,1,1,1,1,1,1,1,1,1,1,4),(0.,0.00892857142857143,
0.0178571428571429,0.0357142857142857,0.0535714285714286,0.0714285714285714,
0.0892857142857143,0.107142857142857,0.125,0.142857142857143,0.158730158730159,
0.174603174603175,0.182539682539683,0.186507936507937,0.19047619047619,
0.202380952380952,0.214285714285714,0.226190476190476,0.238095238095238,
0.25,0.261904761904762,0.273809523809524,0.279761904761905,0.285714285714286,
0.297619047619048,0.30952380952381,0.321428571428571,0.333333333333333,
0.349206349206349,0.365079365079365,0.380952380952381,0.396825396825397,
0.412698412698413,0.428571428571429,0.436507936507937,0.452380952380952,
0.464285714285714,0.476190476190476,0.488095238095238,0.5,0.517857142857143,
0.535714285714286,0.553571428571429,0.571428571428571,0.589285714285714,
0.607142857142857,0.625,0.642857142857143,0.651785714285714,0.660714285714286,
0.678571428571428,0.696428571428571,0.714285714285714,0.726190476190476,
0.738095238095238,0.75,0.761904761904762,0.773809523809524,0.785714285714286,
0.797619047619047,0.809523809523809,0.821428571428571,0.833333333333333,
0.845238095238095,0.857142857142857,0.875,0.892857142857143,0.910714285714286,
0.928571428571429,0.946428571428571,0.964285714285714,0.982142857142857,
0.991071428571429,1.),.UNSPECIFIED.);
#5357=B_SPLINE_CURVE_WITH_KNOTS('',3,(#63737,#63738,#63739,#63740),
 .UNSPECIFIED.,.F.,.F.,(4,4),(0.143091562311917,0.172672323717935),
 .UNSPECIFIED.);
#5358=B_SPLINE_CURVE_WITH_KNOTS('',3,(#63743,#63744,#63745,#63746),
 .UNSPECIFIED.,.F.,.F.,(4,4),(-0.172672323717935,-0.143091563390451),
 .UNSPECIFIED.);
#5359=B_SPLINE_CURVE_WITH_KNOTS('',3,(#63749,#63750,#63751,#63752),
 .UNSPECIFIED.,.F.,.F.,(4,4),(-0.173632784471181,-0.144052021996696),
 .UNSPECIFIED.);
#5360=B_SPLINE_CURVE_WITH_KNOTS('',3,(#63779,#63780,#63781,#63782),
 .UNSPECIFIED.,.F.,.F.,(4,4),(0.144052023091887,0.173632784471181),
 .UNSPECIFIED.);
#5361=B_SPLINE_CURVE_WITH_KNOTS('',3,(#63788,#63789,#63790,#63791),
 .UNSPECIFIED.,.F.,.F.,(4,4),(-0.224098351300682,-0.214549181227953),
 .UNSPECIFIED.);
#5362=B_SPLINE_CURVE_WITH_KNOTS('',3,(#63798,#63799,#63800,#63801,#63802,
#63803,#63804,#63805,#63806,#63807,#63808,#63809,#63810,#63811),
 .UNSPECIFIED.,.F.,.F.,(4,2,2,2,2,2,4),(-0.224745183165744,-0.224338209360955,
-0.195801564669302,-0.167421789000985,-0.142834461201585,-0.123828977041314,
-0.107197280907097),.UNSPECIFIED.);
#5363=B_SPLINE_CURVE_WITH_KNOTS('',3,(#63866,#63867,#63868,#63869,#63870,
#63871,#63872,#63873,#63874,#63875,#63876,#63877,#63878,#63879),
 .UNSPECIFIED.,.F.,.F.,(4,2,2,2,2,2,4),(-0.0960754972725223,-0.0824346759427748,
-0.066846944434569,-0.0466811511835726,-0.0234049052400428,0.,0.000333787781842202),
 .UNSPECIFIED.);
#5364=B_SPLINE_CURVE_WITH_KNOTS('',3,(#63915,#63916,#63917,#63918),
 .UNSPECIFIED.,.F.,.F.,(4,4),(0.357860307352845,0.38744106972591),
 .UNSPECIFIED.);
#5365=B_SPLINE_CURVE_WITH_KNOTS('',3,(#63919,#63920,#63921,#63922),
 .UNSPECIFIED.,.F.,.F.,(4,4),(-0.38744106972591,-0.357860307352845),
 .UNSPECIFIED.);
#5366=B_SPLINE_CURVE_WITH_KNOTS('',3,(#63930,#63931,#63932,#63933),
 .UNSPECIFIED.,.F.,.F.,(4,4),(-0.0295807575131674,-2.15031488595949E-16),
 .UNSPECIFIED.);
#5367=B_SPLINE_CURVE_WITH_KNOTS('',3,(#63940,#63941,#63942,#63943,#63944,
#63945,#63946,#63947,#63948,#63949,#63950,#63951,#63952,#63953),
 .UNSPECIFIED.,.F.,.F.,(4,2,2,2,2,2,4),(0.0949936904735385,0.109164132542672,
0.125358949984382,0.146855590277485,0.168423573252805,0.190934620475292,
0.191367837777155),.UNSPECIFIED.);
#5368=B_SPLINE_CURVE_WITH_KNOTS('',3,(#64015,#64016,#64017,#64018),
 .UNSPECIFIED.,.F.,.F.,(4,4),(-0.0295807623344723,-2.06363027950495E-16),
 .UNSPECIFIED.);
#5369=B_SPLINE_CURVE_WITH_KNOTS('',3,(#64019,#64020,#64021,#64022),
 .UNSPECIFIED.,.F.,.F.,(4,4),(2.06363027950495E-16,0.0295807623344723),
 .UNSPECIFIED.);
#5370=B_SPLINE_CURVE_WITH_KNOTS('',3,(#64047,#64048,#64049,#64050),
 .UNSPECIFIED.,.F.,.F.,(4,4),(-0.0295807623160019,-6.08201692644882E-19),
 .UNSPECIFIED.);
#5371=B_SPLINE_CURVE_WITH_KNOTS('',3,(#64051,#64052,#64053,#64054),
 .UNSPECIFIED.,.F.,.F.,(4,4),(6.08201692644882E-19,0.0295807623160019),
 .UNSPECIFIED.);
#5372=B_SPLINE_CURVE_WITH_KNOTS('',3,(#64057,#64058,#64059,#64060,#64061,
#64062,#64063,#64064,#64065,#64066,#64067,#64068,#64069,#64070),
 .UNSPECIFIED.,.F.,.F.,(4,2,2,2,2,2,4),(-0.00043336587833757,0.,0.0225187676075078,
0.044094147534689,0.0655981603120321,0.0817985319256877,0.0959738338873166),
 .UNSPECIFIED.);
#5373=B_SPLINE_CURVE_WITH_KNOTS('',3,(#64081,#64082,#64083,#64084),
 .UNSPECIFIED.,.F.,.F.,(4,4),(0.21454918194711,0.224098351300682),
 .UNSPECIFIED.);
#5374=B_SPLINE_CURVE_WITH_KNOTS('',3,(#64092,#64093,#64094,#64095,#64096,
#64097,#64098,#64099,#64100,#64101,#64102,#64103,#64104,#64105),
 .UNSPECIFIED.,.F.,.F.,(4,2,2,2,2,2,4),(-0.000433365878018287,0.,0.0225187676075679,
0.04409414753479,0.0655981603121373,0.081798531925792,0.0959738338874173),
 .UNSPECIFIED.);
#5375=B_SPLINE_CURVE_WITH_KNOTS('',3,(#64122,#64123,#64124,#64125,#64126,
#64127,#64128,#64129,#64130,#64131,#64132,#64133),.UNSPECIFIED.,.F.,.F.,
(4,2,2,2,2,4),(0.,0.0151014582898052,0.0345370073824244,0.058455076138778,
0.0839695268602519,0.0844093817034405),.UNSPECIFIED.);
#5376=B_SPLINE_CURVE_WITH_KNOTS('',3,(#64140,#64141,#64142,#64143),
 .UNSPECIFIED.,.F.,.F.,(4,4),(-0.084228764664281,-0.0746795945915525),
 .UNSPECIFIED.);
#5377=B_SPLINE_CURVE_WITH_KNOTS('',3,(#64146,#64147,#64148,#64149,#64150,
#64151,#64152,#64153,#64154,#64155,#64156,#64157,#64158,#64159,#64160,#64161),
 .UNSPECIFIED.,.F.,.F.,(4,2,2,2,2,2,2,4),(-0.000449799814571451,0.,0.0220871623056755,
0.0431506585070033,0.0650141873659196,0.0813775476367432,0.0955802995948401,
0.0959539671675678),.UNSPECIFIED.);
#5378=B_SPLINE_CURVE_WITH_KNOTS('',3,(#64193,#64194,#64195,#64196),
 .UNSPECIFIED.,.F.,.F.,(4,4),(2.15031488595949E-16,0.0295807575131674),
 .UNSPECIFIED.);
#5379=B_SPLINE_CURVE_WITH_KNOTS('',3,(#64203,#64204,#64205,#64206,#64207,
#64208,#64209,#64210,#64211,#64212,#64213,#64214,#64215,#64216),
 .UNSPECIFIED.,.F.,.F.,(4,2,2,2,2,2,4),(0.,0.014053468854056,0.0301647070840401,
0.0516306547628395,0.0728079263494303,0.0950476067985505,0.0954931369347626),
 .UNSPECIFIED.);
#5380=B_SPLINE_CURVE_WITH_KNOTS('',3,(#64226,#64227,#64228,#64229),
 .UNSPECIFIED.,.F.,.F.,(4,4),(-0.224098351300682,-0.214549181227954),
 .UNSPECIFIED.);
#5381=B_SPLINE_CURVE_WITH_KNOTS('',3,(#64249,#64250,#64251,#64252,#64253,
#64254,#64255,#64256,#64257,#64258,#64259,#64260,#64261,#64262),
 .UNSPECIFIED.,.F.,.F.,(4,2,2,2,2,2,4),(0.0949936904735942,0.109164132542739,
0.125358949984464,0.146855590277593,0.168423573252929,0.190934620475441,
0.191367837777403),.UNSPECIFIED.);
#5382=B_SPLINE_CURVE_WITH_KNOTS('',3,(#64275,#64276,#64277,#64278,#64279,
#64280,#64281,#64282,#64283,#64284,#64285,#64286),.UNSPECIFIED.,.F.,.F.,
(4,2,2,2,2,4),(-0.000399537795305727,0.,0.0380148222930731,0.0673927529984265,
0.0894121467178007,0.0947714478271359),.UNSPECIFIED.);
#5383=B_SPLINE_CURVE_WITH_KNOTS('',3,(#64290,#64291,#64292,#64293,#64294,
#64295,#64296,#64297,#64298,#64299,#64300,#64301),.UNSPECIFIED.,.F.,.F.,
(4,2,2,2,2,4),(0.106231153334496,0.110609380645274,0.128597903585479,0.152597909542381,
0.183653737492122,0.183980135888318),.UNSPECIFIED.);
#5384=B_SPLINE_CURVE_WITH_KNOTS('',3,(#64302,#64303,#64304,#64305),
 .UNSPECIFIED.,.F.,.F.,(4,4),(0.0746795945915525,0.0842287639451254),
 .UNSPECIFIED.);
#5385=B_SPLINE_CURVE_WITH_KNOTS('',3,(#64306,#64307,#64308,#64309),
 .UNSPECIFIED.,.F.,.F.,(4,4),(0.21454918194711,0.224098351300682),
 .UNSPECIFIED.);
#5386=B_SPLINE_CURVE_WITH_KNOTS('',3,(#64318,#64319,#64320,#64321,#64322,
#64323,#64324,#64325,#64326,#64327,#64328,#64329),.UNSPECIFIED.,.F.,.F.,
(4,2,2,2,2,4),(0.,0.0151014582898128,0.0345370073824547,0.0584550761388158,
0.0839695268603532,0.0844093817034856),.UNSPECIFIED.);
#5387=B_SPLINE_CURVE_WITH_KNOTS('',3,(#64333,#64334,#64335,#64336,#64337,
#64338,#64339,#64340,#64341,#64342,#64343,#64344),.UNSPECIFIED.,.F.,.F.,
(4,2,2,2,2,4),(-0.000399537795187636,0.,0.0380148222927662,0.0673927529975771,
0.0894121467165036,0.0947714478257393),.UNSPECIFIED.);
#5388=B_SPLINE_CURVE_WITH_KNOTS('',3,(#64346,#64347,#64348,#64349),
 .UNSPECIFIED.,.F.,.F.,(4,4),(-0.084228764664281,-0.0746795945915525),
 .UNSPECIFIED.);
#5389=B_SPLINE_CURVE_WITH_KNOTS('',3,(#64355,#64356,#64357,#64358,#64359,
#64360,#64361,#64362,#64363,#64364,#64365,#64366),.UNSPECIFIED.,.F.,.F.,
(4,2,2,2,2,4),(-0.000444101878230381,0.,0.0380815409708187,0.0676748364114729,
0.0897163855403829,0.0947742742230686),.UNSPECIFIED.);
#5390=B_SPLINE_CURVE_WITH_KNOTS('',3,(#64410,#64411,#64412,#64413,#64414,
#64415,#64416,#64417,#64418,#64419,#64420,#64421),.UNSPECIFIED.,.F.,.F.,
(4,2,2,2,2,4),(-0.000444101878323987,0.,0.0380815409760417,0.0676748364256351,
0.0897163855612856,0.0981715128747534),.UNSPECIFIED.);
#5391=B_SPLINE_CURVE_WITH_KNOTS('',3,(#64424,#64425,#64426,#64427,#64428,
#64429,#64430,#64431,#64432,#64433,#64434,#64435),.UNSPECIFIED.,.F.,.F.,
(4,2,2,2,2,4),(0.103458653410514,0.110599336947648,0.128587640292216,0.152592542525185,
0.183648506748048,0.18397598979878),.UNSPECIFIED.);
#5392=B_SPLINE_CURVE_WITH_KNOTS('',3,(#64437,#64438,#64439,#64440),
 .UNSPECIFIED.,.F.,.F.,(4,4),(0.0743659931772117,0.08135049123277),
 .UNSPECIFIED.);
#5393=B_SPLINE_CURVE_WITH_KNOTS('',3,(#64443,#64444,#64445,#64446),
 .UNSPECIFIED.,.F.,.F.,(4,4),(-0.223127503799962,-0.216143005636944),
 .UNSPECIFIED.);
#5394=B_SPLINE_CURVE_WITH_KNOTS('',3,(#64456,#64457,#64458,#64459,#64460,
#64461,#64462,#64463,#64464,#64465,#64466,#64467),.UNSPECIFIED.,.F.,.F.,
(4,2,2,2,2,4),(-0.000444101878259206,0.,0.0380815409762479,0.0676748364260828,
0.089716385561879,0.0981715128754566),.UNSPECIFIED.);
#5395=B_SPLINE_CURVE_WITH_KNOTS('',3,(#64470,#64471,#64472,#64473,#64474,
#64475,#64476,#64477,#64478,#64479,#64480,#64481),.UNSPECIFIED.,.F.,.F.,
(4,2,2,2,2,4),(0.103458653410644,0.110599336947805,0.128587640292406,0.15259254252545,
0.183648506748331,0.18397598979916),.UNSPECIFIED.);
#5396=B_SPLINE_CURVE_WITH_KNOTS('',3,(#64483,#64484,#64485,#64486),
 .UNSPECIFIED.,.F.,.F.,(4,4),(0.0743659931772121,0.0813504912327701),
 .UNSPECIFIED.);
#5397=B_SPLINE_CURVE_WITH_KNOTS('',3,(#64489,#64490,#64491,#64492),
 .UNSPECIFIED.,.F.,.F.,(4,4),(-0.223127503799961,-0.216143005636943),
 .UNSPECIFIED.);
#5398=B_SPLINE_CURVE_WITH_KNOTS('',3,(#64500,#64501,#64502,#64503,#64504,
#64505,#64506,#64507,#64508,#64509,#64510,#64511),.UNSPECIFIED.,.F.,.F.,
(4,2,2,2,2,4),(-0.00044410187825338,0.,0.0380815409761677,0.0676748364257858,
0.0897163855613554,0.0947742742458168),.UNSPECIFIED.);
#5399=B_SPLINE_CURVE_WITH_KNOTS('',3,(#64518,#64519,#64520,#64521),
 .UNSPECIFIED.,.F.,.F.,(4,4),(0.0746795945915525,0.0842287646642811),
 .UNSPECIFIED.);
#5400=B_SPLINE_CURVE_WITH_KNOTS('',3,(#64522,#64523,#64524,#64525,#64526,
#64527,#64528,#64529,#64530,#64531,#64532,#64533),.UNSPECIFIED.,.F.,.F.,
(4,2,2,2,2,4),(0.,0.0151014582898057,0.0345370073824282,0.0584550761387909,
0.0839695268602773,0.084409381703446),.UNSPECIFIED.);
#5401=B_SPLINE_CURVE_WITH_KNOTS('',3,(#64541,#64542,#64543,#64544,#64545,
#64546,#64547,#64548,#64549,#64550,#64551,#64552),.UNSPECIFIED.,.F.,.F.,
(4,2,2,2,2,4),(0.,0.0151014582898054,0.0345370073824249,0.0584550761387796,
0.0839695268602591,0.0844093817034706),.UNSPECIFIED.);
#5402=B_SPLINE_CURVE_WITH_KNOTS('',3,(#64554,#64555,#64556,#64557),
 .UNSPECIFIED.,.F.,.F.,(4,4),(-0.0842287646642811,-0.0746795945915525),
 .UNSPECIFIED.);
#5403=B_SPLINE_CURVE_WITH_KNOTS('',3,(#64571,#64572,#64573,#64574,#64575,
#64576,#64577,#64578,#64579,#64580,#64581,#64582,#64583,#64584,#64585,#64586,
#64587,#64588,#64589,#64590,#64591),.UNSPECIFIED.,.F.,.F.,(4,2,2,2,2,3,
2,2,2,4),(0.158319501107787,0.167251782267889,0.176184063427991,0.187124730842742,
0.199384896436401,0.211645062030061,0.22379953303083,0.2359540040316,0.246692006811033,
0.264142032122818),.UNSPECIFIED.);
#5404=B_SPLINE_CURVE_WITH_KNOTS('',3,(#64625,#64626,#64627,#64628,#64629,
#64630,#64631,#64632,#64633,#64634,#64635,#64636),.UNSPECIFIED.,.F.,.F.,
(4,2,2,2,2,4),(0.181384150825648,0.206078531962836,0.231632932915096,0.252637853635304,
0.263140313995408,0.273642774355512),.UNSPECIFIED.);
#5405=B_SPLINE_CURVE_WITH_KNOTS('',3,(#64641,#64642,#64643,#64644,#64645,
#64646,#64647,#64648,#64649,#64650,#64651,#64652),.UNSPECIFIED.,.F.,.F.,
(4,2,2,2,2,4),(-0.0876802602836453,-0.0733239775103818,-0.0560578353470276,
-0.0325387048074095,0.,0.000330498359414059),.UNSPECIFIED.);
#5406=B_SPLINE_CURVE_WITH_KNOTS('',3,(#64656,#64657,#64658,#64659),
 .UNSPECIFIED.,.F.,.F.,(4,4),(0.216143005618354,0.223127503799962),
 .UNSPECIFIED.);
#5407=B_SPLINE_CURVE_WITH_KNOTS('',3,(#64665,#64666,#64667,#64668,#64669,
#64670,#64671,#64672,#64673,#64674,#64675,#64676,#64677,#64678,#64679,#64680,
#64681,#64682,#64683,#64684,#64685,#64686,#64687,#64688,#64689,#64690,#64691,
#64692,#64693,#64694,#64695,#64696,#64697,#64698,#64699,#64700,#64701,#64702,
#64703,#64704,#64705,#64706,#64707,#64708,#64709,#64710,#64711,#64712,#64713,
#64714,#64715,#64716,#64717,#64718,#64719,#64720,#64721,#64722,#64723,#64724,
#64725),.UNSPECIFIED.,.F.,.F.,(4,3,3,3,3,3,3,3,3,3,3,3,3,3,3,3,3,3,3,3,
4),(0.,0.00788945390620161,0.0159107528337136,0.0198233466742012,0.0278090397100955,
0.0338830033914972,0.0395609471880743,0.0474955046467764,0.0554321605872608,
0.0591436409533912,0.0671079528129928,0.0676235550484229,0.075592682599463,
0.0785910514609892,0.0865300392579837,0.0944439925209208,0.0979951919099392,
0.101302747945548,0.108060095589035,0.116004888439858,0.118137330218053),
 .UNSPECIFIED.);
#5408=B_SPLINE_CURVE_WITH_KNOTS('',3,(#64731,#64732,#64733,#64734,#64735,
#64736),.UNSPECIFIED.,.F.,.F.,(4,2,4),(0.0370807285215095,0.0556314474159261,
0.0743351338524323),.UNSPECIFIED.);
#5409=B_SPLINE_CURVE_WITH_KNOTS('',3,(#64740,#64741,#64742,#64743,#64744,
#64745,#64746,#64747,#64748,#64749),.UNSPECIFIED.,.F.,.F.,(4,2,2,2,4),(0.148746748488587,
0.167205194290617,0.185750729133706,0.204398921478351,0.223127503799962),
 .UNSPECIFIED.);
#5410=B_SPLINE_CURVE_WITH_KNOTS('',3,(#64754,#64755,#64756,#64757),
 .UNSPECIFIED.,.F.,.F.,(4,4),(0.0743659931772123,0.0813504912327697),
 .UNSPECIFIED.);
#5411=B_SPLINE_CURVE_WITH_KNOTS('',3,(#64759,#64760,#64761,#64762,#64763,
#64764,#64765,#64766,#64767,#64768,#64769,#64770),.UNSPECIFIED.,.F.,.F.,
(4,2,2,2,2,4),(0.103458653410611,0.110599336946118,0.128587640290153,0.152592542522104,
0.183648506743288,0.183975989794056),.UNSPECIFIED.);
#5412=B_SPLINE_CURVE_WITH_KNOTS('',3,(#64797,#64798,#64799,#64800),
 .UNSPECIFIED.,.F.,.F.,(4,4),(-1.32591570645538,-0.833509855154531),
 .UNSPECIFIED.);
#5413=B_SPLINE_CURVE_WITH_KNOTS('',3,(#64807,#64808,#64809,#64810),
 .UNSPECIFIED.,.F.,.F.,(4,4),(-1.32593023123408,-0.833524379933391),
 .UNSPECIFIED.);
#5414=B_SPLINE_CURVE_WITH_KNOTS('',3,(#64821,#64822,#64823,#64824),
 .UNSPECIFIED.,.F.,.F.,(4,4),(-1.32591570645538,-0.833509855154526),
 .UNSPECIFIED.);
#5415=B_SPLINE_CURVE_WITH_KNOTS('',3,(#64831,#64832,#64833,#64834,#64835,
#64836,#64837,#64838,#64839,#64840),.UNSPECIFIED.,.F.,.F.,(4,2,2,2,4),(0.0743659931772121,
0.0930945754988228,0.111742767843467,0.130288302686557,0.148746748488587),
 .UNSPECIFIED.);
#5416=B_SPLINE_CURVE_WITH_KNOTS('',3,(#64843,#64844,#64845,#64846,#64847,
#64848),.UNSPECIFIED.,.F.,.F.,(4,2,4),(0.223030667259691,0.241734353696197,
0.260285072590614),.UNSPECIFIED.);
#5417=B_SPLINE_CURVE_WITH_KNOTS('',3,(#64850,#64851,#64852,#64853,#64854,
#64855,#64856,#64857,#64858,#64859,#64860,#64861,#64862,#64863,#64864,#64865,
#64866,#64867,#64868,#64869,#64870,#64871,#64872,#64873,#64874,#64875,#64876,
#64877,#64878,#64879,#64880,#64881,#64882,#64883,#64884,#64885,#64886,#64887,
#64888,#64889,#64890,#64891,#64892,#64893,#64894,#64895,#64896,#64897,#64898,
#64899,#64900,#64901,#64902,#64903,#64904,#64905,#64906,#64907,#64908,#64909,
#64910),.UNSPECIFIED.,.F.,.F.,(4,3,3,3,3,3,3,3,3,3,3,3,3,3,3,3,3,3,3,3,
4),(0.,0.00795992543948654,0.0158204416141764,0.0168758198258157,0.0195772972159437,
0.0274588993006712,0.0354166538447632,0.0390209976709924,0.0469884348389282,
0.0505535087526213,0.0584240670042275,0.0663285883843903,0.0742861746185043,
0.0778995393740957,0.0842874233172874,0.0922711899963328,0.0975220154528215,
0.105525144757543,0.10781729367049,0.115774466403908,0.11811865411736),
 .UNSPECIFIED.);
#5418=B_SPLINE_CURVE_WITH_KNOTS('',3,(#64918,#64919,#64920,#64921,#64922,
#64923,#64924,#64925,#64926,#64927),.UNSPECIFIED.,.F.,.F.,(4,2,2,2,4),(0.0743659931772119,
0.0930945754988228,0.111742767843467,0.130288302686557,0.148746748488587),
 .UNSPECIFIED.);
#5419=B_SPLINE_CURVE_WITH_KNOTS('',3,(#64930,#64931,#64932,#64933,#64934,
#64935),.UNSPECIFIED.,.F.,.F.,(4,2,4),(0.223030667259691,0.241734353696197,
0.260285072590614),.UNSPECIFIED.);
#5420=B_SPLINE_CURVE_WITH_KNOTS('',3,(#64937,#64938,#64939,#64940,#64941,
#64942,#64943,#64944,#64945,#64946,#64947,#64948,#64949,#64950,#64951,#64952,
#64953,#64954,#64955,#64956,#64957,#64958,#64959,#64960,#64961,#64962,#64963,
#64964,#64965,#64966,#64967,#64968,#64969,#64970,#64971,#64972,#64973,#64974,
#64975,#64976,#64977,#64978,#64979,#64980,#64981,#64982,#64983,#64984,#64985,
#64986,#64987,#64988,#64989,#64990,#64991,#64992,#64993,#64994,#64995,#64996,
#64997),.UNSPECIFIED.,.F.,.F.,(4,3,3,3,3,3,3,3,3,3,3,3,3,3,3,3,3,3,3,3,
4),(0.,0.00795992543949775,0.0158204416141938,0.0168758198258168,0.0195772972159446,
0.0274588993006973,0.0354166538448255,0.039020997670994,0.0469884348389804,
0.0505535087526245,0.0584240670042325,0.0663285883843688,0.0742861746184431,
0.0778995393741076,0.0842874233172998,0.0922711899963224,0.097522015452835,
0.105525144757354,0.107817293670499,0.115774466404384,0.118118654117365),
 .UNSPECIFIED.);
#5421=B_SPLINE_CURVE_WITH_KNOTS('',3,(#65005,#65006,#65007,#65008,#65009,
#65010,#65011,#65012,#65013,#65014),.UNSPECIFIED.,.F.,.F.,(4,2,2,2,4),(0.0743659931772118,
0.0930945754988225,0.111742767843467,0.130288302686557,0.148746748488587),
 .UNSPECIFIED.);
#5422=B_SPLINE_CURVE_WITH_KNOTS('',3,(#65017,#65018,#65019,#65020,#65021,
#65022),.UNSPECIFIED.,.F.,.F.,(4,2,4),(0.223030667259692,0.241734353696198,
0.260285072590615),.UNSPECIFIED.);
#5423=B_SPLINE_CURVE_WITH_KNOTS('',3,(#65024,#65025,#65026,#65027,#65028,
#65029,#65030,#65031,#65032,#65033,#65034,#65035,#65036,#65037,#65038,#65039,
#65040,#65041,#65042,#65043,#65044,#65045,#65046,#65047,#65048,#65049,#65050,
#65051,#65052,#65053,#65054,#65055,#65056,#65057,#65058,#65059,#65060,#65061,
#65062,#65063,#65064,#65065,#65066,#65067,#65068,#65069,#65070,#65071,#65072,
#65073,#65074,#65075,#65076,#65077,#65078,#65079,#65080,#65081,#65082,#65083,
#65084),.UNSPECIFIED.,.F.,.F.,(4,3,3,3,3,3,3,3,3,3,3,3,3,3,3,3,3,3,3,3,
4),(0.,0.0079599254395225,0.0158204416142309,0.016875819825814,0.0195772972159418,
0.027458899300654,0.0354166538447342,0.0390209976709895,0.0469884348389785,
0.050553508752619,0.0584240670042285,0.0663285883843651,0.0742861746184472,
0.0778995393741052,0.0842874233172974,0.0922711899963051,0.0975220154528314,
0.105525144757553,0.107817293670496,0.115774466404379,0.118118654117369),
 .UNSPECIFIED.);
#5424=B_SPLINE_CURVE_WITH_KNOTS('',3,(#65089,#65090,#65091,#65092,#65093,
#65094),.UNSPECIFIED.,.F.,.F.,(4,2,4),(-0.0161375727826142,0.,0.000421605906895856),
 .UNSPECIFIED.);
#5425=B_SPLINE_CURVE_WITH_KNOTS('',3,(#65144,#65145,#65146,#65147,#65148,
#65149,#65150,#65151,#65152,#65153,#65154,#65155,#65156,#65157,#65158,#65159,
#65160,#65161,#65162,#65163,#65164,#65165,#65166,#65167,#65168,#65169,#65170,
#65171,#65172,#65173,#65174,#65175,#65176,#65177,#65178,#65179,#65180,#65181,
#65182,#65183,#65184,#65185,#65186,#65187,#65188,#65189,#65190,#65191,#65192,
#65193,#65194,#65195,#65196,#65197,#65198,#65199,#65200,#65201,#65202,#65203,
#65204),.UNSPECIFIED.,.F.,.F.,(4,3,3,3,3,3,3,3,3,3,3,3,3,3,3,3,3,3,3,3,
4),(0.,0.00788945390620875,0.0159107528337271,0.0198233466742035,0.0278090397101045,
0.0338830033915008,0.0395609471880769,0.047495504646808,0.05543216058732,
0.0591436409533866,0.0671079528129851,0.0676235550484156,0.0755926825994609,
0.0785910514609752,0.0865300392580439,0.0944439925210487,0.0979951919099191,
0.101302747945529,0.108060095589016,0.116004888439911,0.118137330218038),
 .UNSPECIFIED.);
#5426=B_SPLINE_CURVE_WITH_KNOTS('',3,(#65205,#65206,#65207,#65208),
 .UNSPECIFIED.,.F.,.F.,(4,4),(0.82916884759973,1.33025671401017),
 .UNSPECIFIED.);
#5427=B_SPLINE_CURVE_WITH_KNOTS('',3,(#65213,#65214,#65215,#65216,#65217,
#65218),.UNSPECIFIED.,.F.,.F.,(4,2,4),(0.0370807285215093,0.0556314474159263,
0.0743351338524322),.UNSPECIFIED.);
#5428=B_SPLINE_CURVE_WITH_KNOTS('',3,(#65227,#65228,#65229,#65230,#65231,
#65232,#65233,#65234,#65235,#65236),.UNSPECIFIED.,.F.,.F.,(4,2,2,2,4),(0.148746748488587,
0.167205194290616,0.185750729133706,0.204398921478351,0.223127503799962),
 .UNSPECIFIED.);
#5429=B_SPLINE_CURVE_WITH_KNOTS('',3,(#65265,#65266,#65267,#65268),
 .UNSPECIFIED.,.F.,.F.,(4,4),(0.829183372221167,1.33027123863146),
 .UNSPECIFIED.);
#5430=B_SPLINE_CURVE_WITH_KNOTS('',3,(#65305,#65306,#65307,#65308,#65309,
#65310,#65311,#65312,#65313,#65314,#65315,#65316,#65317,#65318,#65319,#65320,
#65321,#65322,#65323,#65324,#65325,#65326,#65327,#65328,#65329,#65330,#65331,
#65332,#65333,#65334,#65335,#65336,#65337,#65338,#65339,#65340,#65341,#65342,
#65343,#65344,#65345,#65346,#65347,#65348,#65349,#65350,#65351,#65352,#65353,
#65354,#65355,#65356,#65357,#65358,#65359,#65360,#65361,#65362,#65363,#65364,
#65365),.UNSPECIFIED.,.F.,.F.,(4,3,3,3,3,3,3,3,3,3,3,3,3,3,3,3,3,3,3,3,
4),(0.,0.00788945390620776,0.0159107528337215,0.019823346674202,0.0278090397100862,
0.0338830033914998,0.0395609471880765,0.0474955046467828,0.055432160587273,
0.0591436409533932,0.0671079528129883,0.0676235550484267,0.0755926825994682,
0.0785910514609908,0.0865300392580284,0.0944439925209911,0.0979951919099412,
0.101302747945553,0.108060095589036,0.116004888440633,0.118137330218056),
 .UNSPECIFIED.);
#5431=B_SPLINE_CURVE_WITH_KNOTS('',3,(#65366,#65367,#65368,#65369),
 .UNSPECIFIED.,.F.,.F.,(4,4),(0.829168847599735,1.33025671401018),
 .UNSPECIFIED.);
#5432=B_SPLINE_CURVE_WITH_KNOTS('',3,(#65383,#65384,#65385,#65386,#65387,
#65388,#65389,#65390,#65391,#65392),.UNSPECIFIED.,.F.,.F.,(4,2,2,2,4),(0.148746748488587,
0.167205194290616,0.185750729133706,0.204398921478351,0.223127503799961),
 .UNSPECIFIED.);
#5433=B_SPLINE_CURVE_WITH_KNOTS('',3,(#65398,#65399,#65400,#65401,#65402,
#65403),.UNSPECIFIED.,.F.,.F.,(4,2,4),(-0.200640408047776,-0.200218802140828,
-0.184081233349071),.UNSPECIFIED.);
#5434=B_SPLINE_CURVE_WITH_KNOTS('',3,(#65422,#65423,#65424,#65425),
 .UNSPECIFIED.,.F.,.F.,(4,4),(-0.08135049134023,-0.0743659931772121),
 .UNSPECIFIED.);
#5435=B_SPLINE_CURVE_WITH_KNOTS('',3,(#65434,#65435,#65436,#65437),
 .UNSPECIFIED.,.F.,.F.,(4,4),(-0.170732657218268,-0.156799509139685),
 .UNSPECIFIED.);
#5436=B_SPLINE_CURVE_WITH_KNOTS('',3,(#65439,#65440,#65441,#65442,#65443,
#65444),.UNSPECIFIED.,.F.,.F.,(4,2,4),(0.0250159248865165,0.262677835658091,
0.516689802275816),.UNSPECIFIED.);
#5437=B_SPLINE_CURVE_WITH_KNOTS('',3,(#65445,#65446,#65447,#65448),
 .UNSPECIFIED.,.F.,.F.,(4,4),(-0.35545892019756,-0.309416993782686),
 .UNSPECIFIED.);
#5438=B_SPLINE_CURVE_WITH_KNOTS('',3,(#65449,#65450,#65451,#65452,#65453,
#65454),.UNSPECIFIED.,.F.,.F.,(4,2,4),(0.0370807285215092,0.0556314474159263,
0.0743351338524322),.UNSPECIFIED.);
#5439=B_SPLINE_CURVE_WITH_KNOTS('',3,(#65466,#65467,#65468,#65469),
 .UNSPECIFIED.,.F.,.F.,(4,4),(-0.223127503799962,-0.216143005636944),
 .UNSPECIFIED.);
#5440=B_SPLINE_CURVE_WITH_KNOTS('',3,(#65481,#65482,#65483,#65484,#65485,
#65486,#65487,#65488,#65489,#65490,#65491,#65492),.UNSPECIFIED.,.F.,.F.,
(4,2,2,2,2,4),(0.,0.0146453155547523,0.0329425480524922,0.0585813427772626,
0.0866269082173564,0.08706621227491),.UNSPECIFIED.);
#5441=B_SPLINE_CURVE_WITH_KNOTS('',3,(#65494,#65495,#65496,#65497,#65498,
#65499,#65500,#65501,#65502,#65503,#65504,#65505),.UNSPECIFIED.,.F.,.F.,
(4,2,2,2,2,4),(-0.00044410187836752,0.,0.0380815409759577,0.0676748364251937,
0.0897163855604342,0.098171512873764),.UNSPECIFIED.);
#5442=LINE('',#27824,#6334);
#5443=LINE('',#27854,#6335);
#5444=LINE('',#27858,#6336);
#5445=LINE('',#27862,#6337);
#5446=LINE('',#27867,#6338);
#5447=LINE('',#27895,#6339);
#5448=LINE('',#27899,#6340);
#5449=LINE('',#27904,#6341);
#5450=LINE('',#27964,#6342);
#5451=LINE('',#28024,#6343);
#5452=LINE('',#28081,#6344);
#5453=LINE('',#28141,#6345);
#5454=LINE('',#28201,#6346);
#5455=LINE('',#28261,#6347);
#5456=LINE('',#28318,#6348);
#5457=LINE('',#28375,#6349);
#5458=LINE('',#28438,#6350);
#5459=LINE('',#28492,#6351);
#5460=LINE('',#28552,#6352);
#5461=LINE('',#28612,#6353);
#5462=LINE('',#28669,#6354);
#5463=LINE('',#28726,#6355);
#5464=LINE('',#28792,#6356);
#5465=LINE('',#28852,#6357);
#5466=LINE('',#28909,#6358);
#5467=LINE('',#28966,#6359);
#5468=LINE('',#29029,#6360);
#5469=LINE('',#29083,#6361);
#5470=LINE('',#29140,#6362);
#5471=LINE('',#29200,#6363);
#5472=LINE('',#29257,#6364);
#5473=LINE('',#29314,#6365);
#5474=LINE('',#29380,#6366);
#5475=LINE('',#29440,#6367);
#5476=LINE('',#29497,#6368);
#5477=LINE('',#29554,#6369);
#5478=LINE('',#29614,#6370);
#5479=LINE('',#29668,#6371);
#5480=LINE('',#29725,#6372);
#5481=LINE('',#29788,#6373);
#5482=LINE('',#29848,#6374);
#5483=LINE('',#29902,#6375);
#5484=LINE('',#29962,#6376);
#5485=LINE('',#30022,#6377);
#5486=LINE('',#30079,#6378);
#5487=LINE('',#30139,#6379);
#5488=LINE('',#30199,#6380);
#5489=LINE('',#30256,#6381);
#5490=LINE('',#30316,#6382);
#5491=LINE('',#30376,#6383);
#5492=LINE('',#30436,#6384);
#5493=LINE('',#30490,#6385);
#5494=LINE('',#30547,#6386);
#5495=LINE('',#30610,#6387);
#5496=LINE('',#30667,#6388);
#5497=LINE('',#30727,#6389);
#5498=LINE('',#30787,#6390);
#5499=LINE('',#30844,#6391);
#5500=LINE('',#30904,#6392);
#5501=LINE('',#30967,#6393);
#5502=LINE('',#31027,#6394);
#5503=LINE('',#31081,#6395);
#5504=LINE('',#31138,#6396);
#5505=LINE('',#31198,#6397);
#5506=LINE('',#31255,#6398);
#5507=LINE('',#31312,#6399);
#5508=LINE('',#31372,#6400);
#5509=LINE('',#31429,#6401);
#5510=LINE('',#31489,#6402);
#5511=LINE('',#31507,#6403);
#5512=LINE('',#31521,#6404);
#5513=LINE('',#31611,#6405);
#5514=LINE('',#31695,#6406);
#5515=LINE('',#31785,#6407);
#5516=LINE('',#31875,#6408);
#5517=LINE('',#31959,#6409);
#5518=LINE('',#32049,#6410);
#5519=LINE('',#32133,#6411);
#5520=LINE('',#32223,#6412);
#5521=LINE('',#32313,#6413);
#5522=LINE('',#32397,#6414);
#5523=LINE('',#32487,#6415);
#5524=LINE('',#32577,#6416);
#5525=LINE('',#32661,#6417);
#5526=LINE('',#32751,#6418);
#5527=LINE('',#32835,#6419);
#5528=LINE('',#32857,#6420);
#5529=LINE('',#32894,#6421);
#5530=LINE('',#32931,#6422);
#5531=LINE('',#32968,#6423);
#5532=LINE('',#33005,#6424);
#5533=LINE('',#33043,#6425);
#5534=LINE('',#33080,#6426);
#5535=LINE('',#33117,#6427);
#5536=LINE('',#33155,#6428);
#5537=LINE('',#33192,#6429);
#5538=LINE('',#33229,#6430);
#5539=LINE('',#33266,#6431);
#5540=LINE('',#33303,#6432);
#5541=LINE('',#33341,#6433);
#5542=LINE('',#33378,#6434);
#5543=LINE('',#33415,#6435);
#5544=LINE('',#33428,#6436);
#5545=LINE('',#33459,#6437);
#5546=LINE('',#33487,#6438);
#5547=LINE('',#33515,#6439);
#5548=LINE('',#33556,#6440);
#5549=LINE('',#33597,#6441);
#5550=LINE('',#33625,#6442);
#5551=LINE('',#33653,#6443);
#5552=LINE('',#33694,#6444);
#5553=LINE('',#33735,#6445);
#5554=LINE('',#33764,#6446);
#5555=LINE('',#33792,#6447);
#5556=LINE('',#33820,#6448);
#5557=LINE('',#33848,#6449);
#5558=LINE('',#33889,#6450);
#5559=LINE('',#33930,#6451);
#5560=LINE('',#33958,#6452);
#5561=LINE('',#33986,#6453);
#5562=LINE('',#34027,#6454);
#5563=LINE('',#34068,#6455);
#5564=LINE('',#34097,#6456);
#5565=LINE('',#34125,#6457);
#5566=LINE('',#34153,#6458);
#5567=LINE('',#34181,#6459);
#5568=LINE('',#34222,#6460);
#5569=LINE('',#34263,#6461);
#5570=LINE('',#34291,#6462);
#5571=LINE('',#34318,#6463);
#5572=LINE('',#34360,#6464);
#5573=LINE('',#34401,#6465);
#5574=LINE('',#34430,#6466);
#5575=LINE('',#34457,#6467);
#5576=LINE('',#34498,#6468);
#5577=LINE('',#34540,#6469);
#5578=LINE('',#34568,#6470);
#5579=LINE('',#34595,#6471);
#5580=LINE('',#34636,#6472);
#5581=LINE('',#34665,#6473);
#5582=LINE('',#34707,#6474);
#5583=LINE('',#34734,#6475);
#5584=LINE('',#34775,#6476);
#5585=LINE('',#34804,#6477);
#5586=LINE('',#34845,#6478);
#5587=LINE('',#34887,#6479);
#5588=LINE('',#34915,#6480);
#5589=LINE('',#34942,#6481);
#5590=LINE('',#34983,#6482);
#5591=LINE('',#35012,#6483);
#5592=LINE('',#35041,#6484);
#5593=LINE('',#35068,#6485);
#5594=LINE('',#35109,#6486);
#5595=LINE('',#35138,#6487);
#5596=LINE('',#35179,#6488);
#5597=LINE('',#35221,#6489);
#5598=LINE('',#35249,#6490);
#5599=LINE('',#35276,#6491);
#5600=LINE('',#35317,#6492);
#5601=LINE('',#35346,#6493);
#5602=LINE('',#35375,#6494);
#5603=LINE('',#35402,#6495);
#5604=LINE('',#35430,#6496);
#5605=LINE('',#35459,#6497);
#5606=LINE('',#35498,#6498);
#5607=LINE('',#35499,#6499);
#5608=LINE('',#35501,#6500);
#5609=LINE('',#35503,#6501);
#5610=LINE('',#42509,#6502);
#5611=LINE('',#42549,#6503);
#5612=LINE('',#42861,#6504);
#5613=LINE('',#42901,#6505);
#5614=LINE('',#43183,#6506);
#5615=LINE('',#43223,#6507);
#5616=LINE('',#43505,#6508);
#5617=LINE('',#43545,#6509);
#5618=LINE('',#43827,#6510);
#5619=LINE('',#43880,#6511);
#5620=LINE('',#44162,#6512);
#5621=LINE('',#44202,#6513);
#5622=LINE('',#44484,#6514);
#5623=LINE('',#44524,#6515);
#5624=LINE('',#44810,#6516);
#5625=LINE('',#44850,#6517);
#5626=LINE('',#45134,#6518);
#5627=LINE('',#45174,#6519);
#5628=LINE('',#45456,#6520);
#5629=LINE('',#45496,#6521);
#5630=LINE('',#45778,#6522);
#5631=LINE('',#45818,#6523);
#5632=LINE('',#46106,#6524);
#5633=LINE('',#46146,#6525);
#5634=LINE('',#46428,#6526);
#5635=LINE('',#46468,#6527);
#5636=LINE('',#46750,#6528);
#5637=LINE('',#46790,#6529);
#5638=LINE('',#47037,#6530);
#5639=LINE('',#47099,#6531);
#5640=LINE('',#47227,#6532);
#5641=LINE('',#47229,#6533);
#5642=LINE('',#47231,#6534);
#5643=LINE('',#47237,#6535);
#5644=LINE('',#47245,#6536);
#5645=LINE('',#47248,#6537);
#5646=LINE('',#47259,#6538);
#5647=LINE('',#47262,#6539);
#5648=LINE('',#47268,#6540);
#5649=LINE('',#47270,#6541);
#5650=LINE('',#47286,#6542);
#5651=LINE('',#47287,#6543);
#5652=LINE('',#47292,#6544);
#5653=LINE('',#47294,#6545);
#5654=LINE('',#47299,#6546);
#5655=LINE('',#47302,#6547);
#5656=LINE('',#47304,#6548);
#5657=LINE('',#47307,#6549);
#5658=LINE('',#47311,#6550);
#5659=LINE('',#47312,#6551);
#5660=LINE('',#47315,#6552);
#5661=LINE('',#47318,#6553);
#5662=LINE('',#47320,#6554);
#5663=LINE('',#47321,#6555);
#5664=LINE('',#47324,#6556);
#5665=LINE('',#47329,#6557);
#5666=LINE('',#47333,#6558);
#5667=LINE('',#47348,#6559);
#5668=LINE('',#47350,#6560);
#5669=LINE('',#47355,#6561);
#5670=LINE('',#47359,#6562);
#5671=LINE('',#47363,#6563);
#5672=LINE('',#47369,#6564);
#5673=LINE('',#47372,#6565);
#5674=LINE('',#47375,#6566);
#5675=LINE('',#47377,#6567);
#5676=LINE('',#47378,#6568);
#5677=LINE('',#47388,#6569);
#5678=LINE('',#47391,#6570);
#5679=LINE('',#47407,#6571);
#5680=LINE('',#47410,#6572);
#5681=LINE('',#47413,#6573);
#5682=LINE('',#47416,#6574);
#5683=LINE('',#47420,#6575);
#5684=LINE('',#47421,#6576);
#5685=LINE('',#47426,#6577);
#5686=LINE('',#47427,#6578);
#5687=LINE('',#47430,#6579);
#5688=LINE('',#47433,#6580);
#5689=LINE('',#47437,#6581);
#5690=LINE('',#47440,#6582);
#5691=LINE('',#47443,#6583);
#5692=LINE('',#47445,#6584);
#5693=LINE('',#47447,#6585);
#5694=LINE('',#47448,#6586);
#5695=LINE('',#47463,#6587);
#5696=LINE('',#47469,#6588);
#5697=LINE('',#47472,#6589);
#5698=LINE('',#47479,#6590);
#5699=LINE('',#47487,#6591);
#5700=LINE('',#47510,#6592);
#5701=LINE('',#47513,#6593);
#5702=LINE('',#47518,#6594);
#5703=LINE('',#47521,#6595);
#5704=LINE('',#47530,#6596);
#5705=LINE('',#47532,#6597);
#5706=LINE('',#47533,#6598);
#5707=LINE('',#47536,#6599);
#5708=LINE('',#47538,#6600);
#5709=LINE('',#47539,#6601);
#5710=LINE('',#47545,#6602);
#5711=LINE('',#47552,#6603);
#5712=LINE('',#47558,#6604);
#5713=LINE('',#47564,#6605);
#5714=LINE('',#47568,#6606);
#5715=LINE('',#47569,#6607);
#5716=LINE('',#47572,#6608);
#5717=LINE('',#47576,#6609);
#5718=LINE('',#47577,#6610);
#5719=LINE('',#47580,#6611);
#5720=LINE('',#47584,#6612);
#5721=LINE('',#47585,#6613);
#5722=LINE('',#47588,#6614);
#5723=LINE('',#47595,#6615);
#5724=LINE('',#47598,#6616);
#5725=LINE('',#47614,#6617);
#5726=LINE('',#47617,#6618);
#5727=LINE('',#47623,#6619);
#5728=LINE('',#47625,#6620);
#5729=LINE('',#47626,#6621);
#5730=LINE('',#47629,#6622);
#5731=LINE('',#47638,#6623);
#5732=LINE('',#47644,#6624);
#5733=LINE('',#47650,#6625);
#5734=LINE('',#47651,#6626);
#5735=LINE('',#47667,#6627);
#5736=LINE('',#47670,#6628);
#5737=LINE('',#47677,#6629);
#5738=LINE('',#47682,#6630);
#5739=LINE('',#47688,#6631);
#5740=LINE('',#47691,#6632);
#5741=LINE('',#47693,#6633);
#5742=LINE('',#47694,#6634);
#5743=LINE('',#47699,#6635);
#5744=LINE('',#47704,#6636);
#5745=LINE('',#47708,#6637);
#5746=LINE('',#47709,#6638);
#5747=LINE('',#47726,#6639);
#5748=LINE('',#47730,#6640);
#5749=LINE('',#47737,#6641);
#5750=LINE('',#47740,#6642);
#5751=LINE('',#47746,#6643);
#5752=LINE('',#47748,#6644);
#5753=LINE('',#47749,#6645);
#5754=LINE('',#47752,#6646);
#5755=LINE('',#47758,#6647);
#5756=LINE('',#47759,#6648);
#5757=LINE('',#47764,#6649);
#5758=LINE('',#47770,#6650);
#5759=LINE('',#47773,#6651);
#5760=LINE('',#47779,#6652);
#5761=LINE('',#47782,#6653);
#5762=LINE('',#47797,#6654);
#5763=LINE('',#47800,#6655);
#5764=LINE('',#47803,#6656);
#5765=LINE('',#47806,#6657);
#5766=LINE('',#47809,#6658);
#5767=LINE('',#47812,#6659);
#5768=LINE('',#47815,#6660);
#5769=LINE('',#47816,#6661);
#5770=LINE('',#47819,#6662);
#5771=LINE('',#47826,#6663);
#5772=LINE('',#47828,#6664);
#5773=LINE('',#47839,#6665);
#5774=LINE('',#47841,#6666);
#5775=LINE('',#47845,#6667);
#5776=LINE('',#47849,#6668);
#5777=LINE('',#47850,#6669);
#5778=LINE('',#47853,#6670);
#5779=LINE('',#47857,#6671);
#5780=LINE('',#47858,#6672);
#5781=LINE('',#47864,#6673);
#5782=LINE('',#47865,#6674);
#5783=LINE('',#47869,#6675);
#5784=LINE('',#47872,#6676);
#5785=LINE('',#47874,#6677);
#5786=LINE('',#47879,#6678);
#5787=LINE('',#47881,#6679);
#5788=LINE('',#47886,#6680);
#5789=LINE('',#47891,#6681);
#5790=LINE('',#47893,#6682);
#5791=LINE('',#47894,#6683);
#5792=LINE('',#47901,#6684);
#5793=LINE('',#47904,#6685);
#5794=LINE('',#47906,#6686);
#5795=LINE('',#47908,#6687);
#5796=LINE('',#47909,#6688);
#5797=LINE('',#47922,#6689);
#5798=LINE('',#47935,#6690);
#5799=LINE('',#47955,#6691);
#5800=LINE('',#47961,#6692);
#5801=LINE('',#47974,#6693);
#5802=LINE('',#47978,#6694);
#5803=LINE('',#47982,#6695);
#5804=LINE('',#47986,#6696);
#5805=LINE('',#47990,#6697);
#5806=LINE('',#47994,#6698);
#5807=LINE('',#47998,#6699);
#5808=LINE('',#48002,#6700);
#5809=LINE('',#48006,#6701);
#5810=LINE('',#48025,#6702);
#5811=LINE('',#48029,#6703);
#5812=LINE('',#48050,#6704);
#5813=LINE('',#48051,#6705);
#5814=LINE('',#48106,#6706);
#5815=LINE('',#48110,#6707);
#5816=LINE('',#48114,#6708);
#5817=LINE('',#48118,#6709);
#5818=LINE('',#48122,#6710);
#5819=LINE('',#48126,#6711);
#5820=LINE('',#48145,#6712);
#5821=LINE('',#48176,#6713);
#5822=LINE('',#48201,#6714);
#5823=LINE('',#48225,#6715);
#5824=LINE('',#48234,#6716);
#5825=LINE('',#48235,#6717);
#5826=LINE('',#48251,#6718);
#5827=LINE('',#48341,#6719);
#5828=LINE('',#48358,#6720);
#5829=LINE('',#48367,#6721);
#5830=LINE('',#48368,#6722);
#5831=LINE('',#48391,#6723);
#5832=LINE('',#48392,#6724);
#5833=LINE('',#48413,#6725);
#5834=LINE('',#48414,#6726);
#5835=LINE('',#48445,#6727);
#5836=LINE('',#48449,#6728);
#5837=LINE('',#48458,#6729);
#5838=LINE('',#48459,#6730);
#5839=LINE('',#48481,#6731);
#5840=LINE('',#48538,#6732);
#5841=LINE('',#48541,#6733);
#5842=LINE('',#48599,#6734);
#5843=LINE('',#48605,#6735);
#5844=LINE('',#48612,#6736);
#5845=LINE('',#48616,#6737);
#5846=LINE('',#48619,#6738);
#5847=LINE('',#48621,#6739);
#5848=LINE('',#48622,#6740);
#5849=LINE('',#48635,#6741);
#5850=LINE('',#48650,#6742);
#5851=LINE('',#48651,#6743);
#5852=LINE('',#48654,#6744);
#5853=LINE('',#48656,#6745);
#5854=LINE('',#48658,#6746);
#5855=LINE('',#48660,#6747);
#5856=LINE('',#48661,#6748);
#5857=LINE('',#48664,#6749);
#5858=LINE('',#48671,#6750);
#5859=LINE('',#48677,#6751);
#5860=LINE('',#48681,#6752);
#5861=LINE('',#48685,#6753);
#5862=LINE('',#48689,#6754);
#5863=LINE('',#48690,#6755);
#5864=LINE('',#48695,#6756);
#5865=LINE('',#48702,#6757);
#5866=LINE('',#48704,#6758);
#5867=LINE('',#48705,#6759);
#5868=LINE('',#48708,#6760);
#5869=LINE('',#48711,#6761);
#5870=LINE('',#48714,#6762);
#5871=LINE('',#48735,#6763);
#5872=LINE('',#48744,#6764);
#5873=LINE('',#48750,#6765);
#5874=LINE('',#48755,#6766);
#5875=LINE('',#48765,#6767);
#5876=LINE('',#48768,#6768);
#5877=LINE('',#48770,#6769);
#5878=LINE('',#48774,#6770);
#5879=LINE('',#48777,#6771);
#5880=LINE('',#48782,#6772);
#5881=LINE('',#48785,#6773);
#5882=LINE('',#48789,#6774);
#5883=LINE('',#48790,#6775);
#5884=LINE('',#48803,#6776);
#5885=LINE('',#48818,#6777);
#5886=LINE('',#48836,#6778);
#5887=LINE('',#48839,#6779);
#5888=LINE('',#48840,#6780);
#5889=LINE('',#48843,#6781);
#5890=LINE('',#48849,#6782);
#5891=LINE('',#48851,#6783);
#5892=LINE('',#48853,#6784);
#5893=LINE('',#48854,#6785);
#5894=LINE('',#48863,#6786);
#5895=LINE('',#48873,#6787);
#5896=LINE('',#48911,#6788);
#5897=LINE('',#48921,#6789);
#5898=LINE('',#48937,#6790);
#5899=LINE('',#48951,#6791);
#5900=LINE('',#48964,#6792);
#5901=LINE('',#48977,#6793);
#5902=LINE('',#48983,#6794);
#5903=LINE('',#48986,#6795);
#5904=LINE('',#48989,#6796);
#5905=LINE('',#48994,#6797);
#5906=LINE('',#48996,#6798);
#5907=LINE('',#49003,#6799);
#5908=LINE('',#49042,#6800);
#5909=LINE('',#49050,#6801);
#5910=LINE('',#49085,#6802);
#5911=LINE('',#49097,#6803);
#5912=LINE('',#49113,#6804);
#5913=LINE('',#49124,#6805);
#5914=LINE('',#49163,#6806);
#5915=LINE('',#49164,#6807);
#5916=LINE('',#49172,#6808);
#5917=LINE('',#49180,#6809);
#5918=LINE('',#49188,#6810);
#5919=LINE('',#49197,#6811);
#5920=LINE('',#49204,#6812);
#5921=LINE('',#49212,#6813);
#5922=LINE('',#49220,#6814);
#5923=LINE('',#49222,#6815);
#5924=LINE('',#49224,#6816);
#5925=LINE('',#49226,#6817);
#5926=LINE('',#49234,#6818);
#5927=LINE('',#49238,#6819);
#5928=LINE('',#50086,#6820);
#5929=LINE('',#51702,#6821);
#5930=LINE('',#51747,#6822);
#5931=LINE('',#52007,#6823);
#5932=LINE('',#52017,#6824);
#5933=LINE('',#54592,#6825);
#5934=LINE('',#54594,#6826);
#5935=LINE('',#54778,#6827);
#5936=LINE('',#54786,#6828);
#5937=LINE('',#54978,#6829);
#5938=LINE('',#54980,#6830);
#5939=LINE('',#55164,#6831);
#5940=LINE('',#55172,#6832);
#5941=LINE('',#55358,#6833);
#5942=LINE('',#55360,#6834);
#5943=LINE('',#55544,#6835);
#5944=LINE('',#55552,#6836);
#5945=LINE('',#55741,#6837);
#5946=LINE('',#55743,#6838);
#5947=LINE('',#55927,#6839);
#5948=LINE('',#55935,#6840);
#5949=LINE('',#56121,#6841);
#5950=LINE('',#56123,#6842);
#5951=LINE('',#56307,#6843);
#5952=LINE('',#56315,#6844);
#5953=LINE('',#56507,#6845);
#5954=LINE('',#56509,#6846);
#5955=LINE('',#56691,#6847);
#5956=LINE('',#56699,#6848);
#5957=LINE('',#56865,#6849);
#5958=LINE('',#56878,#6850);
#5959=LINE('',#57089,#6851);
#5960=LINE('',#57102,#6852);
#5961=LINE('',#57287,#6853);
#5962=LINE('',#57300,#6854);
#5963=LINE('',#57485,#6855);
#5964=LINE('',#57498,#6856);
#5965=LINE('',#57683,#6857);
#5966=LINE('',#57696,#6858);
#5967=LINE('',#57881,#6859);
#5968=LINE('',#57894,#6860);
#5969=LINE('',#58093,#6861);
#5970=LINE('',#58119,#6862);
#5971=LINE('',#58304,#6863);
#5972=LINE('',#58317,#6864);
#5973=LINE('',#58502,#6865);
#5974=LINE('',#58515,#6866);
#5975=LINE('',#58700,#6867);
#5976=LINE('',#58713,#6868);
#5977=LINE('',#58898,#6869);
#5978=LINE('',#58911,#6870);
#5979=LINE('',#59096,#6871);
#5980=LINE('',#59109,#6872);
#5981=LINE('',#59310,#6873);
#5982=LINE('',#59323,#6874);
#5983=LINE('',#59520,#6875);
#5984=LINE('',#59533,#6876);
#5985=LINE('',#59718,#6877);
#5986=LINE('',#59731,#6878);
#5987=LINE('',#59916,#6879);
#5988=LINE('',#59929,#6880);
#5989=LINE('',#60114,#6881);
#5990=LINE('',#60127,#6882);
#5991=LINE('',#60312,#6883);
#5992=LINE('',#60325,#6884);
#5993=LINE('',#60524,#6885);
#5994=LINE('',#60537,#6886);
#5995=LINE('',#60734,#6887);
#5996=LINE('',#60747,#6888);
#5997=LINE('',#60932,#6889);
#5998=LINE('',#60945,#6890);
#5999=LINE('',#61130,#6891);
#6000=LINE('',#61143,#6892);
#6001=LINE('',#61328,#6893);
#6002=LINE('',#61341,#6894);
#6003=LINE('',#61526,#6895);
#6004=LINE('',#61539,#6896);
#6005=LINE('',#61724,#6897);
#6006=LINE('',#61737,#6898);
#6007=LINE('',#61837,#6899);
#6008=LINE('',#61850,#6900);
#6009=LINE('',#61862,#6901);
#6010=LINE('',#61877,#6902);
#6011=LINE('',#61880,#6903);
#6012=LINE('',#61891,#6904);
#6013=LINE('',#61892,#6905);
#6014=LINE('',#61898,#6906);
#6015=LINE('',#61901,#6907);
#6016=LINE('',#61904,#6908);
#6017=LINE('',#61905,#6909);
#6018=LINE('',#61914,#6910);
#6019=LINE('',#61924,#6911);
#6020=LINE('',#61925,#6912);
#6021=LINE('',#61929,#6913);
#6022=LINE('',#61939,#6914);
#6023=LINE('',#61957,#6915);
#6024=LINE('',#61970,#6916);
#6025=LINE('',#61982,#6917);
#6026=LINE('',#62020,#6918);
#6027=LINE('',#62024,#6919);
#6028=LINE('',#62027,#6920);
#6029=LINE('',#62031,#6921);
#6030=LINE('',#62034,#6922);
#6031=LINE('',#62044,#6923);
#6032=LINE('',#62045,#6924);
#6033=LINE('',#62050,#6925);
#6034=LINE('',#62051,#6926);
#6035=LINE('',#62064,#6927);
#6036=LINE('',#62065,#6928);
#6037=LINE('',#62070,#6929);
#6038=LINE('',#62074,#6930);
#6039=LINE('',#62077,#6931);
#6040=LINE('',#62078,#6932);
#6041=LINE('',#62080,#6933);
#6042=LINE('',#62084,#6934);
#6043=LINE('',#62087,#6935);
#6044=LINE('',#62093,#6936);
#6045=LINE('',#62095,#6937);
#6046=LINE('',#62096,#6938);
#6047=LINE('',#62101,#6939);
#6048=LINE('',#62121,#6940);
#6049=LINE('',#62125,#6941);
#6050=LINE('',#62128,#6942);
#6051=LINE('',#62134,#6943);
#6052=LINE('',#62137,#6944);
#6053=LINE('',#62145,#6945);
#6054=LINE('',#62148,#6946);
#6055=LINE('',#62152,#6947);
#6056=LINE('',#62154,#6948);
#6057=LINE('',#62161,#6949);
#6058=LINE('',#62165,#6950);
#6059=LINE('',#62168,#6951);
#6060=LINE('',#62169,#6952);
#6061=LINE('',#62171,#6953);
#6062=LINE('',#62183,#6954);
#6063=LINE('',#62184,#6955);
#6064=LINE('',#62190,#6956);
#6065=LINE('',#62192,#6957);
#6066=LINE('',#62193,#6958);
#6067=LINE('',#62195,#6959);
#6068=LINE('',#62196,#6960);
#6069=LINE('',#62203,#6961);
#6070=LINE('',#62209,#6962);
#6071=LINE('',#62212,#6963);
#6072=LINE('',#62223,#6964);
#6073=LINE('',#62226,#6965);
#6074=LINE('',#62229,#6966);
#6075=LINE('',#62232,#6967);
#6076=LINE('',#62235,#6968);
#6077=LINE('',#62236,#6969);
#6078=LINE('',#62256,#6970);
#6079=LINE('',#62259,#6971);
#6080=LINE('',#62262,#6972);
#6081=LINE('',#62266,#6973);
#6082=LINE('',#62269,#6974);
#6083=LINE('',#62275,#6975);
#6084=LINE('',#62278,#6976);
#6085=LINE('',#62295,#6977);
#6086=LINE('',#62300,#6978);
#6087=LINE('',#62304,#6979);
#6088=LINE('',#62308,#6980);
#6089=LINE('',#62310,#6981);
#6090=LINE('',#62313,#6982);
#6091=LINE('',#62314,#6983);
#6092=LINE('',#62319,#6984);
#6093=LINE('',#62395,#6985);
#6094=LINE('',#62399,#6986);
#6095=LINE('',#62402,#6987);
#6096=LINE('',#62403,#6988);
#6097=LINE('',#62404,#6989);
#6098=LINE('',#62405,#6990);
#6099=LINE('',#62406,#6991);
#6100=LINE('',#62407,#6992);
#6101=LINE('',#62412,#6993);
#6102=LINE('',#62426,#6994);
#6103=LINE('',#62438,#6995);
#6104=LINE('',#62447,#6996);
#6105=LINE('',#62450,#6997);
#6106=LINE('',#62455,#6998);
#6107=LINE('',#62458,#6999);
#6108=LINE('',#62463,#7000);
#6109=LINE('',#62466,#7001);
#6110=LINE('',#62477,#7002);
#6111=LINE('',#62478,#7003);
#6112=LINE('',#62481,#7004);
#6113=LINE('',#62485,#7005);
#6114=LINE('',#62486,#7006);
#6115=LINE('',#62489,#7007);
#6116=LINE('',#62493,#7008);
#6117=LINE('',#62494,#7009);
#6118=LINE('',#62503,#7010);
#6119=LINE('',#62514,#7011);
#6120=LINE('',#62530,#7012);
#6121=LINE('',#62536,#7013);
#6122=LINE('',#62539,#7014);
#6123=LINE('',#62542,#7015);
#6124=LINE('',#62543,#7016);
#6125=LINE('',#62547,#7017);
#6126=LINE('',#62551,#7018);
#6127=LINE('',#62557,#7019);
#6128=LINE('',#62568,#7020);
#6129=LINE('',#62578,#7021);
#6130=LINE('',#62589,#7022);
#6131=LINE('',#62591,#7023);
#6132=LINE('',#62592,#7024);
#6133=LINE('',#62596,#7025);
#6134=LINE('',#62598,#7026);
#6135=LINE('',#62599,#7027);
#6136=LINE('',#62603,#7028);
#6137=LINE('',#62605,#7029);
#6138=LINE('',#62606,#7030);
#6139=LINE('',#62610,#7031);
#6140=LINE('',#62612,#7032);
#6141=LINE('',#62613,#7033);
#6142=LINE('',#62615,#7034);
#6143=LINE('',#62616,#7035);
#6144=LINE('',#62620,#7036);
#6145=LINE('',#62622,#7037);
#6146=LINE('',#62623,#7038);
#6147=LINE('',#62627,#7039);
#6148=LINE('',#62629,#7040);
#6149=LINE('',#62630,#7041);
#6150=LINE('',#62632,#7042);
#6151=LINE('',#62633,#7043);
#6152=LINE('',#62637,#7044);
#6153=LINE('',#62639,#7045);
#6154=LINE('',#62640,#7046);
#6155=LINE('',#62642,#7047);
#6156=LINE('',#62643,#7048);
#6157=LINE('',#62645,#7049);
#6158=LINE('',#62646,#7050);
#6159=LINE('',#62650,#7051);
#6160=LINE('',#62652,#7052);
#6161=LINE('',#62653,#7053);
#6162=LINE('',#62655,#7054);
#6163=LINE('',#62656,#7055);
#6164=LINE('',#62658,#7056);
#6165=LINE('',#62659,#7057);
#6166=LINE('',#62661,#7058);
#6167=LINE('',#62662,#7059);
#6168=LINE('',#62664,#7060);
#6169=LINE('',#62665,#7061);
#6170=LINE('',#62667,#7062);
#6171=LINE('',#62668,#7063);
#6172=LINE('',#62670,#7064);
#6173=LINE('',#62671,#7065);
#6174=LINE('',#62673,#7066);
#6175=LINE('',#62674,#7067);
#6176=LINE('',#62676,#7068);
#6177=LINE('',#62677,#7069);
#6178=LINE('',#63541,#7070);
#6179=LINE('',#63545,#7071);
#6180=LINE('',#63553,#7072);
#6181=LINE('',#63555,#7073);
#6182=LINE('',#63557,#7074);
#6183=LINE('',#63567,#7075);
#6184=LINE('',#63569,#7076);
#6185=LINE('',#63571,#7077);
#6186=LINE('',#63579,#7078);
#6187=LINE('',#63581,#7079);
#6188=LINE('',#63583,#7080);
#6189=LINE('',#63591,#7081);
#6190=LINE('',#63592,#7082);
#6191=LINE('',#63600,#7083);
#6192=LINE('',#63604,#7084);
#6193=LINE('',#63606,#7085);
#6194=LINE('',#63608,#7086);
#6195=LINE('',#63612,#7087);
#6196=LINE('',#63614,#7088);
#6197=LINE('',#63616,#7089);
#6198=LINE('',#63622,#7090);
#6199=LINE('',#63624,#7091);
#6200=LINE('',#63626,#7092);
#6201=LINE('',#63632,#7093);
#6202=LINE('',#63633,#7094);
#6203=LINE('',#63638,#7095);
#6204=LINE('',#63642,#7096);
#6205=LINE('',#63644,#7097);
#6206=LINE('',#63645,#7098);
#6207=LINE('',#63653,#7099);
#6208=LINE('',#63657,#7100);
#6209=LINE('',#63659,#7101);
#6210=LINE('',#63660,#7102);
#6211=LINE('',#63668,#7103);
#6212=LINE('',#63672,#7104);
#6213=LINE('',#63674,#7105);
#6214=LINE('',#63675,#7106);
#6215=LINE('',#63696,#7107);
#6216=LINE('',#63699,#7108);
#6217=LINE('',#63708,#7109);
#6218=LINE('',#63711,#7110);
#6219=LINE('',#63786,#7111);
#6220=LINE('',#63793,#7112);
#6221=LINE('',#63794,#7113);
#6222=LINE('',#63813,#7114);
#6223=LINE('',#63829,#7115);
#6224=LINE('',#63833,#7116);
#6225=LINE('',#63837,#7117);
#6226=LINE('',#63841,#7118);
#6227=LINE('',#63845,#7119);
#6228=LINE('',#63849,#7120);
#6229=LINE('',#63853,#7121);
#6230=LINE('',#63856,#7122);
#6231=LINE('',#63864,#7123);
#6232=LINE('',#63959,#7124);
#6233=LINE('',#63962,#7125);
#6234=LINE('',#64073,#7126);
#6235=LINE('',#64075,#7127);
#6236=LINE('',#64078,#7128);
#6237=LINE('',#64080,#7129);
#6238=LINE('',#64087,#7130);
#6239=LINE('',#64110,#7131);
#6240=LINE('',#64120,#7132);
#6241=LINE('',#64134,#7133);
#6242=LINE('',#64137,#7134);
#6243=LINE('',#64139,#7135);
#6244=LINE('',#64200,#7136);
#6245=LINE('',#64222,#7137);
#6246=LINE('',#64224,#7138);
#6247=LINE('',#64230,#7139);
#6248=LINE('',#64233,#7140);
#6249=LINE('',#64237,#7141);
#6250=LINE('',#64241,#7142);
#6251=LINE('',#64268,#7143);
#6252=LINE('',#64271,#7144);
#6253=LINE('',#64316,#7145);
#6254=LINE('',#64330,#7146);
#6255=LINE('',#64354,#7147);
#6256=LINE('',#64369,#7148);
#6257=LINE('',#64371,#7149);
#6258=LINE('',#64374,#7150);
#6259=LINE('',#64376,#7151);
#6260=LINE('',#64379,#7152);
#6261=LINE('',#64381,#7153);
#6262=LINE('',#64384,#7154);
#6263=LINE('',#64388,#7155);
#6264=LINE('',#64391,#7156);
#6265=LINE('',#64393,#7157);
#6266=LINE('',#64397,#7158);
#6267=LINE('',#64400,#7159);
#6268=LINE('',#64403,#7160);
#6269=LINE('',#64405,#7161);
#6270=LINE('',#64409,#7162);
#6271=LINE('',#64449,#7163);
#6272=LINE('',#64451,#7164);
#6273=LINE('',#64452,#7165);
#6274=LINE('',#64455,#7166);
#6275=LINE('',#64495,#7167);
#6276=LINE('',#64497,#7168);
#6277=LINE('',#64498,#7169);
#6278=LINE('',#64540,#7170);
#6279=LINE('',#64563,#7171);
#6280=LINE('',#64566,#7172);
#6281=LINE('',#64569,#7173);
#6282=LINE('',#64594,#7174);
#6283=LINE('',#64601,#7175);
#6284=LINE('',#64605,#7176);
#6285=LINE('',#64616,#7177);
#6286=LINE('',#64623,#7178);
#6287=LINE('',#64637,#7179);
#6288=LINE('',#64653,#7180);
#6289=LINE('',#64661,#7181);
#6290=LINE('',#64663,#7182);
#6291=LINE('',#64738,#7183);
#6292=LINE('',#64750,#7184);
#6293=LINE('',#64773,#7185);
#6294=LINE('',#64774,#7186);
#6295=LINE('',#64789,#7187);
#6296=LINE('',#64826,#7188);
#6297=LINE('',#64829,#7189);
#6298=LINE('',#64842,#7190);
#6299=LINE('',#64911,#7191);
#6300=LINE('',#64913,#7192);
#6301=LINE('',#64916,#7193);
#6302=LINE('',#64929,#7194);
#6303=LINE('',#64998,#7195);
#6304=LINE('',#65000,#7196);
#6305=LINE('',#65003,#7197);
#6306=LINE('',#65016,#7198);
#6307=LINE('',#65085,#7199);
#6308=LINE('',#65096,#7200);
#6309=LINE('',#65100,#7201);
#6310=LINE('',#65110,#7202);
#6311=LINE('',#65111,#7203);
#6312=LINE('',#65210,#7204);
#6313=LINE('',#65222,#7205);
#6314=LINE('',#65371,#7206);
#6315=LINE('',#65375,#7207);
#6316=LINE('',#65379,#7208);
#6317=LINE('',#65407,#7209);
#6318=LINE('',#65412,#7210);
#6319=LINE('',#65413,#7211);
#6320=LINE('',#65415,#7212);
#6321=LINE('',#65418,#7213);
#6322=LINE('',#65420,#7214);
#6323=LINE('',#65426,#7215);
#6324=LINE('',#65430,#7216);
#6325=LINE('',#65456,#7217);
#6326=LINE('',#65461,#7218);
#6327=LINE('',#65464,#7219);
#6328=LINE('',#65471,#7220);
#6329=LINE('',#65472,#7221);
#6330=LINE('',#65474,#7222);
#6331=LINE('',#65476,#7223);
#6332=LINE('',#65478,#7224);
#6333=LINE('',#65511,#7225);
#6334=VECTOR('',#22409,7.);
#6335=VECTOR('',#22412,7.);
#6336=VECTOR('',#22415,10.);
#6337=VECTOR('',#22418,7.);
#6338=VECTOR('',#22423,10.);
#6339=VECTOR('',#22428,10.);
#6340=VECTOR('',#22431,10.);
#6341=VECTOR('',#22436,7.);
#6342=VECTOR('',#22439,7.);
#6343=VECTOR('',#22442,7.);
#6344=VECTOR('',#22445,7.);
#6345=VECTOR('',#22448,7.);
#6346=VECTOR('',#22451,7.);
#6347=VECTOR('',#22454,7.);
#6348=VECTOR('',#22457,7.);
#6349=VECTOR('',#22460,7.);
#6350=VECTOR('',#22463,7.);
#6351=VECTOR('',#22466,7.);
#6352=VECTOR('',#22469,7.);
#6353=VECTOR('',#22472,7.);
#6354=VECTOR('',#22475,7.);
#6355=VECTOR('',#22478,7.);
#6356=VECTOR('',#22481,7.);
#6357=VECTOR('',#22484,7.);
#6358=VECTOR('',#22487,7.);
#6359=VECTOR('',#22490,7.);
#6360=VECTOR('',#22493,7.);
#6361=VECTOR('',#22496,7.);
#6362=VECTOR('',#22499,7.);
#6363=VECTOR('',#22502,7.);
#6364=VECTOR('',#22505,7.);
#6365=VECTOR('',#22508,7.);
#6366=VECTOR('',#22511,7.);
#6367=VECTOR('',#22514,7.);
#6368=VECTOR('',#22517,7.);
#6369=VECTOR('',#22520,7.);
#6370=VECTOR('',#22523,7.);
#6371=VECTOR('',#22526,7.);
#6372=VECTOR('',#22529,7.);
#6373=VECTOR('',#22532,7.);
#6374=VECTOR('',#22535,7.);
#6375=VECTOR('',#22538,7.);
#6376=VECTOR('',#22541,7.);
#6377=VECTOR('',#22544,7.);
#6378=VECTOR('',#22547,7.);
#6379=VECTOR('',#22550,7.);
#6380=VECTOR('',#22553,7.);
#6381=VECTOR('',#22556,7.);
#6382=VECTOR('',#22559,7.);
#6383=VECTOR('',#22562,7.);
#6384=VECTOR('',#22565,7.);
#6385=VECTOR('',#22568,7.);
#6386=VECTOR('',#22571,7.);
#6387=VECTOR('',#22574,7.);
#6388=VECTOR('',#22577,7.);
#6389=VECTOR('',#22580,7.);
#6390=VECTOR('',#22583,7.);
#6391=VECTOR('',#22586,7.);
#6392=VECTOR('',#22589,7.);
#6393=VECTOR('',#22592,7.);
#6394=VECTOR('',#22595,7.);
#6395=VECTOR('',#22598,7.);
#6396=VECTOR('',#22601,7.);
#6397=VECTOR('',#22604,7.);
#6398=VECTOR('',#22607,7.);
#6399=VECTOR('',#22610,7.);
#6400=VECTOR('',#22613,7.);
#6401=VECTOR('',#22616,7.);
#6402=VECTOR('',#22619,7.);
#6403=VECTOR('',#22622,7.);
#6404=VECTOR('',#22629,7.);
#6405=VECTOR('',#22632,7.);
#6406=VECTOR('',#22635,7.);
#6407=VECTOR('',#22638,7.);
#6408=VECTOR('',#22641,7.);
#6409=VECTOR('',#22644,7.);
#6410=VECTOR('',#22647,7.);
#6411=VECTOR('',#22650,7.);
#6412=VECTOR('',#22653,7.);
#6413=VECTOR('',#22656,7.);
#6414=VECTOR('',#22659,7.);
#6415=VECTOR('',#22662,7.);
#6416=VECTOR('',#22665,7.);
#6417=VECTOR('',#22668,7.);
#6418=VECTOR('',#22671,7.);
#6419=VECTOR('',#22674,6.21925);
#6420=VECTOR('',#22679,6.21925);
#6421=VECTOR('',#22682,6.21925);
#6422=VECTOR('',#22685,6.21925);
#6423=VECTOR('',#22688,6.21925);
#6424=VECTOR('',#22691,6.21925);
#6425=VECTOR('',#22694,6.21925);
#6426=VECTOR('',#22697,6.21925);
#6427=VECTOR('',#22700,6.21925);
#6428=VECTOR('',#22703,6.21925);
#6429=VECTOR('',#22706,6.21925);
#6430=VECTOR('',#22709,6.21925);
#6431=VECTOR('',#22712,6.21925);
#6432=VECTOR('',#22715,6.21925);
#6433=VECTOR('',#22718,6.21925);
#6434=VECTOR('',#22721,6.21925);
#6435=VECTOR('',#22724,6.21925);
#6436=VECTOR('',#22729,6.21925);
#6437=VECTOR('',#22734,6.21925);
#6438=VECTOR('',#22737,6.21925);
#6439=VECTOR('',#22740,6.21925);
#6440=VECTOR('',#22743,6.21925);
#6441=VECTOR('',#22746,6.21925);
#6442=VECTOR('',#22749,6.21925);
#6443=VECTOR('',#22752,6.21925);
#6444=VECTOR('',#22755,6.21925);
#6445=VECTOR('',#22758,6.21925);
#6446=VECTOR('',#22761,6.21925);
#6447=VECTOR('',#22764,6.21925);
#6448=VECTOR('',#22767,6.21925);
#6449=VECTOR('',#22770,6.21925);
#6450=VECTOR('',#22773,6.21925);
#6451=VECTOR('',#22776,6.21925);
#6452=VECTOR('',#22779,6.21925);
#6453=VECTOR('',#22782,6.21925);
#6454=VECTOR('',#22785,6.21925);
#6455=VECTOR('',#22788,6.21925);
#6456=VECTOR('',#22791,6.21925);
#6457=VECTOR('',#22794,6.21925);
#6458=VECTOR('',#22797,6.21925);
#6459=VECTOR('',#22800,6.21925);
#6460=VECTOR('',#22803,6.21925);
#6461=VECTOR('',#22806,6.21925);
#6462=VECTOR('',#22809,6.21925);
#6463=VECTOR('',#22812,6.21925);
#6464=VECTOR('',#22815,6.21925);
#6465=VECTOR('',#22818,6.21925);
#6466=VECTOR('',#22821,6.21925);
#6467=VECTOR('',#22824,6.21925);
#6468=VECTOR('',#22827,6.21925);
#6469=VECTOR('',#22830,6.21925);
#6470=VECTOR('',#22833,6.21925);
#6471=VECTOR('',#22836,6.21925);
#6472=VECTOR('',#22839,6.21925);
#6473=VECTOR('',#22842,6.21925);
#6474=VECTOR('',#22845,6.21925);
#6475=VECTOR('',#22848,6.21925);
#6476=VECTOR('',#22851,6.21925);
#6477=VECTOR('',#22854,6.21925);
#6478=VECTOR('',#22857,6.21925);
#6479=VECTOR('',#22860,6.21925);
#6480=VECTOR('',#22863,6.21925);
#6481=VECTOR('',#22866,6.21925);
#6482=VECTOR('',#22869,6.21925);
#6483=VECTOR('',#22872,6.21925);
#6484=VECTOR('',#22875,6.21925);
#6485=VECTOR('',#22878,6.21925);
#6486=VECTOR('',#22881,6.21925);
#6487=VECTOR('',#22884,6.21925);
#6488=VECTOR('',#22887,6.21925);
#6489=VECTOR('',#22890,6.21925);
#6490=VECTOR('',#22893,6.21925);
#6491=VECTOR('',#22896,6.21925);
#6492=VECTOR('',#22899,6.21925);
#6493=VECTOR('',#22902,6.21925);
#6494=VECTOR('',#22905,6.21925);
#6495=VECTOR('',#22908,6.21925);
#6496=VECTOR('',#22911,6.21925);
#6497=VECTOR('',#22914,6.21925);
#6498=VECTOR('',#22917,10.);
#6499=VECTOR('',#22918,10.);
#6500=VECTOR('',#22921,10.);
#6501=VECTOR('',#22924,10.);
#6502=VECTOR('',#22961,10.);
#6503=VECTOR('',#22964,10.);
#6504=VECTOR('',#22997,10.);
#6505=VECTOR('',#23000,10.);
#6506=VECTOR('',#23027,10.);
#6507=VECTOR('',#23030,10.);
#6508=VECTOR('',#23057,10.);
#6509=VECTOR('',#23060,10.);
#6510=VECTOR('',#23087,10.);
#6511=VECTOR('',#23090,10.);
#6512=VECTOR('',#23117,10.);
#6513=VECTOR('',#23120,10.);
#6514=VECTOR('',#23147,10.);
#6515=VECTOR('',#23150,10.);
#6516=VECTOR('',#23179,10.);
#6517=VECTOR('',#23182,10.);
#6518=VECTOR('',#23211,10.);
#6519=VECTOR('',#23214,10.);
#6520=VECTOR('',#23241,10.);
#6521=VECTOR('',#23244,10.);
#6522=VECTOR('',#23271,10.);
#6523=VECTOR('',#23274,10.);
#6524=VECTOR('',#23301,10.);
#6525=VECTOR('',#23304,10.);
#6526=VECTOR('',#23331,10.);
#6527=VECTOR('',#23334,10.);
#6528=VECTOR('',#23361,10.);
#6529=VECTOR('',#23364,10.);
#6530=VECTOR('',#23385,10.);
#6531=VECTOR('',#23396,10.);
#6532=VECTOR('',#23415,6.5);
#6533=VECTOR('',#23418,8.5625);
#6534=VECTOR('',#23421,8.5625);
#6535=VECTOR('',#23430,6.5);
#6536=VECTOR('',#23439,10.);
#6537=VECTOR('',#23442,10.);
#6538=VECTOR('',#23455,10.);
#6539=VECTOR('',#23458,10.);
#6540=VECTOR('',#23463,10.);
#6541=VECTOR('',#23466,10.);
#6542=VECTOR('',#23485,10.);
#6543=VECTOR('',#23486,10.);
#6544=VECTOR('',#23491,10.);
#6545=VECTOR('',#23494,10.);
#6546=VECTOR('',#23501,10.);
#6547=VECTOR('',#23504,10.);
#6548=VECTOR('',#23507,10.);
#6549=VECTOR('',#23510,10.);
#6550=VECTOR('',#23515,10.);
#6551=VECTOR('',#23516,10.);
#6552=VECTOR('',#23519,10.);
#6553=VECTOR('',#23524,10.);
#6554=VECTOR('',#23527,10.);
#6555=VECTOR('',#23528,10.);
#6556=VECTOR('',#23531,10.);
#6557=VECTOR('',#23540,10.);
#6558=VECTOR('',#23547,10.);
#6559=VECTOR('',#23554,10.);
#6560=VECTOR('',#23557,10.);
#6561=VECTOR('',#23564,10.);
#6562=VECTOR('',#23567,10.);
#6563=VECTOR('',#23572,10.);
#6564=VECTOR('',#23581,10.);
#6565=VECTOR('',#23584,10.);
#6566=VECTOR('',#23587,10.);
#6567=VECTOR('',#23588,10.);
#6568=VECTOR('',#23589,10.);
#6569=VECTOR('',#23602,10.);
#6570=VECTOR('',#23605,10.);
#6571=VECTOR('',#23610,10.);
#6572=VECTOR('',#23613,10.);
#6573=VECTOR('',#23616,10.);
#6574=VECTOR('',#23619,10.);
#6575=VECTOR('',#23624,10.);
#6576=VECTOR('',#23625,10.);
#6577=VECTOR('',#23632,10.);
#6578=VECTOR('',#23633,10.);
#6579=VECTOR('',#23636,10.);
#6580=VECTOR('',#23641,10.);
#6581=VECTOR('',#23646,10.);
#6582=VECTOR('',#23649,10.);
#6583=VECTOR('',#23652,10.);
#6584=VECTOR('',#23653,10.);
#6585=VECTOR('',#23654,10.);
#6586=VECTOR('',#23655,10.);
#6587=VECTOR('',#23666,10.);
#6588=VECTOR('',#23675,10.);
#6589=VECTOR('',#23678,10.);
#6590=VECTOR('',#23679,10.);
#6591=VECTOR('',#23686,10.);
#6592=VECTOR('',#23701,10.);
#6593=VECTOR('',#23704,10.);
#6594=VECTOR('',#23709,10.);
#6595=VECTOR('',#23712,10.);
#6596=VECTOR('',#23723,10.);
#6597=VECTOR('',#23724,10.);
#6598=VECTOR('',#23725,10.);
#6599=VECTOR('',#23728,10.);
#6600=VECTOR('',#23729,10.);
#6601=VECTOR('',#23730,10.);
#6602=VECTOR('',#23737,10.);
#6603=VECTOR('',#23746,10.);
#6604=VECTOR('',#23755,10.);
#6605=VECTOR('',#23764,10.);
#6606=VECTOR('',#23769,10.);
#6607=VECTOR('',#23770,10.);
#6608=VECTOR('',#23773,10.);
#6609=VECTOR('',#23778,10.);
#6610=VECTOR('',#23779,10.);
#6611=VECTOR('',#23782,10.);
#6612=VECTOR('',#23787,10.);
#6613=VECTOR('',#23788,10.);
#6614=VECTOR('',#23791,10.);
#6615=VECTOR('',#23798,10.);
#6616=VECTOR('',#23801,10.);
#6617=VECTOR('',#23804,10.);
#6618=VECTOR('',#23807,10.);
#6619=VECTOR('',#23816,10.);
#6620=VECTOR('',#23817,10.);
#6621=VECTOR('',#23818,10.);
#6622=VECTOR('',#23821,10.);
#6623=VECTOR('',#23826,10.);
#6624=VECTOR('',#23827,10.);
#6625=VECTOR('',#23836,10.);
#6626=VECTOR('',#23837,10.);
#6627=VECTOR('',#23842,10.);
#6628=VECTOR('',#23845,10.);
#6629=VECTOR('',#23854,10.);
#6630=VECTOR('',#23861,10.);
#6631=VECTOR('',#23870,10.);
#6632=VECTOR('',#23875,10.);
#6633=VECTOR('',#23878,10.);
#6634=VECTOR('',#23879,10.);
#6635=VECTOR('',#23886,10.);
#6636=VECTOR('',#23893,10.);
#6637=VECTOR('',#23898,10.);
#6638=VECTOR('',#23899,10.);
#6639=VECTOR('',#23910,10.);
#6640=VECTOR('',#23913,10.);
#6641=VECTOR('',#23920,10.);
#6642=VECTOR('',#23923,10.);
#6643=VECTOR('',#23932,10.);
#6644=VECTOR('',#23933,10.);
#6645=VECTOR('',#23934,10.);
#6646=VECTOR('',#23937,10.);
#6647=VECTOR('',#23944,10.);
#6648=VECTOR('',#23945,0.5);
#6649=VECTOR('',#23950,10.);
#6650=VECTOR('',#23957,10.);
#6651=VECTOR('',#23960,10.);
#6652=VECTOR('',#23965,10.);
#6653=VECTOR('',#23968,10.);
#6654=VECTOR('',#23987,10.);
#6655=VECTOR('',#23990,10.);
#6656=VECTOR('',#23993,10.);
#6657=VECTOR('',#23996,10.);
#6658=VECTOR('',#23999,10.);
#6659=VECTOR('',#24002,10.);
#6660=VECTOR('',#24005,10.);
#6661=VECTOR('',#24006,10.);
#6662=VECTOR('',#24009,10.);
#6663=VECTOR('',#24016,10.);
#6664=VECTOR('',#24019,10.);
#6665=VECTOR('',#24034,0.5);
#6666=VECTOR('',#24035,0.5);
#6667=VECTOR('',#24040,10.);
#6668=VECTOR('',#24045,10.);
#6669=VECTOR('',#24046,10.);
#6670=VECTOR('',#24049,10.);
#6671=VECTOR('',#24054,10.);
#6672=VECTOR('',#24055,10.);
#6673=VECTOR('',#24064,10.);
#6674=VECTOR('',#24065,10.);
#6675=VECTOR('',#24070,10.);
#6676=VECTOR('',#24073,10.);
#6677=VECTOR('',#24076,10.);
#6678=VECTOR('',#24081,10.);
#6679=VECTOR('',#24084,10.);
#6680=VECTOR('',#24091,10.);
#6681=VECTOR('',#24098,10.);
#6682=VECTOR('',#24101,10.);
#6683=VECTOR('',#24102,10.);
#6684=VECTOR('',#24109,10.);
#6685=VECTOR('',#24112,10.);
#6686=VECTOR('',#24115,10.);
#6687=VECTOR('',#24116,10.);
#6688=VECTOR('',#24117,10.);
#6689=VECTOR('',#24130,10.);
#6690=VECTOR('',#24137,10.);
#6691=VECTOR('',#24150,10.);
#6692=VECTOR('',#24161,10.);
#6693=VECTOR('',#24178,44.);
#6694=VECTOR('',#24181,10.);
#6695=VECTOR('',#24184,10.);
#6696=VECTOR('',#24187,10.);
#6697=VECTOR('',#24190,10.);
#6698=VECTOR('',#24193,10.);
#6699=VECTOR('',#24196,10.);
#6700=VECTOR('',#24199,10.);
#6701=VECTOR('',#24202,10.);
#6702=VECTOR('',#24211,10.);
#6703=VECTOR('',#24214,10.);
#6704=VECTOR('',#24227,10.);
#6705=VECTOR('',#24228,10.);
#6706=VECTOR('',#24251,10.);
#6707=VECTOR('',#24254,10.);
#6708=VECTOR('',#24257,10.);
#6709=VECTOR('',#24260,10.);
#6710=VECTOR('',#24263,10.);
#6711=VECTOR('',#24266,10.);
#6712=VECTOR('',#24287,10.);
#6713=VECTOR('',#24292,10.);
#6714=VECTOR('',#24303,10.);
#6715=VECTOR('',#24318,10.);
#6716=VECTOR('',#24319,10.);
#6717=VECTOR('',#24320,10.);
#6718=VECTOR('',#24327,10.);
#6719=VECTOR('',#24344,10.);
#6720=VECTOR('',#24355,10.);
#6721=VECTOR('',#24356,10.);
#6722=VECTOR('',#24357,10.);
#6723=VECTOR('',#24368,10.);
#6724=VECTOR('',#24369,10.);
#6725=VECTOR('',#24376,10.);
#6726=VECTOR('',#24377,10.);
#6727=VECTOR('',#24392,10.);
#6728=VECTOR('',#24397,10.);
#6729=VECTOR('',#24398,10.);
#6730=VECTOR('',#24399,10.);
#6731=VECTOR('',#24406,10.);
#6732=VECTOR('',#24437,10.);
#6733=VECTOR('',#24440,10.);
#6734=VECTOR('',#24453,10.);
#6735=VECTOR('',#24462,10.);
#6736=VECTOR('',#24473,10.);
#6737=VECTOR('',#24480,10.);
#6738=VECTOR('',#24483,10.);
#6739=VECTOR('',#24484,10.);
#6740=VECTOR('',#24485,10.);
#6741=VECTOR('',#24506,1.25);
#6742=VECTOR('',#24523,10.);
#6743=VECTOR('',#24524,10.);
#6744=VECTOR('',#24527,10.);
#6745=VECTOR('',#24528,10.);
#6746=VECTOR('',#24529,10.);
#6747=VECTOR('',#24530,10.);
#6748=VECTOR('',#24531,10.);
#6749=VECTOR('',#24534,10.);
#6750=VECTOR('',#24541,10.);
#6751=VECTOR('',#24546,10.);
#6752=VECTOR('',#24551,0.5);
#6753=VECTOR('',#24554,0.5);
#6754=VECTOR('',#24559,0.5);
#6755=VECTOR('',#24560,10.);
#6756=VECTOR('',#24565,0.5);
#6757=VECTOR('',#24576,10.);
#6758=VECTOR('',#24577,10.);
#6759=VECTOR('',#24578,10.);
#6760=VECTOR('',#24581,10.);
#6761=VECTOR('',#24584,10.);
#6762=VECTOR('',#24587,10.);
#6763=VECTOR('',#24608,1.25);
#6764=VECTOR('',#24619,10.);
#6765=VECTOR('',#24628,10.);
#6766=VECTOR('',#24635,10.);
#6767=VECTOR('',#24648,10.);
#6768=VECTOR('',#24651,10.);
#6769=VECTOR('',#24654,10.);
#6770=VECTOR('',#24659,10.);
#6771=VECTOR('',#24662,10.);
#6772=VECTOR('',#24671,10.);
#6773=VECTOR('',#24674,10.);
#6774=VECTOR('',#24679,10.);
#6775=VECTOR('',#24680,0.5);
#6776=VECTOR('',#24695,44.);
#6777=VECTOR('',#24714,43.6);
#6778=VECTOR('',#24743,10.);
#6779=VECTOR('',#24746,10.);
#6780=VECTOR('',#24747,10.);
#6781=VECTOR('',#24750,10.);
#6782=VECTOR('',#24759,10.);
#6783=VECTOR('',#24760,10.);
#6784=VECTOR('',#24761,10.);
#6785=VECTOR('',#24762,10.);
#6786=VECTOR('',#24775,1.25);
#6787=VECTOR('',#24788,1.25);
#6788=VECTOR('',#24831,3.);
#6789=VECTOR('',#24844,3.);
#6790=VECTOR('',#24869,3.);
#6791=VECTOR('',#24890,3.);
#6792=VECTOR('',#24907,3.);
#6793=VECTOR('',#24924,3.);
#6794=VECTOR('',#24931,10.);
#6795=VECTOR('',#24934,10.);
#6796=VECTOR('',#24939,10.);
#6797=VECTOR('',#24946,10.);
#6798=VECTOR('',#24947,10.);
#6799=VECTOR('',#24948,10.);
#6800=VECTOR('',#24967,43.7);
#6801=VECTOR('',#24976,44.);
#6802=VECTOR('',#25023,7.05);
#6803=VECTOR('',#25038,7.3);
#6804=VECTOR('',#25059,12.);
#6805=VECTOR('',#25074,43.7);
#6806=VECTOR('',#25107,10.);
#6807=VECTOR('',#25108,10.);
#6808=VECTOR('',#25117,5.);
#6809=VECTOR('',#25128,5.);
#6810=VECTOR('',#25139,5.);
#6811=VECTOR('',#25150,12.25);
#6812=VECTOR('',#25161,10.);
#6813=VECTOR('',#25176,10.);
#6814=VECTOR('',#25191,42.4);
#6815=VECTOR('',#25194,4.5);
#6816=VECTOR('',#25197,4.5);
#6817=VECTOR('',#25200,4.5);
#6818=VECTOR('',#25209,3.18);
#6819=VECTOR('',#25214,3.03);
#6820=VECTOR('',#25281,3.18);
#6821=VECTOR('',#25384,10.);
#6822=VECTOR('',#25389,10.);
#6823=VECTOR('',#25398,10.);
#6824=VECTOR('',#25403,10.);
#6825=VECTOR('',#25562,10.);
#6826=VECTOR('',#25565,10.);
#6827=VECTOR('',#25572,10.);
#6828=VECTOR('',#25575,10.);
#6829=VECTOR('',#25582,10.);
#6830=VECTOR('',#25585,10.);
#6831=VECTOR('',#25592,10.);
#6832=VECTOR('',#25595,10.);
#6833=VECTOR('',#25602,10.);
#6834=VECTOR('',#25605,10.);
#6835=VECTOR('',#25612,10.);
#6836=VECTOR('',#25615,10.);
#6837=VECTOR('',#25622,10.);
#6838=VECTOR('',#25625,10.);
#6839=VECTOR('',#25632,10.);
#6840=VECTOR('',#25635,10.);
#6841=VECTOR('',#25642,10.);
#6842=VECTOR('',#25645,10.);
#6843=VECTOR('',#25652,10.);
#6844=VECTOR('',#25655,10.);
#6845=VECTOR('',#25662,10.);
#6846=VECTOR('',#25665,10.);
#6847=VECTOR('',#25672,10.);
#6848=VECTOR('',#25675,10.);
#6849=VECTOR('',#25676,10.);
#6850=VECTOR('',#25679,10.);
#6851=VECTOR('',#25690,10.);
#6852=VECTOR('',#25693,10.);
#6853=VECTOR('',#25704,10.);
#6854=VECTOR('',#25707,10.);
#6855=VECTOR('',#25718,10.);
#6856=VECTOR('',#25721,10.);
#6857=VECTOR('',#25732,10.);
#6858=VECTOR('',#25735,10.);
#6859=VECTOR('',#25746,10.);
#6860=VECTOR('',#25749,10.);
#6861=VECTOR('',#25760,10.);
#6862=VECTOR('',#25763,10.);
#6863=VECTOR('',#25774,10.);
#6864=VECTOR('',#25777,10.);
#6865=VECTOR('',#25788,10.);
#6866=VECTOR('',#25791,10.);
#6867=VECTOR('',#25802,10.);
#6868=VECTOR('',#25805,10.);
#6869=VECTOR('',#25816,10.);
#6870=VECTOR('',#25819,10.);
#6871=VECTOR('',#25830,10.);
#6872=VECTOR('',#25833,10.);
#6873=VECTOR('',#25844,10.);
#6874=VECTOR('',#25847,10.);
#6875=VECTOR('',#25858,10.);
#6876=VECTOR('',#25861,10.);
#6877=VECTOR('',#25872,10.);
#6878=VECTOR('',#25875,10.);
#6879=VECTOR('',#25886,10.);
#6880=VECTOR('',#25889,10.);
#6881=VECTOR('',#25900,10.);
#6882=VECTOR('',#25903,10.);
#6883=VECTOR('',#25914,10.);
#6884=VECTOR('',#25917,10.);
#6885=VECTOR('',#25928,10.);
#6886=VECTOR('',#25931,10.);
#6887=VECTOR('',#25942,10.);
#6888=VECTOR('',#25945,10.);
#6889=VECTOR('',#25956,10.);
#6890=VECTOR('',#25959,10.);
#6891=VECTOR('',#25970,10.);
#6892=VECTOR('',#25973,10.);
#6893=VECTOR('',#25984,10.);
#6894=VECTOR('',#25987,10.);
#6895=VECTOR('',#25998,10.);
#6896=VECTOR('',#26001,10.);
#6897=VECTOR('',#26012,10.);
#6898=VECTOR('',#26015,10.);
#6899=VECTOR('',#26046,2.8);
#6900=VECTOR('',#26063,3.);
#6901=VECTOR('',#26078,2.8);
#6902=VECTOR('',#26097,10.);
#6903=VECTOR('',#26100,10.);
#6904=VECTOR('',#26113,10.);
#6905=VECTOR('',#26114,10.);
#6906=VECTOR('',#26123,10.);
#6907=VECTOR('',#26126,10.);
#6908=VECTOR('',#26129,10.);
#6909=VECTOR('',#26130,10.);
#6910=VECTOR('',#26141,10.);
#6911=VECTOR('',#26154,10.);
#6912=VECTOR('',#26155,10.);
#6913=VECTOR('',#26162,10.);
#6914=VECTOR('',#26175,1.275);
#6915=VECTOR('',#26200,1.1);
#6916=VECTOR('',#26217,1.25);
#6917=VECTOR('',#26232,1.1);
#6918=VECTOR('',#26263,10.);
#6919=VECTOR('',#26266,10.);
#6920=VECTOR('',#26269,10.);
#6921=VECTOR('',#26272,10.);
#6922=VECTOR('',#26275,10.);
#6923=VECTOR('',#26288,10.);
#6924=VECTOR('',#26289,10.);
#6925=VECTOR('',#26294,10.);
#6926=VECTOR('',#26295,10.);
#6927=VECTOR('',#26312,10.);
#6928=VECTOR('',#26313,10.);
#6929=VECTOR('',#26320,10.);
#6930=VECTOR('',#26323,10.);
#6931=VECTOR('',#26328,10.);
#6932=VECTOR('',#26329,10.);
#6933=VECTOR('',#26332,10.);
#6934=VECTOR('',#26337,10.);
#6935=VECTOR('',#26340,10.);
#6936=VECTOR('',#26349,10.);
#6937=VECTOR('',#26352,10.);
#6938=VECTOR('',#26353,10.);
#6939=VECTOR('',#26360,10.);
#6940=VECTOR('',#26363,10.);
#6941=VECTOR('',#26366,10.);
#6942=VECTOR('',#26369,10.);
#6943=VECTOR('',#26374,10.);
#6944=VECTOR('',#26377,10.);
#6945=VECTOR('',#26386,10.);
#6946=VECTOR('',#26389,10.);
#6947=VECTOR('',#26394,10.);
#6948=VECTOR('',#26397,10.);
#6949=VECTOR('',#26408,10.);
#6950=VECTOR('',#26411,10.);
#6951=VECTOR('',#26416,10.);
#6952=VECTOR('',#26417,10.);
#6953=VECTOR('',#26420,10.);
#6954=VECTOR('',#26433,10.);
#6955=VECTOR('',#26434,10.);
#6956=VECTOR('',#26443,10.);
#6957=VECTOR('',#26446,10.);
#6958=VECTOR('',#26447,10.);
#6959=VECTOR('',#26450,10.);
#6960=VECTOR('',#26451,10.);
#6961=VECTOR('',#26460,10.);
#6962=VECTOR('',#26465,10.);
#6963=VECTOR('',#26468,10.);
#6964=VECTOR('',#26483,10.);
#6965=VECTOR('',#26486,10.);
#6966=VECTOR('',#26489,10.);
#6967=VECTOR('',#26492,10.);
#6968=VECTOR('',#26495,10.);
#6969=VECTOR('',#26496,10.);
#6970=VECTOR('',#26499,10.);
#6971=VECTOR('',#26502,10.);
#6972=VECTOR('',#26505,10.);
#6973=VECTOR('',#26510,10.);
#6974=VECTOR('',#26513,10.);
#6975=VECTOR('',#26518,10.);
#6976=VECTOR('',#26521,10.);
#6977=VECTOR('',#26522,10.);
#6978=VECTOR('',#26531,10.);
#6979=VECTOR('',#26534,10.);
#6980=VECTOR('',#26541,10.);
#6981=VECTOR('',#26544,10.);
#6982=VECTOR('',#26547,10.);
#6983=VECTOR('',#26548,10.);
#6984=VECTOR('',#26553,10.);
#6985=VECTOR('',#26578,10.);
#6986=VECTOR('',#26581,10.);
#6987=VECTOR('',#26584,10.);
#6988=VECTOR('',#26585,10.);
#6989=VECTOR('',#26586,10.);
#6990=VECTOR('',#26587,10.);
#6991=VECTOR('',#26588,10.);
#6992=VECTOR('',#26589,10.);
#6993=VECTOR('',#26594,21.55);
#6994=VECTOR('',#26611,23.);
#6995=VECTOR('',#26630,10.);
#6996=VECTOR('',#26643,10.);
#6997=VECTOR('',#26646,10.);
#6998=VECTOR('',#26651,10.);
#6999=VECTOR('',#26654,10.);
#7000=VECTOR('',#26659,10.);
#7001=VECTOR('',#26662,10.);
#7002=VECTOR('',#26679,10.);
#7003=VECTOR('',#26680,10.);
#7004=VECTOR('',#26683,10.);
#7005=VECTOR('',#26688,10.);
#7006=VECTOR('',#26689,10.);
#7007=VECTOR('',#26692,10.);
#7008=VECTOR('',#26697,10.);
#7009=VECTOR('',#26698,10.);
#7010=VECTOR('',#26709,22.7);
#7011=VECTOR('',#26724,21.8);
#7012=VECTOR('',#26745,10.);
#7013=VECTOR('',#26754,10.);
#7014=VECTOR('',#26757,10.);
#7015=VECTOR('',#26760,10.);
#7016=VECTOR('',#26761,10.);
#7017=VECTOR('',#26768,10.);
#7018=VECTOR('',#26775,10.);
#7019=VECTOR('',#26786,10.);
#7020=VECTOR('',#26799,7.05);
#7021=VECTOR('',#26814,10.4);
#7022=VECTOR('',#26831,10.);
#7023=VECTOR('',#26832,10.);
#7024=VECTOR('',#26833,10.);
#7025=VECTOR('',#26836,10.);
#7026=VECTOR('',#26837,10.);
#7027=VECTOR('',#26838,10.);
#7028=VECTOR('',#26841,10.);
#7029=VECTOR('',#26842,10.);
#7030=VECTOR('',#26843,10.);
#7031=VECTOR('',#26846,10.);
#7032=VECTOR('',#26847,10.);
#7033=VECTOR('',#26848,10.);
#7034=VECTOR('',#26851,10.);
#7035=VECTOR('',#26852,10.);
#7036=VECTOR('',#26855,10.);
#7037=VECTOR('',#26856,10.);
#7038=VECTOR('',#26857,10.);
#7039=VECTOR('',#26860,10.);
#7040=VECTOR('',#26861,10.);
#7041=VECTOR('',#26862,10.);
#7042=VECTOR('',#26865,10.);
#7043=VECTOR('',#26866,10.);
#7044=VECTOR('',#26869,10.);
#7045=VECTOR('',#26870,10.);
#7046=VECTOR('',#26871,10.);
#7047=VECTOR('',#26874,10.);
#7048=VECTOR('',#26875,10.);
#7049=VECTOR('',#26878,10.);
#7050=VECTOR('',#26879,10.);
#7051=VECTOR('',#26882,10.);
#7052=VECTOR('',#26883,10.);
#7053=VECTOR('',#26884,10.);
#7054=VECTOR('',#26887,10.);
#7055=VECTOR('',#26888,10.);
#7056=VECTOR('',#26891,10.);
#7057=VECTOR('',#26892,10.);
#7058=VECTOR('',#26895,10.);
#7059=VECTOR('',#26896,10.);
#7060=VECTOR('',#26899,10.);
#7061=VECTOR('',#26900,10.);
#7062=VECTOR('',#26903,10.);
#7063=VECTOR('',#26904,10.);
#7064=VECTOR('',#26907,10.);
#7065=VECTOR('',#26908,10.);
#7066=VECTOR('',#26911,10.);
#7067=VECTOR('',#26912,10.);
#7068=VECTOR('',#26915,10.);
#7069=VECTOR('',#26916,10.);
#7070=VECTOR('',#26957,9.);
#7071=VECTOR('',#26960,10.);
#7072=VECTOR('',#26967,10.);
#7073=VECTOR('',#26968,10.);
#7074=VECTOR('',#26969,10.);
#7075=VECTOR('',#26978,10.);
#7076=VECTOR('',#26979,10.);
#7077=VECTOR('',#26980,10.);
#7078=VECTOR('',#26987,10.);
#7079=VECTOR('',#26988,10.);
#7080=VECTOR('',#26989,10.);
#7081=VECTOR('',#26996,10.);
#7082=VECTOR('',#26997,10.);
#7083=VECTOR('',#27006,10.);
#7084=VECTOR('',#27009,10.);
#7085=VECTOR('',#27010,10.);
#7086=VECTOR('',#27011,10.);
#7087=VECTOR('',#27014,10.);
#7088=VECTOR('',#27015,10.);
#7089=VECTOR('',#27016,10.);
#7090=VECTOR('',#27021,10.);
#7091=VECTOR('',#27022,10.);
#7092=VECTOR('',#27023,10.);
#7093=VECTOR('',#27028,10.);
#7094=VECTOR('',#27029,10.);
#7095=VECTOR('',#27034,10.);
#7096=VECTOR('',#27039,10.);
#7097=VECTOR('',#27040,10.);
#7098=VECTOR('',#27041,10.);
#7099=VECTOR('',#27052,10.);
#7100=VECTOR('',#27057,10.);
#7101=VECTOR('',#27058,10.);
#7102=VECTOR('',#27059,10.);
#7103=VECTOR('',#27070,10.);
#7104=VECTOR('',#27075,10.);
#7105=VECTOR('',#27076,10.);
#7106=VECTOR('',#27077,10.);
#7107=VECTOR('',#27104,10.);
#7108=VECTOR('',#27107,10.);
#7109=VECTOR('',#27120,10.);
#7110=VECTOR('',#27123,10.);
#7111=VECTOR('',#27134,10.);
#7112=VECTOR('',#27135,10.);
#7113=VECTOR('',#27136,10.);
#7114=VECTOR('',#27139,10.);
#7115=VECTOR('',#27162,21.);
#7116=VECTOR('',#27165,10.);
#7117=VECTOR('',#27168,10.);
#7118=VECTOR('',#27171,10.);
#7119=VECTOR('',#27174,10.);
#7120=VECTOR('',#27177,10.);
#7121=VECTOR('',#27180,10.);
#7122=VECTOR('',#27183,10.);
#7123=VECTOR('',#27192,10.);
#7124=VECTOR('',#27233,10.);
#7125=VECTOR('',#27236,10.);
#7126=VECTOR('',#27277,10.);
#7127=VECTOR('',#27280,10.);
#7128=VECTOR('',#27283,10.);
#7129=VECTOR('',#27284,10.);
#7130=VECTOR('',#27287,10.);
#7131=VECTOR('',#27298,10.);
#7132=VECTOR('',#27313,10.);
#7133=VECTOR('',#27314,10.);
#7134=VECTOR('',#27317,10.);
#7135=VECTOR('',#27318,10.);
#7136=VECTOR('',#27335,10.);
#7137=VECTOR('',#27346,10.);
#7138=VECTOR('',#27347,10.);
#7139=VECTOR('',#27348,10.);
#7140=VECTOR('',#27351,10.);
#7141=VECTOR('',#27356,10.);
#7142=VECTOR('',#27361,10.);
#7143=VECTOR('',#27378,10.);
#7144=VECTOR('',#27381,10.);
#7145=VECTOR('',#27394,10.);
#7146=VECTOR('',#27395,10.);
#7147=VECTOR('',#27406,10.);
#7148=VECTOR('',#27409,10.);
#7149=VECTOR('',#27410,10.);
#7150=VECTOR('',#27413,10.);
#7151=VECTOR('',#27414,10.);
#7152=VECTOR('',#27417,10.);
#7153=VECTOR('',#27418,18.5);
#7154=VECTOR('',#27421,10.);
#7155=VECTOR('',#27426,10.);
#7156=VECTOR('',#27429,10.);
#7157=VECTOR('',#27430,10.);
#7158=VECTOR('',#27433,10.);
#7159=VECTOR('',#27436,10.);
#7160=VECTOR('',#27439,10.);
#7161=VECTOR('',#27440,10.);
#7162=VECTOR('',#27445,10.);
#7163=VECTOR('',#27452,10.);
#7164=VECTOR('',#27453,10.);
#7165=VECTOR('',#27454,10.);
#7166=VECTOR('',#27457,10.);
#7167=VECTOR('',#27464,10.);
#7168=VECTOR('',#27465,10.);
#7169=VECTOR('',#27466,10.);
#7170=VECTOR('',#27483,10.);
#7171=VECTOR('',#27496,10.);
#7172=VECTOR('',#27499,10.);
#7173=VECTOR('',#27502,10.);
#7174=VECTOR('',#27509,10.);
#7175=VECTOR('',#27520,10.);
#7176=VECTOR('',#27525,10.);
#7177=VECTOR('',#27546,10.);
#7178=VECTOR('',#27555,10.);
#7179=VECTOR('',#27558,10.);
#7180=VECTOR('',#27563,10.);
#7181=VECTOR('',#27566,10.);
#7182=VECTOR('',#27567,10.);
#7183=VECTOR('',#27568,10.);
#7184=VECTOR('',#27569,10.);
#7185=VECTOR('',#27576,10.);
#7186=VECTOR('',#27577,10.);
#7187=VECTOR('',#27590,20.6);
#7188=VECTOR('',#27599,10.);
#7189=VECTOR('',#27602,10.);
#7190=VECTOR('',#27603,10.);
#7191=VECTOR('',#27604,10.);
#7192=VECTOR('',#27607,10.);
#7193=VECTOR('',#27610,10.);
#7194=VECTOR('',#27611,10.);
#7195=VECTOR('',#27612,10.);
#7196=VECTOR('',#27615,10.);
#7197=VECTOR('',#27618,10.);
#7198=VECTOR('',#27619,10.);
#7199=VECTOR('',#27620,10.);
#7200=VECTOR('',#27623,10.);
#7201=VECTOR('',#27626,10.);
#7202=VECTOR('',#27643,10.);
#7203=VECTOR('',#27644,10.);
#7204=VECTOR('',#27653,10.);
#7205=VECTOR('',#27660,10.);
#7206=VECTOR('',#27683,10.);
#7207=VECTOR('',#27686,10.);
#7208=VECTOR('',#27689,10.);
#7209=VECTOR('',#27702,10.);
#7210=VECTOR('',#27711,10.);
#7211=VECTOR('',#27712,10.);
#7212=VECTOR('',#27715,10.);
#7213=VECTOR('',#27718,10.);
#7214=VECTOR('',#27719,10.);
#7215=VECTOR('',#27720,10.);
#7216=VECTOR('',#27723,10.);
#7217=VECTOR('',#27730,10.);
#7218=VECTOR('',#27735,10.);
#7219=VECTOR('',#27738,10.);
#7220=VECTOR('',#27739,10.);
#7221=VECTOR('',#27740,10.);
#7222=VECTOR('',#27743,10.);
#7223=VECTOR('',#27746,10.);
#7224=VECTOR('',#27749,10.);
#7225=VECTOR('',#27766,10.);
#7226=VERTEX_POINT('',#27822);
#7227=VERTEX_POINT('',#27823);
#7228=VERTEX_POINT('',#27825);
#7229=VERTEX_POINT('',#27851);
#7230=VERTEX_POINT('',#27853);
#7231=VERTEX_POINT('',#27855);
#7232=VERTEX_POINT('',#27857);
#7233=VERTEX_POINT('',#27859);
#7234=VERTEX_POINT('',#27861);
#7235=VERTEX_POINT('',#27864);
#7236=VERTEX_POINT('',#27866);
#7237=VERTEX_POINT('',#27869);
#7238=VERTEX_POINT('',#27893);
#7239=VERTEX_POINT('',#27894);
#7240=VERTEX_POINT('',#27896);
#7241=VERTEX_POINT('',#27898);
#7242=VERTEX_POINT('',#27902);
#7243=VERTEX_POINT('',#27903);
#7244=VERTEX_POINT('',#27962);
#7245=VERTEX_POINT('',#27963);
#7246=VERTEX_POINT('',#28022);
#7247=VERTEX_POINT('',#28023);
#7248=VERTEX_POINT('',#28079);
#7249=VERTEX_POINT('',#28080);
#7250=VERTEX_POINT('',#28139);
#7251=VERTEX_POINT('',#28140);
#7252=VERTEX_POINT('',#28199);
#7253=VERTEX_POINT('',#28200);
#7254=VERTEX_POINT('',#28259);
#7255=VERTEX_POINT('',#28260);
#7256=VERTEX_POINT('',#28316);
#7257=VERTEX_POINT('',#28317);
#7258=VERTEX_POINT('',#28373);
#7259=VERTEX_POINT('',#28374);
#7260=VERTEX_POINT('',#28436);
#7261=VERTEX_POINT('',#28437);
#7262=VERTEX_POINT('',#28490);
#7263=VERTEX_POINT('',#28491);
#7264=VERTEX_POINT('',#28550);
#7265=VERTEX_POINT('',#28551);
#7266=VERTEX_POINT('',#28610);
#7267=VERTEX_POINT('',#28611);
#7268=VERTEX_POINT('',#28667);
#7269=VERTEX_POINT('',#28668);
#7270=VERTEX_POINT('',#28724);
#7271=VERTEX_POINT('',#28725);
#7272=VERTEX_POINT('',#28790);
#7273=VERTEX_POINT('',#28791);
#7274=VERTEX_POINT('',#28850);
#7275=VERTEX_POINT('',#28851);
#7276=VERTEX_POINT('',#28907);
#7277=VERTEX_POINT('',#28908);
#7278=VERTEX_POINT('',#28964);
#7279=VERTEX_POINT('',#28965);
#7280=VERTEX_POINT('',#29027);
#7281=VERTEX_POINT('',#29028);
#7282=VERTEX_POINT('',#29081);
#7283=VERTEX_POINT('',#29082);
#7284=VERTEX_POINT('',#29138);
#7285=VERTEX_POINT('',#29139);
#7286=VERTEX_POINT('',#29198);
#7287=VERTEX_POINT('',#29199);
#7288=VERTEX_POINT('',#29255);
#7289=VERTEX_POINT('',#29256);
#7290=VERTEX_POINT('',#29312);
#7291=VERTEX_POINT('',#29313);
#7292=VERTEX_POINT('',#29378);
#7293=VERTEX_POINT('',#29379);
#7294=VERTEX_POINT('',#29438);
#7295=VERTEX_POINT('',#29439);
#7296=VERTEX_POINT('',#29495);
#7297=VERTEX_POINT('',#29496);
#7298=VERTEX_POINT('',#29552);
#7299=VERTEX_POINT('',#29553);
#7300=VERTEX_POINT('',#29612);
#7301=VERTEX_POINT('',#29613);
#7302=VERTEX_POINT('',#29666);
#7303=VERTEX_POINT('',#29667);
#7304=VERTEX_POINT('',#29723);
#7305=VERTEX_POINT('',#29724);
#7306=VERTEX_POINT('',#29786);
#7307=VERTEX_POINT('',#29787);
#7308=VERTEX_POINT('',#29846);
#7309=VERTEX_POINT('',#29847);
#7310=VERTEX_POINT('',#29900);
#7311=VERTEX_POINT('',#29901);
#7312=VERTEX_POINT('',#29960);
#7313=VERTEX_POINT('',#29961);
#7314=VERTEX_POINT('',#30020);
#7315=VERTEX_POINT('',#30021);
#7316=VERTEX_POINT('',#30077);
#7317=VERTEX_POINT('',#30078);
#7318=VERTEX_POINT('',#30137);
#7319=VERTEX_POINT('',#30138);
#7320=VERTEX_POINT('',#30197);
#7321=VERTEX_POINT('',#30198);
#7322=VERTEX_POINT('',#30254);
#7323=VERTEX_POINT('',#30255);
#7324=VERTEX_POINT('',#30314);
#7325=VERTEX_POINT('',#30315);
#7326=VERTEX_POINT('',#30374);
#7327=VERTEX_POINT('',#30375);
#7328=VERTEX_POINT('',#30434);
#7329=VERTEX_POINT('',#30435);
#7330=VERTEX_POINT('',#30488);
#7331=VERTEX_POINT('',#30489);
#7332=VERTEX_POINT('',#30545);
#7333=VERTEX_POINT('',#30546);
#7334=VERTEX_POINT('',#30608);
#7335=VERTEX_POINT('',#30609);
#7336=VERTEX_POINT('',#30665);
#7337=VERTEX_POINT('',#30666);
#7338=VERTEX_POINT('',#30725);
#7339=VERTEX_POINT('',#30726);
#7340=VERTEX_POINT('',#30785);
#7341=VERTEX_POINT('',#30786);
#7342=VERTEX_POINT('',#30842);
#7343=VERTEX_POINT('',#30843);
#7344=VERTEX_POINT('',#30902);
#7345=VERTEX_POINT('',#30903);
#7346=VERTEX_POINT('',#30965);
#7347=VERTEX_POINT('',#30966);
#7348=VERTEX_POINT('',#31025);
#7349=VERTEX_POINT('',#31026);
#7350=VERTEX_POINT('',#31079);
#7351=VERTEX_POINT('',#31080);
#7352=VERTEX_POINT('',#31136);
#7353=VERTEX_POINT('',#31137);
#7354=VERTEX_POINT('',#31196);
#7355=VERTEX_POINT('',#31197);
#7356=VERTEX_POINT('',#31253);
#7357=VERTEX_POINT('',#31254);
#7358=VERTEX_POINT('',#31310);
#7359=VERTEX_POINT('',#31311);
#7360=VERTEX_POINT('',#31370);
#7361=VERTEX_POINT('',#31371);
#7362=VERTEX_POINT('',#31427);
#7363=VERTEX_POINT('',#31428);
#7364=VERTEX_POINT('',#31487);
#7365=VERTEX_POINT('',#31488);
#7366=VERTEX_POINT('',#31490);
#7367=VERTEX_POINT('',#31504);
#7368=VERTEX_POINT('',#31506);
#7369=VERTEX_POINT('',#31509);
#7370=VERTEX_POINT('',#31519);
#7371=VERTEX_POINT('',#31520);
#7372=VERTEX_POINT('',#31609);
#7373=VERTEX_POINT('',#31610);
#7374=VERTEX_POINT('',#31693);
#7375=VERTEX_POINT('',#31694);
#7376=VERTEX_POINT('',#31783);
#7377=VERTEX_POINT('',#31784);
#7378=VERTEX_POINT('',#31873);
#7379=VERTEX_POINT('',#31874);
#7380=VERTEX_POINT('',#31957);
#7381=VERTEX_POINT('',#31958);
#7382=VERTEX_POINT('',#32047);
#7383=VERTEX_POINT('',#32048);
#7384=VERTEX_POINT('',#32131);
#7385=VERTEX_POINT('',#32132);
#7386=VERTEX_POINT('',#32221);
#7387=VERTEX_POINT('',#32222);
#7388=VERTEX_POINT('',#32311);
#7389=VERTEX_POINT('',#32312);
#7390=VERTEX_POINT('',#32395);
#7391=VERTEX_POINT('',#32396);
#7392=VERTEX_POINT('',#32485);
#7393=VERTEX_POINT('',#32486);
#7394=VERTEX_POINT('',#32575);
#7395=VERTEX_POINT('',#32576);
#7396=VERTEX_POINT('',#32659);
#7397=VERTEX_POINT('',#32660);
#7398=VERTEX_POINT('',#32749);
#7399=VERTEX_POINT('',#32750);
#7400=VERTEX_POINT('',#32833);
#7401=VERTEX_POINT('',#32834);
#7402=VERTEX_POINT('',#32836);
#7403=VERTEX_POINT('',#32846);
#7404=VERTEX_POINT('',#32855);
#7405=VERTEX_POINT('',#32856);
#7406=VERTEX_POINT('',#32892);
#7407=VERTEX_POINT('',#32893);
#7408=VERTEX_POINT('',#32929);
#7409=VERTEX_POINT('',#32930);
#7410=VERTEX_POINT('',#32966);
#7411=VERTEX_POINT('',#32967);
#7412=VERTEX_POINT('',#33003);
#7413=VERTEX_POINT('',#33004);
#7414=VERTEX_POINT('',#33041);
#7415=VERTEX_POINT('',#33042);
#7416=VERTEX_POINT('',#33078);
#7417=VERTEX_POINT('',#33079);
#7418=VERTEX_POINT('',#33115);
#7419=VERTEX_POINT('',#33116);
#7420=VERTEX_POINT('',#33153);
#7421=VERTEX_POINT('',#33154);
#7422=VERTEX_POINT('',#33190);
#7423=VERTEX_POINT('',#33191);
#7424=VERTEX_POINT('',#33227);
#7425=VERTEX_POINT('',#33228);
#7426=VERTEX_POINT('',#33264);
#7427=VERTEX_POINT('',#33265);
#7428=VERTEX_POINT('',#33301);
#7429=VERTEX_POINT('',#33302);
#7430=VERTEX_POINT('',#33339);
#7431=VERTEX_POINT('',#33340);
#7432=VERTEX_POINT('',#33376);
#7433=VERTEX_POINT('',#33377);
#7434=VERTEX_POINT('',#33413);
#7435=VERTEX_POINT('',#33414);
#7436=VERTEX_POINT('',#33416);
#7437=VERTEX_POINT('',#33426);
#7438=VERTEX_POINT('',#33427);
#7439=VERTEX_POINT('',#33441);
#7440=VERTEX_POINT('',#33457);
#7441=VERTEX_POINT('',#33458);
#7442=VERTEX_POINT('',#33485);
#7443=VERTEX_POINT('',#33486);
#7444=VERTEX_POINT('',#33513);
#7445=VERTEX_POINT('',#33514);
#7446=VERTEX_POINT('',#33554);
#7447=VERTEX_POINT('',#33555);
#7448=VERTEX_POINT('',#33595);
#7449=VERTEX_POINT('',#33596);
#7450=VERTEX_POINT('',#33623);
#7451=VERTEX_POINT('',#33624);
#7452=VERTEX_POINT('',#33651);
#7453=VERTEX_POINT('',#33652);
#7454=VERTEX_POINT('',#33692);
#7455=VERTEX_POINT('',#33693);
#7456=VERTEX_POINT('',#33733);
#7457=VERTEX_POINT('',#33734);
#7458=VERTEX_POINT('',#33762);
#7459=VERTEX_POINT('',#33763);
#7460=VERTEX_POINT('',#33790);
#7461=VERTEX_POINT('',#33791);
#7462=VERTEX_POINT('',#33818);
#7463=VERTEX_POINT('',#33819);
#7464=VERTEX_POINT('',#33846);
#7465=VERTEX_POINT('',#33847);
#7466=VERTEX_POINT('',#33887);
#7467=VERTEX_POINT('',#33888);
#7468=VERTEX_POINT('',#33928);
#7469=VERTEX_POINT('',#33929);
#7470=VERTEX_POINT('',#33956);
#7471=VERTEX_POINT('',#33957);
#7472=VERTEX_POINT('',#33984);
#7473=VERTEX_POINT('',#33985);
#7474=VERTEX_POINT('',#34025);
#7475=VERTEX_POINT('',#34026);
#7476=VERTEX_POINT('',#34066);
#7477=VERTEX_POINT('',#34067);
#7478=VERTEX_POINT('',#34095);
#7479=VERTEX_POINT('',#34096);
#7480=VERTEX_POINT('',#34123);
#7481=VERTEX_POINT('',#34124);
#7482=VERTEX_POINT('',#34151);
#7483=VERTEX_POINT('',#34152);
#7484=VERTEX_POINT('',#34179);
#7485=VERTEX_POINT('',#34180);
#7486=VERTEX_POINT('',#34220);
#7487=VERTEX_POINT('',#34221);
#7488=VERTEX_POINT('',#34261);
#7489=VERTEX_POINT('',#34262);
#7490=VERTEX_POINT('',#34289);
#7491=VERTEX_POINT('',#34290);
#7492=VERTEX_POINT('',#34316);
#7493=VERTEX_POINT('',#34317);
#7494=VERTEX_POINT('',#34358);
#7495=VERTEX_POINT('',#34359);
#7496=VERTEX_POINT('',#34399);
#7497=VERTEX_POINT('',#34400);
#7498=VERTEX_POINT('',#34428);
#7499=VERTEX_POINT('',#34429);
#7500=VERTEX_POINT('',#34455);
#7501=VERTEX_POINT('',#34456);
#7502=VERTEX_POINT('',#34496);
#7503=VERTEX_POINT('',#34497);
#7504=VERTEX_POINT('',#34538);
#7505=VERTEX_POINT('',#34539);
#7506=VERTEX_POINT('',#34566);
#7507=VERTEX_POINT('',#34567);
#7508=VERTEX_POINT('',#34593);
#7509=VERTEX_POINT('',#34594);
#7510=VERTEX_POINT('',#34634);
#7511=VERTEX_POINT('',#34635);
#7512=VERTEX_POINT('',#34663);
#7513=VERTEX_POINT('',#34664);
#7514=VERTEX_POINT('',#34705);
#7515=VERTEX_POINT('',#34706);
#7516=VERTEX_POINT('',#34732);
#7517=VERTEX_POINT('',#34733);
#7518=VERTEX_POINT('',#34773);
#7519=VERTEX_POINT('',#34774);
#7520=VERTEX_POINT('',#34802);
#7521=VERTEX_POINT('',#34803);
#7522=VERTEX_POINT('',#34843);
#7523=VERTEX_POINT('',#34844);
#7524=VERTEX_POINT('',#34885);
#7525=VERTEX_POINT('',#34886);
#7526=VERTEX_POINT('',#34913);
#7527=VERTEX_POINT('',#34914);
#7528=VERTEX_POINT('',#34940);
#7529=VERTEX_POINT('',#34941);
#7530=VERTEX_POINT('',#34981);
#7531=VERTEX_POINT('',#34982);
#7532=VERTEX_POINT('',#35010);
#7533=VERTEX_POINT('',#35011);
#7534=VERTEX_POINT('',#35039);
#7535=VERTEX_POINT('',#35040);
#7536=VERTEX_POINT('',#35066);
#7537=VERTEX_POINT('',#35067);
#7538=VERTEX_POINT('',#35107);
#7539=VERTEX_POINT('',#35108);
#7540=VERTEX_POINT('',#35136);
#7541=VERTEX_POINT('',#35137);
#7542=VERTEX_POINT('',#35177);
#7543=VERTEX_POINT('',#35178);
#7544=VERTEX_POINT('',#35219);
#7545=VERTEX_POINT('',#35220);
#7546=VERTEX_POINT('',#35247);
#7547=VERTEX_POINT('',#35248);
#7548=VERTEX_POINT('',#35274);
#7549=VERTEX_POINT('',#35275);
#7550=VERTEX_POINT('',#35315);
#7551=VERTEX_POINT('',#35316);
#7552=VERTEX_POINT('',#35344);
#7553=VERTEX_POINT('',#35345);
#7554=VERTEX_POINT('',#35373);
#7555=VERTEX_POINT('',#35374);
#7556=VERTEX_POINT('',#35400);
#7557=VERTEX_POINT('',#35401);
#7558=VERTEX_POINT('',#35428);
#7559=VERTEX_POINT('',#35429);
#7560=VERTEX_POINT('',#35457);
#7561=VERTEX_POINT('',#35458);
#7562=VERTEX_POINT('',#35506);
#7563=VERTEX_POINT('',#35622);
#7564=VERTEX_POINT('',#35624);
#7565=VERTEX_POINT('',#37812);
#7566=VERTEX_POINT('',#37935);
#7567=VERTEX_POINT('',#40131);
#7568=VERTEX_POINT('',#40244);
#7569=VERTEX_POINT('',#40246);
#7570=VERTEX_POINT('',#41236);
#7571=VERTEX_POINT('',#41364);
#7572=VERTEX_POINT('',#42363);
#7573=VERTEX_POINT('',#42364);
#7574=VERTEX_POINT('',#42366);
#7575=VERTEX_POINT('',#42396);
#7576=VERTEX_POINT('',#42503);
#7577=VERTEX_POINT('',#42508);
#7578=VERTEX_POINT('',#42510);
#7579=VERTEX_POINT('',#42536);
#7580=VERTEX_POINT('',#42548);
#7581=VERTEX_POINT('',#42631);
#7582=VERTEX_POINT('',#42639);
#7583=VERTEX_POINT('',#42644);
#7584=VERTEX_POINT('',#42684);
#7585=VERTEX_POINT('',#42686);
#7586=VERTEX_POINT('',#42693);
#7587=VERTEX_POINT('',#42695);
#7588=VERTEX_POINT('',#42702);
#7589=VERTEX_POINT('',#42709);
#7590=VERTEX_POINT('',#42716);
#7591=VERTEX_POINT('',#42718);
#7592=VERTEX_POINT('',#42748);
#7593=VERTEX_POINT('',#42855);
#7594=VERTEX_POINT('',#42860);
#7595=VERTEX_POINT('',#42862);
#7596=VERTEX_POINT('',#42888);
#7597=VERTEX_POINT('',#42900);
#7598=VERTEX_POINT('',#43015);
#7599=VERTEX_POINT('',#43017);
#7600=VERTEX_POINT('',#43024);
#7601=VERTEX_POINT('',#43031);
#7602=VERTEX_POINT('',#43038);
#7603=VERTEX_POINT('',#43040);
#7604=VERTEX_POINT('',#43070);
#7605=VERTEX_POINT('',#43177);
#7606=VERTEX_POINT('',#43182);
#7607=VERTEX_POINT('',#43184);
#7608=VERTEX_POINT('',#43210);
#7609=VERTEX_POINT('',#43222);
#7610=VERTEX_POINT('',#43337);
#7611=VERTEX_POINT('',#43339);
#7612=VERTEX_POINT('',#43346);
#7613=VERTEX_POINT('',#43353);
#7614=VERTEX_POINT('',#43360);
#7615=VERTEX_POINT('',#43362);
#7616=VERTEX_POINT('',#43392);
#7617=VERTEX_POINT('',#43499);
#7618=VERTEX_POINT('',#43504);
#7619=VERTEX_POINT('',#43506);
#7620=VERTEX_POINT('',#43532);
#7621=VERTEX_POINT('',#43544);
#7622=VERTEX_POINT('',#43659);
#7623=VERTEX_POINT('',#43661);
#7624=VERTEX_POINT('',#43668);
#7625=VERTEX_POINT('',#43675);
#7626=VERTEX_POINT('',#43682);
#7627=VERTEX_POINT('',#43684);
#7628=VERTEX_POINT('',#43714);
#7629=VERTEX_POINT('',#43821);
#7630=VERTEX_POINT('',#43826);
#7631=VERTEX_POINT('',#43828);
#7632=VERTEX_POINT('',#43854);
#7633=VERTEX_POINT('',#43879);
#7634=VERTEX_POINT('',#43994);
#7635=VERTEX_POINT('',#43996);
#7636=VERTEX_POINT('',#44003);
#7637=VERTEX_POINT('',#44010);
#7638=VERTEX_POINT('',#44017);
#7639=VERTEX_POINT('',#44019);
#7640=VERTEX_POINT('',#44049);
#7641=VERTEX_POINT('',#44156);
#7642=VERTEX_POINT('',#44161);
#7643=VERTEX_POINT('',#44163);
#7644=VERTEX_POINT('',#44189);
#7645=VERTEX_POINT('',#44201);
#7646=VERTEX_POINT('',#44316);
#7647=VERTEX_POINT('',#44318);
#7648=VERTEX_POINT('',#44325);
#7649=VERTEX_POINT('',#44332);
#7650=VERTEX_POINT('',#44339);
#7651=VERTEX_POINT('',#44341);
#7652=VERTEX_POINT('',#44371);
#7653=VERTEX_POINT('',#44478);
#7654=VERTEX_POINT('',#44483);
#7655=VERTEX_POINT('',#44485);
#7656=VERTEX_POINT('',#44511);
#7657=VERTEX_POINT('',#44523);
#7658=VERTEX_POINT('',#44638);
#7659=VERTEX_POINT('',#44640);
#7660=VERTEX_POINT('',#44647);
#7661=VERTEX_POINT('',#44654);
#7662=VERTEX_POINT('',#44661);
#7663=VERTEX_POINT('',#44662);
#7664=VERTEX_POINT('',#44665);
#7665=VERTEX_POINT('',#44695);
#7666=VERTEX_POINT('',#44802);
#7667=VERTEX_POINT('',#44809);
#7668=VERTEX_POINT('',#44811);
#7669=VERTEX_POINT('',#44837);
#7670=VERTEX_POINT('',#44849);
#7671=VERTEX_POINT('',#44962);
#7672=VERTEX_POINT('',#44966);
#7673=VERTEX_POINT('',#44968);
#7674=VERTEX_POINT('',#44975);
#7675=VERTEX_POINT('',#44982);
#7676=VERTEX_POINT('',#44989);
#7677=VERTEX_POINT('',#44991);
#7678=VERTEX_POINT('',#45021);
#7679=VERTEX_POINT('',#45128);
#7680=VERTEX_POINT('',#45133);
#7681=VERTEX_POINT('',#45135);
#7682=VERTEX_POINT('',#45161);
#7683=VERTEX_POINT('',#45173);
#7684=VERTEX_POINT('',#45288);
#7685=VERTEX_POINT('',#45290);
#7686=VERTEX_POINT('',#45297);
#7687=VERTEX_POINT('',#45304);
#7688=VERTEX_POINT('',#45311);
#7689=VERTEX_POINT('',#45313);
#7690=VERTEX_POINT('',#45343);
#7691=VERTEX_POINT('',#45450);
#7692=VERTEX_POINT('',#45455);
#7693=VERTEX_POINT('',#45457);
#7694=VERTEX_POINT('',#45483);
#7695=VERTEX_POINT('',#45495);
#7696=VERTEX_POINT('',#45610);
#7697=VERTEX_POINT('',#45612);
#7698=VERTEX_POINT('',#45619);
#7699=VERTEX_POINT('',#45626);
#7700=VERTEX_POINT('',#45633);
#7701=VERTEX_POINT('',#45635);
#7702=VERTEX_POINT('',#45665);
#7703=VERTEX_POINT('',#45772);
#7704=VERTEX_POINT('',#45777);
#7705=VERTEX_POINT('',#45779);
#7706=VERTEX_POINT('',#45805);
#7707=VERTEX_POINT('',#45817);
#7708=VERTEX_POINT('',#45932);
#7709=VERTEX_POINT('',#45934);
#7710=VERTEX_POINT('',#45944);
#7711=VERTEX_POINT('',#45951);
#7712=VERTEX_POINT('',#45961);
#7713=VERTEX_POINT('',#45963);
#7714=VERTEX_POINT('',#45993);
#7715=VERTEX_POINT('',#46100);
#7716=VERTEX_POINT('',#46105);
#7717=VERTEX_POINT('',#46107);
#7718=VERTEX_POINT('',#46133);
#7719=VERTEX_POINT('',#46145);
#7720=VERTEX_POINT('',#46260);
#7721=VERTEX_POINT('',#46262);
#7722=VERTEX_POINT('',#46269);
#7723=VERTEX_POINT('',#46276);
#7724=VERTEX_POINT('',#46283);
#7725=VERTEX_POINT('',#46285);
#7726=VERTEX_POINT('',#46315);
#7727=VERTEX_POINT('',#46422);
#7728=VERTEX_POINT('',#46427);
#7729=VERTEX_POINT('',#46429);
#7730=VERTEX_POINT('',#46455);
#7731=VERTEX_POINT('',#46467);
#7732=VERTEX_POINT('',#46582);
#7733=VERTEX_POINT('',#46584);
#7734=VERTEX_POINT('',#46591);
#7735=VERTEX_POINT('',#46598);
#7736=VERTEX_POINT('',#46605);
#7737=VERTEX_POINT('',#46607);
#7738=VERTEX_POINT('',#46637);
#7739=VERTEX_POINT('',#46744);
#7740=VERTEX_POINT('',#46749);
#7741=VERTEX_POINT('',#46751);
#7742=VERTEX_POINT('',#46777);
#7743=VERTEX_POINT('',#46789);
#7744=VERTEX_POINT('',#46904);
#7745=VERTEX_POINT('',#46906);
#7746=VERTEX_POINT('',#46913);
#7747=VERTEX_POINT('',#46920);
#7748=VERTEX_POINT('',#47006);
#7749=VERTEX_POINT('',#47036);
#7750=VERTEX_POINT('',#47069);
#7751=VERTEX_POINT('',#47097);
#7752=VERTEX_POINT('',#47180);
#7753=VERTEX_POINT('',#47181);
#7754=VERTEX_POINT('',#47224);
#7755=VERTEX_POINT('',#47235);
#7756=VERTEX_POINT('',#47241);
#7757=VERTEX_POINT('',#47242);
#7758=VERTEX_POINT('',#47244);
#7759=VERTEX_POINT('',#47246);
#7760=VERTEX_POINT('',#47250);
#7761=VERTEX_POINT('',#47251);
#7762=VERTEX_POINT('',#47256);
#7763=VERTEX_POINT('',#47257);
#7764=VERTEX_POINT('',#47260);
#7765=VERTEX_POINT('',#47264);
#7766=VERTEX_POINT('',#47265);
#7767=VERTEX_POINT('',#47267);
#7768=VERTEX_POINT('',#47274);
#7769=VERTEX_POINT('',#47275);
#7770=VERTEX_POINT('',#47277);
#7771=VERTEX_POINT('',#47279);
#7772=VERTEX_POINT('',#47283);
#7773=VERTEX_POINT('',#47284);
#7774=VERTEX_POINT('',#47289);
#7775=VERTEX_POINT('',#47291);
#7776=VERTEX_POINT('',#47298);
#7777=VERTEX_POINT('',#47300);
#7778=VERTEX_POINT('',#47306);
#7779=VERTEX_POINT('',#47310);
#7780=VERTEX_POINT('',#47314);
#7781=VERTEX_POINT('',#47323);
#7782=VERTEX_POINT('',#47335);
#7783=VERTEX_POINT('',#47336);
#7784=VERTEX_POINT('',#47343);
#7785=VERTEX_POINT('',#47345);
#7786=VERTEX_POINT('',#47347);
#7787=VERTEX_POINT('',#47354);
#7788=VERTEX_POINT('',#47356);
#7789=VERTEX_POINT('',#47358);
#7790=VERTEX_POINT('',#47362);
#7791=VERTEX_POINT('',#47368);
#7792=VERTEX_POINT('',#47370);
#7793=VERTEX_POINT('',#47374);
#7794=VERTEX_POINT('',#47376);
#7795=VERTEX_POINT('',#47380);
#7796=VERTEX_POINT('',#47381);
#7797=VERTEX_POINT('',#47384);
#7798=VERTEX_POINT('',#47390);
#7799=VERTEX_POINT('',#47392);
#7800=VERTEX_POINT('',#47406);
#7801=VERTEX_POINT('',#47408);
#7802=VERTEX_POINT('',#47412);
#7803=VERTEX_POINT('',#47414);
#7804=VERTEX_POINT('',#47418);
#7805=VERTEX_POINT('',#47425);
#7806=VERTEX_POINT('',#47429);
#7807=VERTEX_POINT('',#47436);
#7808=VERTEX_POINT('',#47438);
#7809=VERTEX_POINT('',#47442);
#7810=VERTEX_POINT('',#47444);
#7811=VERTEX_POINT('',#47446);
#7812=VERTEX_POINT('',#47450);
#7813=VERTEX_POINT('',#47452);
#7814=VERTEX_POINT('',#47461);
#7815=VERTEX_POINT('',#47467);
#7816=VERTEX_POINT('',#47471);
#7817=VERTEX_POINT('',#47473);
#7818=VERTEX_POINT('',#47478);
#7819=VERTEX_POINT('',#47491);
#7820=VERTEX_POINT('',#47506);
#7821=VERTEX_POINT('',#47507);
#7822=VERTEX_POINT('',#47509);
#7823=VERTEX_POINT('',#47511);
#7824=VERTEX_POINT('',#47515);
#7825=VERTEX_POINT('',#47517);
#7826=VERTEX_POINT('',#47519);
#7827=VERTEX_POINT('',#47523);
#7828=VERTEX_POINT('',#47524);
#7829=VERTEX_POINT('',#47529);
#7830=VERTEX_POINT('',#47531);
#7831=VERTEX_POINT('',#47535);
#7832=VERTEX_POINT('',#47537);
#7833=VERTEX_POINT('',#47541);
#7834=VERTEX_POINT('',#47543);
#7835=VERTEX_POINT('',#47549);
#7836=VERTEX_POINT('',#47551);
#7837=VERTEX_POINT('',#47557);
#7838=VERTEX_POINT('',#47563);
#7839=VERTEX_POINT('',#47567);
#7840=VERTEX_POINT('',#47571);
#7841=VERTEX_POINT('',#47575);
#7842=VERTEX_POINT('',#47579);
#7843=VERTEX_POINT('',#47583);
#7844=VERTEX_POINT('',#47587);
#7845=VERTEX_POINT('',#47591);
#7846=VERTEX_POINT('',#47592);
#7847=VERTEX_POINT('',#47594);
#7848=VERTEX_POINT('',#47596);
#7849=VERTEX_POINT('',#47600);
#7850=VERTEX_POINT('',#47601);
#7851=VERTEX_POINT('',#47613);
#7852=VERTEX_POINT('',#47616);
#7853=VERTEX_POINT('',#47622);
#7854=VERTEX_POINT('',#47624);
#7855=VERTEX_POINT('',#47628);
#7856=VERTEX_POINT('',#47632);
#7857=VERTEX_POINT('',#47637);
#7858=VERTEX_POINT('',#47639);
#7859=VERTEX_POINT('',#47646);
#7860=VERTEX_POINT('',#47653);
#7861=VERTEX_POINT('',#47665);
#7862=VERTEX_POINT('',#47669);
#7863=VERTEX_POINT('',#47673);
#7864=VERTEX_POINT('',#47675);
#7865=VERTEX_POINT('',#47679);
#7866=VERTEX_POINT('',#47686);
#7867=VERTEX_POINT('',#47697);
#7868=VERTEX_POINT('',#47703);
#7869=VERTEX_POINT('',#47707);
#7870=VERTEX_POINT('',#47715);
#7871=VERTEX_POINT('',#47716);
#7872=VERTEX_POINT('',#47725);
#7873=VERTEX_POINT('',#47727);
#7874=VERTEX_POINT('',#47729);
#7875=VERTEX_POINT('',#47733);
#7876=VERTEX_POINT('',#47734);
#7877=VERTEX_POINT('',#47736);
#7878=VERTEX_POINT('',#47739);
#7879=VERTEX_POINT('',#47745);
#7880=VERTEX_POINT('',#47747);
#7881=VERTEX_POINT('',#47751);
#7882=VERTEX_POINT('',#47753);
#7883=VERTEX_POINT('',#47757);
#7884=VERTEX_POINT('',#47761);
#7885=VERTEX_POINT('',#47763);
#7886=VERTEX_POINT('',#47767);
#7887=VERTEX_POINT('',#47769);
#7888=VERTEX_POINT('',#47771);
#7889=VERTEX_POINT('',#47775);
#7890=VERTEX_POINT('',#47776);
#7891=VERTEX_POINT('',#47778);
#7892=VERTEX_POINT('',#47780);
#7893=VERTEX_POINT('',#47784);
#7894=VERTEX_POINT('',#47785);
#7895=VERTEX_POINT('',#47790);
#7896=VERTEX_POINT('',#47791);
#7897=VERTEX_POINT('',#47796);
#7898=VERTEX_POINT('',#47798);
#7899=VERTEX_POINT('',#47802);
#7900=VERTEX_POINT('',#47804);
#7901=VERTEX_POINT('',#47808);
#7902=VERTEX_POINT('',#47810);
#7903=VERTEX_POINT('',#47814);
#7904=VERTEX_POINT('',#47818);
#7905=VERTEX_POINT('',#47822);
#7906=VERTEX_POINT('',#47823);
#7907=VERTEX_POINT('',#47825);
#7908=VERTEX_POINT('',#47830);
#7909=VERTEX_POINT('',#47836);
#7910=VERTEX_POINT('',#47837);
#7911=VERTEX_POINT('',#47840);
#7912=VERTEX_POINT('',#47844);
#7913=VERTEX_POINT('',#47848);
#7914=VERTEX_POINT('',#47852);
#7915=VERTEX_POINT('',#47856);
#7916=VERTEX_POINT('',#47860);
#7917=VERTEX_POINT('',#47868);
#7918=VERTEX_POINT('',#47870);
#7919=VERTEX_POINT('',#47876);
#7920=VERTEX_POINT('',#47878);
#7921=VERTEX_POINT('',#47885);
#7922=VERTEX_POINT('',#47889);
#7923=VERTEX_POINT('',#47897);
#7924=VERTEX_POINT('',#47898);
#7925=VERTEX_POINT('',#47900);
#7926=VERTEX_POINT('',#47902);
#7927=VERTEX_POINT('',#47907);
#7928=VERTEX_POINT('',#47911);
#7929=VERTEX_POINT('',#47921);
#7930=VERTEX_POINT('',#47934);
#7931=VERTEX_POINT('',#47936);
#7932=VERTEX_POINT('',#47952);
#7933=VERTEX_POINT('',#47965);
#7934=VERTEX_POINT('',#47966);
#7935=VERTEX_POINT('',#47968);
#7936=VERTEX_POINT('',#47973);
#7937=VERTEX_POINT('',#47975);
#7938=VERTEX_POINT('',#47977);
#7939=VERTEX_POINT('',#47979);
#7940=VERTEX_POINT('',#47981);
#7941=VERTEX_POINT('',#47983);
#7942=VERTEX_POINT('',#47985);
#7943=VERTEX_POINT('',#47987);
#7944=VERTEX_POINT('',#47989);
#7945=VERTEX_POINT('',#47991);
#7946=VERTEX_POINT('',#47993);
#7947=VERTEX_POINT('',#47995);
#7948=VERTEX_POINT('',#47997);
#7949=VERTEX_POINT('',#47999);
#7950=VERTEX_POINT('',#48001);
#7951=VERTEX_POINT('',#48003);
#7952=VERTEX_POINT('',#48005);
#7953=VERTEX_POINT('',#48009);
#7954=VERTEX_POINT('',#48012);
#7955=VERTEX_POINT('',#48013);
#7956=VERTEX_POINT('',#48024);
#7957=VERTEX_POINT('',#48026);
#7958=VERTEX_POINT('',#48028);
#7959=VERTEX_POINT('',#48041);
#7960=VERTEX_POINT('',#48042);
#7961=VERTEX_POINT('',#48047);
#7962=VERTEX_POINT('',#48048);
#7963=VERTEX_POINT('',#48053);
#7964=VERTEX_POINT('',#48057);
#7965=VERTEX_POINT('',#48058);
#7966=VERTEX_POINT('',#48060);
#7967=VERTEX_POINT('',#48062);
#7968=VERTEX_POINT('',#48103);
#7969=VERTEX_POINT('',#48105);
#7970=VERTEX_POINT('',#48107);
#7971=VERTEX_POINT('',#48109);
#7972=VERTEX_POINT('',#48111);
#7973=VERTEX_POINT('',#48113);
#7974=VERTEX_POINT('',#48115);
#7975=VERTEX_POINT('',#48117);
#7976=VERTEX_POINT('',#48119);
#7977=VERTEX_POINT('',#48121);
#7978=VERTEX_POINT('',#48123);
#7979=VERTEX_POINT('',#48125);
#7980=VERTEX_POINT('',#48128);
#7981=VERTEX_POINT('',#48131);
#7982=VERTEX_POINT('',#48135);
#7983=VERTEX_POINT('',#48144);
#7984=VERTEX_POINT('',#48146);
#7985=VERTEX_POINT('',#48163);
#7986=VERTEX_POINT('',#48164);
#7987=VERTEX_POINT('',#48175);
#7988=VERTEX_POINT('',#48189);
#7989=VERTEX_POINT('',#48193);
#7990=VERTEX_POINT('',#48200);
#7991=VERTEX_POINT('',#48204);
#7992=VERTEX_POINT('',#48208);
#7993=VERTEX_POINT('',#48215);
#7994=VERTEX_POINT('',#48219);
#7995=VERTEX_POINT('',#48224);
#7996=VERTEX_POINT('',#48226);
#7997=VERTEX_POINT('',#48233);
#7998=VERTEX_POINT('',#48237);
#7999=VERTEX_POINT('',#48250);
#8000=VERTEX_POINT('',#48252);
#8001=VERTEX_POINT('',#48306);
#8002=VERTEX_POINT('',#48307);
#8003=VERTEX_POINT('',#48313);
#8004=VERTEX_POINT('',#48322);
#8005=VERTEX_POINT('',#48337);
#8006=VERTEX_POINT('',#48340);
#8007=VERTEX_POINT('',#48345);
#8008=VERTEX_POINT('',#48348);
#8009=VERTEX_POINT('',#48352);
#8010=VERTEX_POINT('',#48357);
#8011=VERTEX_POINT('',#48359);
#8012=VERTEX_POINT('',#48366);
#8013=VERTEX_POINT('',#48390);
#8014=VERTEX_POINT('',#48412);
#8015=VERTEX_POINT('',#48431);
#8016=VERTEX_POINT('',#48433);
#8017=VERTEX_POINT('',#48444);
#8018=VERTEX_POINT('',#48448);
#8019=VERTEX_POINT('',#48450);
#8020=VERTEX_POINT('',#48457);
#8021=VERTEX_POINT('',#48470);
#8022=VERTEX_POINT('',#48472);
#8023=VERTEX_POINT('',#48498);
#8024=VERTEX_POINT('',#48499);
#8025=VERTEX_POINT('',#48501);
#8026=VERTEX_POINT('',#48517);
#8027=VERTEX_POINT('',#48521);
#8028=VERTEX_POINT('',#48528);
#8029=VERTEX_POINT('',#48537);
#8030=VERTEX_POINT('',#48539);
#8031=VERTEX_POINT('',#48542);
#8032=VERTEX_POINT('',#48545);
#8033=VERTEX_POINT('',#48576);
#8034=VERTEX_POINT('',#48583);
#8035=VERTEX_POINT('',#48598);
#8036=VERTEX_POINT('',#48604);
#8037=VERTEX_POINT('',#48608);
#8038=VERTEX_POINT('',#48618);
#8039=VERTEX_POINT('',#48620);
#8040=VERTEX_POINT('',#48630);
#8041=VERTEX_POINT('',#48634);
#8042=VERTEX_POINT('',#48636);
#8043=VERTEX_POINT('',#48640);
#8044=VERTEX_POINT('',#48641);
#8045=VERTEX_POINT('',#48643);
#8046=VERTEX_POINT('',#48647);
#8047=VERTEX_POINT('',#48648);
#8048=VERTEX_POINT('',#48653);
#8049=VERTEX_POINT('',#48655);
#8050=VERTEX_POINT('',#48657);
#8051=VERTEX_POINT('',#48659);
#8052=VERTEX_POINT('',#48663);
#8053=VERTEX_POINT('',#48667);
#8054=VERTEX_POINT('',#48668);
#8055=VERTEX_POINT('',#48670);
#8056=VERTEX_POINT('',#48672);
#8057=VERTEX_POINT('',#48674);
#8058=VERTEX_POINT('',#48676);
#8059=VERTEX_POINT('',#48680);
#8060=VERTEX_POINT('',#48682);
#8061=VERTEX_POINT('',#48684);
#8062=VERTEX_POINT('',#48688);
#8063=VERTEX_POINT('',#48692);
#8064=VERTEX_POINT('',#48694);
#8065=VERTEX_POINT('',#48701);
#8066=VERTEX_POINT('',#48703);
#8067=VERTEX_POINT('',#48707);
#8068=VERTEX_POINT('',#48709);
#8069=VERTEX_POINT('',#48713);
#8070=VERTEX_POINT('',#48715);
#8071=VERTEX_POINT('',#48727);
#8072=VERTEX_POINT('',#48730);
#8073=VERTEX_POINT('',#48734);
#8074=VERTEX_POINT('',#48736);
#8075=VERTEX_POINT('',#48740);
#8076=VERTEX_POINT('',#48742);
#8077=VERTEX_POINT('',#48748);
#8078=VERTEX_POINT('',#48754);
#8079=VERTEX_POINT('',#48758);
#8080=VERTEX_POINT('',#48759);
#8081=VERTEX_POINT('',#48764);
#8082=VERTEX_POINT('',#48766);
#8083=VERTEX_POINT('',#48772);
#8084=VERTEX_POINT('',#48776);
#8085=VERTEX_POINT('',#48784);
#8086=VERTEX_POINT('',#48788);
#8087=VERTEX_POINT('',#48792);
#8088=VERTEX_POINT('',#48793);
#8089=VERTEX_POINT('',#48795);
#8090=VERTEX_POINT('',#48800);
#8091=VERTEX_POINT('',#48801);
#8092=VERTEX_POINT('',#48806);
#8093=VERTEX_POINT('',#48809);
#8094=VERTEX_POINT('',#48810);
#8095=VERTEX_POINT('',#48815);
#8096=VERTEX_POINT('',#48816);
#8097=VERTEX_POINT('',#48824);
#8098=VERTEX_POINT('',#48829);
#8099=VERTEX_POINT('',#48832);
#8100=VERTEX_POINT('',#48838);
#8101=VERTEX_POINT('',#48842);
#8102=VERTEX_POINT('',#48848);
#8103=VERTEX_POINT('',#48850);
#8104=VERTEX_POINT('',#48852);
#8105=VERTEX_POINT('',#48858);
#8106=VERTEX_POINT('',#48862);
#8107=VERTEX_POINT('',#48864);
#8108=VERTEX_POINT('',#48868);
#8109=VERTEX_POINT('',#48872);
#8110=VERTEX_POINT('',#48874);
#8111=VERTEX_POINT('',#48878);
#8112=VERTEX_POINT('',#48880);
#8113=VERTEX_POINT('',#48882);
#8114=VERTEX_POINT('',#48886);
#8115=VERTEX_POINT('',#48888);
#8116=VERTEX_POINT('',#48890);
#8117=VERTEX_POINT('',#48892);
#8118=VERTEX_POINT('',#48894);
#8119=VERTEX_POINT('',#48896);
#8120=VERTEX_POINT('',#48898);
#8121=VERTEX_POINT('',#48900);
#8122=VERTEX_POINT('',#48902);
#8123=VERTEX_POINT('',#48904);
#8124=VERTEX_POINT('',#48906);
#8125=VERTEX_POINT('',#48909);
#8126=VERTEX_POINT('',#48913);
#8127=VERTEX_POINT('',#48915);
#8128=VERTEX_POINT('',#48919);
#8129=VERTEX_POINT('',#48929);
#8130=VERTEX_POINT('',#48931);
#8131=VERTEX_POINT('',#48935);
#8132=VERTEX_POINT('',#48943);
#8133=VERTEX_POINT('',#48945);
#8134=VERTEX_POINT('',#48949);
#8135=VERTEX_POINT('',#48953);
#8136=VERTEX_POINT('',#48956);
#8137=VERTEX_POINT('',#48958);
#8138=VERTEX_POINT('',#48962);
#8139=VERTEX_POINT('',#48966);
#8140=VERTEX_POINT('',#48969);
#8141=VERTEX_POINT('',#48971);
#8142=VERTEX_POINT('',#48975);
#8143=VERTEX_POINT('',#48979);
#8144=VERTEX_POINT('',#48982);
#8145=VERTEX_POINT('',#48984);
#8146=VERTEX_POINT('',#48993);
#8147=VERTEX_POINT('',#48995);
#8148=VERTEX_POINT('',#48997);
#8149=VERTEX_POINT('',#49002);
#8150=VERTEX_POINT('',#49004);
#8151=VERTEX_POINT('',#49017);
#8152=VERTEX_POINT('',#49031);
#8153=VERTEX_POINT('',#49032);
#8154=VERTEX_POINT('',#49035);
#8155=VERTEX_POINT('',#49037);
#8156=VERTEX_POINT('',#49041);
#8157=VERTEX_POINT('',#49043);
#8158=VERTEX_POINT('',#49047);
#8159=VERTEX_POINT('',#49048);
#8160=VERTEX_POINT('',#49053);
#8161=VERTEX_POINT('',#49057);
#8162=VERTEX_POINT('',#49059);
#8163=VERTEX_POINT('',#49061);
#8164=VERTEX_POINT('',#49063);
#8165=VERTEX_POINT('',#49065);
#8166=VERTEX_POINT('',#49067);
#8167=VERTEX_POINT('',#49069);
#8168=VERTEX_POINT('',#49078);
#8169=VERTEX_POINT('',#49079);
#8170=VERTEX_POINT('',#49084);
#8171=VERTEX_POINT('',#49086);
#8172=VERTEX_POINT('',#49090);
#8173=VERTEX_POINT('',#49091);
#8174=VERTEX_POINT('',#49096);
#8175=VERTEX_POINT('',#49098);
#8176=VERTEX_POINT('',#49104);
#8177=VERTEX_POINT('',#49106);
#8178=VERTEX_POINT('',#49110);
#8179=VERTEX_POINT('',#49111);
#8180=VERTEX_POINT('',#49116);
#8181=VERTEX_POINT('',#49117);
#8182=VERTEX_POINT('',#49122);
#8183=VERTEX_POINT('',#49125);
#8184=VERTEX_POINT('',#49127);
#8185=VERTEX_POINT('',#49138);
#8186=VERTEX_POINT('',#49143);
#8187=VERTEX_POINT('',#49155);
#8188=VERTEX_POINT('',#49157);
#8189=VERTEX_POINT('',#49159);
#8190=VERTEX_POINT('',#49165);
#8191=VERTEX_POINT('',#49167);
#8192=VERTEX_POINT('',#49169);
#8193=VERTEX_POINT('',#49174);
#8194=VERTEX_POINT('',#49176);
#8195=VERTEX_POINT('',#49182);
#8196=VERTEX_POINT('',#49184);
#8197=VERTEX_POINT('',#49190);
#8198=VERTEX_POINT('',#49191);
#8199=VERTEX_POINT('',#49196);
#8200=VERTEX_POINT('',#49198);
#8201=VERTEX_POINT('',#49229);
#8202=VERTEX_POINT('',#49230);
#8203=VERTEX_POINT('',#49233);
#8204=VERTEX_POINT('',#49237);
#8205=VERTEX_POINT('',#49239);
#8206=VERTEX_POINT('',#49243);
#8207=VERTEX_POINT('',#49244);
#8208=VERTEX_POINT('',#49270);
#8209=VERTEX_POINT('',#49272);
#8210=VERTEX_POINT('',#49302);
#8211=VERTEX_POINT('',#49304);
#8212=VERTEX_POINT('',#49330);
#8213=VERTEX_POINT('',#49332);
#8214=VERTEX_POINT('',#49362);
#8215=VERTEX_POINT('',#49364);
#8216=VERTEX_POINT('',#49390);
#8217=VERTEX_POINT('',#49392);
#8218=VERTEX_POINT('',#49422);
#8219=VERTEX_POINT('',#49424);
#8220=VERTEX_POINT('',#49450);
#8221=VERTEX_POINT('',#49452);
#8222=VERTEX_POINT('',#49482);
#8223=VERTEX_POINT('',#49484);
#8224=VERTEX_POINT('',#49510);
#8225=VERTEX_POINT('',#49512);
#8226=VERTEX_POINT('',#49542);
#8227=VERTEX_POINT('',#49544);
#8228=VERTEX_POINT('',#49570);
#8229=VERTEX_POINT('',#49572);
#8230=VERTEX_POINT('',#49602);
#8231=VERTEX_POINT('',#49604);
#8232=VERTEX_POINT('',#49630);
#8233=VERTEX_POINT('',#49632);
#8234=VERTEX_POINT('',#49662);
#8235=VERTEX_POINT('',#49664);
#8236=VERTEX_POINT('',#49690);
#8237=VERTEX_POINT('',#49692);
#8238=VERTEX_POINT('',#49722);
#8239=VERTEX_POINT('',#49724);
#8240=VERTEX_POINT('',#49750);
#8241=VERTEX_POINT('',#49752);
#8242=VERTEX_POINT('',#49782);
#8243=VERTEX_POINT('',#49784);
#8244=VERTEX_POINT('',#49810);
#8245=VERTEX_POINT('',#49812);
#8246=VERTEX_POINT('',#49842);
#8247=VERTEX_POINT('',#49844);
#8248=VERTEX_POINT('',#49870);
#8249=VERTEX_POINT('',#49872);
#8250=VERTEX_POINT('',#49902);
#8251=VERTEX_POINT('',#49904);
#8252=VERTEX_POINT('',#49930);
#8253=VERTEX_POINT('',#49932);
#8254=VERTEX_POINT('',#49962);
#8255=VERTEX_POINT('',#49964);
#8256=VERTEX_POINT('',#49990);
#8257=VERTEX_POINT('',#49992);
#8258=VERTEX_POINT('',#50022);
#8259=VERTEX_POINT('',#50024);
#8260=VERTEX_POINT('',#50050);
#8261=VERTEX_POINT('',#50052);
#8262=VERTEX_POINT('',#50084);
#8263=VERTEX_POINT('',#50088);
#8264=VERTEX_POINT('',#50089);
#8265=VERTEX_POINT('',#50119);
#8266=VERTEX_POINT('',#50121);
#8267=VERTEX_POINT('',#50148);
#8268=VERTEX_POINT('',#50150);
#8269=VERTEX_POINT('',#50180);
#8270=VERTEX_POINT('',#50182);
#8271=VERTEX_POINT('',#50209);
#8272=VERTEX_POINT('',#50211);
#8273=VERTEX_POINT('',#50241);
#8274=VERTEX_POINT('',#50243);
#8275=VERTEX_POINT('',#50270);
#8276=VERTEX_POINT('',#50272);
#8277=VERTEX_POINT('',#50302);
#8278=VERTEX_POINT('',#50304);
#8279=VERTEX_POINT('',#50331);
#8280=VERTEX_POINT('',#50333);
#8281=VERTEX_POINT('',#50363);
#8282=VERTEX_POINT('',#50365);
#8283=VERTEX_POINT('',#50392);
#8284=VERTEX_POINT('',#50394);
#8285=VERTEX_POINT('',#50424);
#8286=VERTEX_POINT('',#50426);
#8287=VERTEX_POINT('',#50453);
#8288=VERTEX_POINT('',#50455);
#8289=VERTEX_POINT('',#50485);
#8290=VERTEX_POINT('',#50487);
#8291=VERTEX_POINT('',#50514);
#8292=VERTEX_POINT('',#50516);
#8293=VERTEX_POINT('',#50546);
#8294=VERTEX_POINT('',#50548);
#8295=VERTEX_POINT('',#50575);
#8296=VERTEX_POINT('',#50577);
#8297=VERTEX_POINT('',#50607);
#8298=VERTEX_POINT('',#50609);
#8299=VERTEX_POINT('',#50636);
#8300=VERTEX_POINT('',#50638);
#8301=VERTEX_POINT('',#50668);
#8302=VERTEX_POINT('',#50670);
#8303=VERTEX_POINT('',#50697);
#8304=VERTEX_POINT('',#50699);
#8305=VERTEX_POINT('',#50729);
#8306=VERTEX_POINT('',#50731);
#8307=VERTEX_POINT('',#50758);
#8308=VERTEX_POINT('',#50760);
#8309=VERTEX_POINT('',#50790);
#8310=VERTEX_POINT('',#50792);
#8311=VERTEX_POINT('',#50819);
#8312=VERTEX_POINT('',#50821);
#8313=VERTEX_POINT('',#50851);
#8314=VERTEX_POINT('',#50853);
#8315=VERTEX_POINT('',#50880);
#8316=VERTEX_POINT('',#50882);
#8317=VERTEX_POINT('',#50912);
#8318=VERTEX_POINT('',#50914);
#8319=VERTEX_POINT('',#50941);
#8320=VERTEX_POINT('',#50943);
#8321=VERTEX_POINT('',#50973);
#8322=VERTEX_POINT('',#50975);
#8323=VERTEX_POINT('',#51002);
#8324=VERTEX_POINT('',#51004);
#8325=VERTEX_POINT('',#51034);
#8326=VERTEX_POINT('',#51036);
#8327=VERTEX_POINT('',#51063);
#8328=VERTEX_POINT('',#51065);
#8329=VERTEX_POINT('',#51095);
#8330=VERTEX_POINT('',#51097);
#8331=VERTEX_POINT('',#51124);
#8332=VERTEX_POINT('',#51126);
#8333=VERTEX_POINT('',#51156);
#8334=VERTEX_POINT('',#51158);
#8335=VERTEX_POINT('',#51185);
#8336=VERTEX_POINT('',#51187);
#8337=VERTEX_POINT('',#51217);
#8338=VERTEX_POINT('',#51219);
#8339=VERTEX_POINT('',#51246);
#8340=VERTEX_POINT('',#51248);
#8341=VERTEX_POINT('',#51278);
#8342=VERTEX_POINT('',#51280);
#8343=VERTEX_POINT('',#51307);
#8344=VERTEX_POINT('',#51309);
#8345=VERTEX_POINT('',#51339);
#8346=VERTEX_POINT('',#51341);
#8347=VERTEX_POINT('',#51368);
#8348=VERTEX_POINT('',#51370);
#8349=VERTEX_POINT('',#51400);
#8350=VERTEX_POINT('',#51402);
#8351=VERTEX_POINT('',#51429);
#8352=VERTEX_POINT('',#51431);
#8353=VERTEX_POINT('',#51461);
#8354=VERTEX_POINT('',#51463);
#8355=VERTEX_POINT('',#51490);
#8356=VERTEX_POINT('',#51492);
#8357=VERTEX_POINT('',#51522);
#8358=VERTEX_POINT('',#51524);
#8359=VERTEX_POINT('',#51551);
#8360=VERTEX_POINT('',#51553);
#8361=VERTEX_POINT('',#51583);
#8362=VERTEX_POINT('',#51585);
#8363=VERTEX_POINT('',#51693);
#8364=VERTEX_POINT('',#51701);
#8365=VERTEX_POINT('',#51703);
#8366=VERTEX_POINT('',#51745);
#8367=VERTEX_POINT('',#51828);
#8368=VERTEX_POINT('',#51835);
#8369=VERTEX_POINT('',#51872);
#8370=VERTEX_POINT('',#51881);
#8371=VERTEX_POINT('',#51969);
#8372=VERTEX_POINT('',#51970);
#8373=VERTEX_POINT('',#51977);
#8374=VERTEX_POINT('',#52015);
#8375=VERTEX_POINT('',#52098);
#8376=VERTEX_POINT('',#52099);
#8377=VERTEX_POINT('',#52145);
#8378=VERTEX_POINT('',#52146);
#8379=VERTEX_POINT('',#52176);
#8380=VERTEX_POINT('',#52178);
#8381=VERTEX_POINT('',#52205);
#8382=VERTEX_POINT('',#52207);
#8383=VERTEX_POINT('',#52237);
#8384=VERTEX_POINT('',#52239);
#8385=VERTEX_POINT('',#52266);
#8386=VERTEX_POINT('',#52268);
#8387=VERTEX_POINT('',#52298);
#8388=VERTEX_POINT('',#52300);
#8389=VERTEX_POINT('',#52327);
#8390=VERTEX_POINT('',#52329);
#8391=VERTEX_POINT('',#52359);
#8392=VERTEX_POINT('',#52361);
#8393=VERTEX_POINT('',#52388);
#8394=VERTEX_POINT('',#52390);
#8395=VERTEX_POINT('',#52420);
#8396=VERTEX_POINT('',#52422);
#8397=VERTEX_POINT('',#52449);
#8398=VERTEX_POINT('',#52451);
#8399=VERTEX_POINT('',#52481);
#8400=VERTEX_POINT('',#52483);
#8401=VERTEX_POINT('',#52510);
#8402=VERTEX_POINT('',#52512);
#8403=VERTEX_POINT('',#52542);
#8404=VERTEX_POINT('',#52544);
#8405=VERTEX_POINT('',#52571);
#8406=VERTEX_POINT('',#52573);
#8407=VERTEX_POINT('',#52603);
#8408=VERTEX_POINT('',#52605);
#8409=VERTEX_POINT('',#52632);
#8410=VERTEX_POINT('',#52634);
#8411=VERTEX_POINT('',#52664);
#8412=VERTEX_POINT('',#52666);
#8413=VERTEX_POINT('',#52693);
#8414=VERTEX_POINT('',#52695);
#8415=VERTEX_POINT('',#52725);
#8416=VERTEX_POINT('',#52727);
#8417=VERTEX_POINT('',#52754);
#8418=VERTEX_POINT('',#52756);
#8419=VERTEX_POINT('',#52786);
#8420=VERTEX_POINT('',#52788);
#8421=VERTEX_POINT('',#52815);
#8422=VERTEX_POINT('',#52817);
#8423=VERTEX_POINT('',#52847);
#8424=VERTEX_POINT('',#52849);
#8425=VERTEX_POINT('',#52876);
#8426=VERTEX_POINT('',#52878);
#8427=VERTEX_POINT('',#52908);
#8428=VERTEX_POINT('',#52910);
#8429=VERTEX_POINT('',#52937);
#8430=VERTEX_POINT('',#52939);
#8431=VERTEX_POINT('',#52969);
#8432=VERTEX_POINT('',#52971);
#8433=VERTEX_POINT('',#52998);
#8434=VERTEX_POINT('',#53000);
#8435=VERTEX_POINT('',#53030);
#8436=VERTEX_POINT('',#53032);
#8437=VERTEX_POINT('',#53059);
#8438=VERTEX_POINT('',#53061);
#8439=VERTEX_POINT('',#53091);
#8440=VERTEX_POINT('',#53093);
#8441=VERTEX_POINT('',#53120);
#8442=VERTEX_POINT('',#53122);
#8443=VERTEX_POINT('',#53152);
#8444=VERTEX_POINT('',#53154);
#8445=VERTEX_POINT('',#53181);
#8446=VERTEX_POINT('',#53183);
#8447=VERTEX_POINT('',#53213);
#8448=VERTEX_POINT('',#53215);
#8449=VERTEX_POINT('',#53242);
#8450=VERTEX_POINT('',#53244);
#8451=VERTEX_POINT('',#53274);
#8452=VERTEX_POINT('',#53276);
#8453=VERTEX_POINT('',#53303);
#8454=VERTEX_POINT('',#53305);
#8455=VERTEX_POINT('',#53335);
#8456=VERTEX_POINT('',#53337);
#8457=VERTEX_POINT('',#53364);
#8458=VERTEX_POINT('',#53366);
#8459=VERTEX_POINT('',#53396);
#8460=VERTEX_POINT('',#53398);
#8461=VERTEX_POINT('',#53425);
#8462=VERTEX_POINT('',#53427);
#8463=VERTEX_POINT('',#53457);
#8464=VERTEX_POINT('',#53459);
#8465=VERTEX_POINT('',#53486);
#8466=VERTEX_POINT('',#53488);
#8467=VERTEX_POINT('',#53518);
#8468=VERTEX_POINT('',#53520);
#8469=VERTEX_POINT('',#53547);
#8470=VERTEX_POINT('',#53549);
#8471=VERTEX_POINT('',#53579);
#8472=VERTEX_POINT('',#53581);
#8473=VERTEX_POINT('',#53608);
#8474=VERTEX_POINT('',#53610);
#8475=VERTEX_POINT('',#53640);
#8476=VERTEX_POINT('',#53642);
#8477=VERTEX_POINT('',#53671);
#8478=VERTEX_POINT('',#53673);
#8479=VERTEX_POINT('',#53708);
#8480=VERTEX_POINT('',#53710);
#8481=VERTEX_POINT('',#53740);
#8482=VERTEX_POINT('',#53742);
#8483=VERTEX_POINT('',#53777);
#8484=VERTEX_POINT('',#53779);
#8485=VERTEX_POINT('',#53809);
#8486=VERTEX_POINT('',#53811);
#8487=VERTEX_POINT('',#53846);
#8488=VERTEX_POINT('',#53848);
#8489=VERTEX_POINT('',#53878);
#8490=VERTEX_POINT('',#53880);
#8491=VERTEX_POINT('',#53915);
#8492=VERTEX_POINT('',#53917);
#8493=VERTEX_POINT('',#53947);
#8494=VERTEX_POINT('',#53949);
#8495=VERTEX_POINT('',#53984);
#8496=VERTEX_POINT('',#53986);
#8497=VERTEX_POINT('',#54016);
#8498=VERTEX_POINT('',#54018);
#8499=VERTEX_POINT('',#54053);
#8500=VERTEX_POINT('',#54055);
#8501=VERTEX_POINT('',#54085);
#8502=VERTEX_POINT('',#54087);
#8503=VERTEX_POINT('',#54122);
#8504=VERTEX_POINT('',#54124);
#8505=VERTEX_POINT('',#54154);
#8506=VERTEX_POINT('',#54156);
#8507=VERTEX_POINT('',#54191);
#8508=VERTEX_POINT('',#54193);
#8509=VERTEX_POINT('',#54223);
#8510=VERTEX_POINT('',#54225);
#8511=VERTEX_POINT('',#54260);
#8512=VERTEX_POINT('',#54262);
#8513=VERTEX_POINT('',#54292);
#8514=VERTEX_POINT('',#54294);
#8515=VERTEX_POINT('',#54329);
#8516=VERTEX_POINT('',#54331);
#8517=VERTEX_POINT('',#54361);
#8518=VERTEX_POINT('',#54363);
#8519=VERTEX_POINT('',#54398);
#8520=VERTEX_POINT('',#54400);
#8521=VERTEX_POINT('',#54430);
#8522=VERTEX_POINT('',#54432);
#8523=VERTEX_POINT('',#54467);
#8524=VERTEX_POINT('',#54499);
#8525=VERTEX_POINT('',#54675);
#8526=VERTEX_POINT('',#54771);
#8527=VERTEX_POINT('',#54867);
#8528=VERTEX_POINT('',#54879);
#8529=VERTEX_POINT('',#55061);
#8530=VERTEX_POINT('',#55157);
#8531=VERTEX_POINT('',#55253);
#8532=VERTEX_POINT('',#55265);
#8533=VERTEX_POINT('',#55441);
#8534=VERTEX_POINT('',#55537);
#8535=VERTEX_POINT('',#55633);
#8536=VERTEX_POINT('',#55648);
#8537=VERTEX_POINT('',#55824);
#8538=VERTEX_POINT('',#55920);
#8539=VERTEX_POINT('',#56016);
#8540=VERTEX_POINT('',#56028);
#8541=VERTEX_POINT('',#56204);
#8542=VERTEX_POINT('',#56300);
#8543=VERTEX_POINT('',#56396);
#8544=VERTEX_POINT('',#56414);
#8545=VERTEX_POINT('',#56590);
#8546=VERTEX_POINT('',#56686);
#8547=VERTEX_POINT('',#56860);
#8548=VERTEX_POINT('',#56866);
#8549=VERTEX_POINT('',#56959);
#8550=VERTEX_POINT('',#56970);
#8551=VERTEX_POINT('',#56986);
#8552=VERTEX_POINT('',#56993);
#8553=VERTEX_POINT('',#57084);
#8554=VERTEX_POINT('',#57090);
#8555=VERTEX_POINT('',#57184);
#8556=VERTEX_POINT('',#57191);
#8557=VERTEX_POINT('',#57282);
#8558=VERTEX_POINT('',#57288);
#8559=VERTEX_POINT('',#57382);
#8560=VERTEX_POINT('',#57389);
#8561=VERTEX_POINT('',#57480);
#8562=VERTEX_POINT('',#57486);
#8563=VERTEX_POINT('',#57580);
#8564=VERTEX_POINT('',#57587);
#8565=VERTEX_POINT('',#57678);
#8566=VERTEX_POINT('',#57684);
#8567=VERTEX_POINT('',#57778);
#8568=VERTEX_POINT('',#57785);
#8569=VERTEX_POINT('',#57876);
#8570=VERTEX_POINT('',#57882);
#8571=VERTEX_POINT('',#57976);
#8572=VERTEX_POINT('',#57989);
#8573=VERTEX_POINT('',#58086);
#8574=VERTEX_POINT('',#58094);
#8575=VERTEX_POINT('',#58201);
#8576=VERTEX_POINT('',#58208);
#8577=VERTEX_POINT('',#58299);
#8578=VERTEX_POINT('',#58305);
#8579=VERTEX_POINT('',#58399);
#8580=VERTEX_POINT('',#58406);
#8581=VERTEX_POINT('',#58497);
#8582=VERTEX_POINT('',#58503);
#8583=VERTEX_POINT('',#58597);
#8584=VERTEX_POINT('',#58604);
#8585=VERTEX_POINT('',#58695);
#8586=VERTEX_POINT('',#58701);
#8587=VERTEX_POINT('',#58795);
#8588=VERTEX_POINT('',#58802);
#8589=VERTEX_POINT('',#58893);
#8590=VERTEX_POINT('',#58899);
#8591=VERTEX_POINT('',#58993);
#8592=VERTEX_POINT('',#59000);
#8593=VERTEX_POINT('',#59091);
#8594=VERTEX_POINT('',#59097);
#8595=VERTEX_POINT('',#59191);
#8596=VERTEX_POINT('',#59204);
#8597=VERTEX_POINT('',#59301);
#8598=VERTEX_POINT('',#59311);
#8599=VERTEX_POINT('',#59405);
#8600=VERTEX_POINT('',#59418);
#8601=VERTEX_POINT('',#59515);
#8602=VERTEX_POINT('',#59521);
#8603=VERTEX_POINT('',#59615);
#8604=VERTEX_POINT('',#59622);
#8605=VERTEX_POINT('',#59713);
#8606=VERTEX_POINT('',#59719);
#8607=VERTEX_POINT('',#59813);
#8608=VERTEX_POINT('',#59820);
#8609=VERTEX_POINT('',#59911);
#8610=VERTEX_POINT('',#59917);
#8611=VERTEX_POINT('',#60011);
#8612=VERTEX_POINT('',#60018);
#8613=VERTEX_POINT('',#60109);
#8614=VERTEX_POINT('',#60115);
#8615=VERTEX_POINT('',#60209);
#8616=VERTEX_POINT('',#60216);
#8617=VERTEX_POINT('',#60307);
#8618=VERTEX_POINT('',#60313);
#8619=VERTEX_POINT('',#60407);
#8620=VERTEX_POINT('',#60420);
#8621=VERTEX_POINT('',#60517);
#8622=VERTEX_POINT('',#60525);
#8623=VERTEX_POINT('',#60619);
#8624=VERTEX_POINT('',#60632);
#8625=VERTEX_POINT('',#60729);
#8626=VERTEX_POINT('',#60735);
#8627=VERTEX_POINT('',#60829);
#8628=VERTEX_POINT('',#60836);
#8629=VERTEX_POINT('',#60927);
#8630=VERTEX_POINT('',#60933);
#8631=VERTEX_POINT('',#61027);
#8632=VERTEX_POINT('',#61034);
#8633=VERTEX_POINT('',#61125);
#8634=VERTEX_POINT('',#61131);
#8635=VERTEX_POINT('',#61225);
#8636=VERTEX_POINT('',#61232);
#8637=VERTEX_POINT('',#61323);
#8638=VERTEX_POINT('',#61329);
#8639=VERTEX_POINT('',#61423);
#8640=VERTEX_POINT('',#61430);
#8641=VERTEX_POINT('',#61521);
#8642=VERTEX_POINT('',#61527);
#8643=VERTEX_POINT('',#61621);
#8644=VERTEX_POINT('',#61628);
#8645=VERTEX_POINT('',#61719);
#8646=VERTEX_POINT('',#61725);
#8647=VERTEX_POINT('',#61828);
#8648=VERTEX_POINT('',#61830);
#8649=VERTEX_POINT('',#61832);
#8650=VERTEX_POINT('',#61836);
#8651=VERTEX_POINT('',#61838);
#8652=VERTEX_POINT('',#61843);
#8653=VERTEX_POINT('',#61845);
#8654=VERTEX_POINT('',#61849);
#8655=VERTEX_POINT('',#61851);
#8656=VERTEX_POINT('',#61855);
#8657=VERTEX_POINT('',#61857);
#8658=VERTEX_POINT('',#61861);
#8659=VERTEX_POINT('',#61863);
#8660=VERTEX_POINT('',#61867);
#8661=VERTEX_POINT('',#61873);
#8662=VERTEX_POINT('',#61874);
#8663=VERTEX_POINT('',#61876);
#8664=VERTEX_POINT('',#61878);
#8665=VERTEX_POINT('',#61882);
#8666=VERTEX_POINT('',#61883);
#8667=VERTEX_POINT('',#61888);
#8668=VERTEX_POINT('',#61889);
#8669=VERTEX_POINT('',#61897);
#8670=VERTEX_POINT('',#61899);
#8671=VERTEX_POINT('',#61903);
#8672=VERTEX_POINT('',#61907);
#8673=VERTEX_POINT('',#61910);
#8674=VERTEX_POINT('',#61912);
#8675=VERTEX_POINT('',#61916);
#8676=VERTEX_POINT('',#61917);
#8677=VERTEX_POINT('',#61922);
#8678=VERTEX_POINT('',#61931);
#8679=VERTEX_POINT('',#61934);
#8680=VERTEX_POINT('',#61938);
#8681=VERTEX_POINT('',#61940);
#8682=VERTEX_POINT('',#61948);
#8683=VERTEX_POINT('',#61950);
#8684=VERTEX_POINT('',#61952);
#8685=VERTEX_POINT('',#61956);
#8686=VERTEX_POINT('',#61958);
#8687=VERTEX_POINT('',#61963);
#8688=VERTEX_POINT('',#61965);
#8689=VERTEX_POINT('',#61969);
#8690=VERTEX_POINT('',#61971);
#8691=VERTEX_POINT('',#61975);
#8692=VERTEX_POINT('',#61977);
#8693=VERTEX_POINT('',#61981);
#8694=VERTEX_POINT('',#61983);
#8695=VERTEX_POINT('',#61987);
#8696=VERTEX_POINT('',#61993);
#8697=VERTEX_POINT('',#61995);
#8698=VERTEX_POINT('',#62002);
#8699=VERTEX_POINT('',#62003);
#8700=VERTEX_POINT('',#62019);
#8701=VERTEX_POINT('',#62021);
#8702=VERTEX_POINT('',#62023);
#8703=VERTEX_POINT('',#62025);
#8704=VERTEX_POINT('',#62029);
#8705=VERTEX_POINT('',#62030);
#8706=VERTEX_POINT('',#62033);
#8707=VERTEX_POINT('',#62037);
#8708=VERTEX_POINT('',#62038);
#8709=VERTEX_POINT('',#62040);
#8710=VERTEX_POINT('',#62047);
#8711=VERTEX_POINT('',#62048);
#8712=VERTEX_POINT('',#62053);
#8713=VERTEX_POINT('',#62057);
#8714=VERTEX_POINT('',#62058);
#8715=VERTEX_POINT('',#62060);
#8716=VERTEX_POINT('',#62069);
#8717=VERTEX_POINT('',#62071);
#8718=VERTEX_POINT('',#62073);
#8719=VERTEX_POINT('',#62083);
#8720=VERTEX_POINT('',#62085);
#8721=VERTEX_POINT('',#62089);
#8722=VERTEX_POINT('',#62099);
#8723=VERTEX_POINT('',#62103);
#8724=VERTEX_POINT('',#62104);
#8725=VERTEX_POINT('',#62120);
#8726=VERTEX_POINT('',#62122);
#8727=VERTEX_POINT('',#62124);
#8728=VERTEX_POINT('',#62126);
#8729=VERTEX_POINT('',#62130);
#8730=VERTEX_POINT('',#62131);
#8731=VERTEX_POINT('',#62133);
#8732=VERTEX_POINT('',#62135);
#8733=VERTEX_POINT('',#62139);
#8734=VERTEX_POINT('',#62143);
#8735=VERTEX_POINT('',#62144);
#8736=VERTEX_POINT('',#62147);
#8737=VERTEX_POINT('',#62151);
#8738=VERTEX_POINT('',#62160);
#8739=VERTEX_POINT('',#62162);
#8740=VERTEX_POINT('',#62164);
#8741=VERTEX_POINT('',#62173);
#8742=VERTEX_POINT('',#62174);
#8743=VERTEX_POINT('',#62176);
#8744=VERTEX_POINT('',#62180);
#8745=VERTEX_POINT('',#62181);
#8746=VERTEX_POINT('',#62186);
#8747=VERTEX_POINT('',#62199);
#8748=VERTEX_POINT('',#62201);
#8749=VERTEX_POINT('',#62205);
#8750=VERTEX_POINT('',#62206);
#8751=VERTEX_POINT('',#62208);
#8752=VERTEX_POINT('',#62210);
#8753=VERTEX_POINT('',#62214);
#8754=VERTEX_POINT('',#62218);
#8755=VERTEX_POINT('',#62222);
#8756=VERTEX_POINT('',#62224);
#8757=VERTEX_POINT('',#62228);
#8758=VERTEX_POINT('',#62230);
#8759=VERTEX_POINT('',#62234);
#8760=VERTEX_POINT('',#62238);
#8761=VERTEX_POINT('',#62239);
#8762=VERTEX_POINT('',#62255);
#8763=VERTEX_POINT('',#62258);
#8764=VERTEX_POINT('',#62260);
#8765=VERTEX_POINT('',#62265);
#8766=VERTEX_POINT('',#62267);
#8767=VERTEX_POINT('',#62271);
#8768=VERTEX_POINT('',#62272);
#8769=VERTEX_POINT('',#62274);
#8770=VERTEX_POINT('',#62277);
#8771=VERTEX_POINT('',#62279);
#8772=VERTEX_POINT('',#62301);
#8773=VERTEX_POINT('',#62303);
#8774=VERTEX_POINT('',#62312);
#8775=VERTEX_POINT('',#62316);
#8776=VERTEX_POINT('',#62318);
#8777=VERTEX_POINT('',#62322);
#8778=VERTEX_POINT('',#62329);
#8779=VERTEX_POINT('',#62331);
#8780=VERTEX_POINT('',#62336);
#8781=VERTEX_POINT('',#62338);
#8782=VERTEX_POINT('',#62360);
#8783=VERTEX_POINT('',#62362);
#8784=VERTEX_POINT('',#62384);
#8785=VERTEX_POINT('',#62394);
#8786=VERTEX_POINT('',#62396);
#8787=VERTEX_POINT('',#62398);
#8788=VERTEX_POINT('',#62400);
#8789=VERTEX_POINT('',#62408);
#8790=VERTEX_POINT('',#62411);
#8791=VERTEX_POINT('',#62413);
#8792=VERTEX_POINT('',#62417);
#8793=VERTEX_POINT('',#62419);
#8794=VERTEX_POINT('',#62421);
#8795=VERTEX_POINT('',#62425);
#8796=VERTEX_POINT('',#62427);
#8797=VERTEX_POINT('',#62431);
#8798=VERTEX_POINT('',#62444);
#8799=VERTEX_POINT('',#62446);
#8800=VERTEX_POINT('',#62448);
#8801=VERTEX_POINT('',#62452);
#8802=VERTEX_POINT('',#62454);
#8803=VERTEX_POINT('',#62456);
#8804=VERTEX_POINT('',#62460);
#8805=VERTEX_POINT('',#62462);
#8806=VERTEX_POINT('',#62464);
#8807=VERTEX_POINT('',#62468);
#8808=VERTEX_POINT('',#62476);
#8809=VERTEX_POINT('',#62480);
#8810=VERTEX_POINT('',#62484);
#8811=VERTEX_POINT('',#62488);
#8812=VERTEX_POINT('',#62492);
#8813=VERTEX_POINT('',#62496);
#8814=VERTEX_POINT('',#62498);
#8815=VERTEX_POINT('',#62502);
#8816=VERTEX_POINT('',#62504);
#8817=VERTEX_POINT('',#62508);
#8818=VERTEX_POINT('',#62510);
#8819=VERTEX_POINT('',#62516);
#8820=VERTEX_POINT('',#62520);
#8821=VERTEX_POINT('',#62524);
#8822=VERTEX_POINT('',#62527);
#8823=VERTEX_POINT('',#62529);
#8824=VERTEX_POINT('',#62535);
#8825=VERTEX_POINT('',#62537);
#8826=VERTEX_POINT('',#62541);
#8827=VERTEX_POINT('',#62559);
#8828=VERTEX_POINT('',#62561);
#8829=VERTEX_POINT('',#62565);
#8830=VERTEX_POINT('',#62566);
#8831=VERTEX_POINT('',#62571);
#8832=VERTEX_POINT('',#62575);
#8833=VERTEX_POINT('',#62587);
#8834=VERTEX_POINT('',#62588);
#8835=VERTEX_POINT('',#62590);
#8836=VERTEX_POINT('',#62594);
#8837=VERTEX_POINT('',#62595);
#8838=VERTEX_POINT('',#62597);
#8839=VERTEX_POINT('',#62601);
#8840=VERTEX_POINT('',#62602);
#8841=VERTEX_POINT('',#62604);
#8842=VERTEX_POINT('',#62608);
#8843=VERTEX_POINT('',#62609);
#8844=VERTEX_POINT('',#62611);
#8845=VERTEX_POINT('',#62618);
#8846=VERTEX_POINT('',#62619);
#8847=VERTEX_POINT('',#62621);
#8848=VERTEX_POINT('',#62625);
#8849=VERTEX_POINT('',#62626);
#8850=VERTEX_POINT('',#62628);
#8851=VERTEX_POINT('',#62635);
#8852=VERTEX_POINT('',#62636);
#8853=VERTEX_POINT('',#62638);
#8854=VERTEX_POINT('',#62648);
#8855=VERTEX_POINT('',#62649);
#8856=VERTEX_POINT('',#62651);
#8857=VERTEX_POINT('',#63445);
#8858=VERTEX_POINT('',#63447);
#8859=VERTEX_POINT('',#63529);
#8860=VERTEX_POINT('',#63531);
#8861=VERTEX_POINT('',#63533);
#8862=VERTEX_POINT('',#63537);
#8863=VERTEX_POINT('',#63538);
#8864=VERTEX_POINT('',#63543);
#8865=VERTEX_POINT('',#63544);
#8866=VERTEX_POINT('',#63546);
#8867=VERTEX_POINT('',#63548);
#8868=VERTEX_POINT('',#63550);
#8869=VERTEX_POINT('',#63552);
#8870=VERTEX_POINT('',#63554);
#8871=VERTEX_POINT('',#63556);
#8872=VERTEX_POINT('',#63558);
#8873=VERTEX_POINT('',#63560);
#8874=VERTEX_POINT('',#63562);
#8875=VERTEX_POINT('',#63564);
#8876=VERTEX_POINT('',#63566);
#8877=VERTEX_POINT('',#63568);
#8878=VERTEX_POINT('',#63570);
#8879=VERTEX_POINT('',#63572);
#8880=VERTEX_POINT('',#63574);
#8881=VERTEX_POINT('',#63576);
#8882=VERTEX_POINT('',#63578);
#8883=VERTEX_POINT('',#63580);
#8884=VERTEX_POINT('',#63582);
#8885=VERTEX_POINT('',#63584);
#8886=VERTEX_POINT('',#63586);
#8887=VERTEX_POINT('',#63588);
#8888=VERTEX_POINT('',#63590);
#8889=VERTEX_POINT('',#63594);
#8890=VERTEX_POINT('',#63598);
#8891=VERTEX_POINT('',#63599);
#8892=VERTEX_POINT('',#63601);
#8893=VERTEX_POINT('',#63603);
#8894=VERTEX_POINT('',#63605);
#8895=VERTEX_POINT('',#63607);
#8896=VERTEX_POINT('',#63609);
#8897=VERTEX_POINT('',#63611);
#8898=VERTEX_POINT('',#63613);
#8899=VERTEX_POINT('',#63615);
#8900=VERTEX_POINT('',#63617);
#8901=VERTEX_POINT('',#63619);
#8902=VERTEX_POINT('',#63621);
#8903=VERTEX_POINT('',#63623);
#8904=VERTEX_POINT('',#63625);
#8905=VERTEX_POINT('',#63627);
#8906=VERTEX_POINT('',#63629);
#8907=VERTEX_POINT('',#63631);
#8908=VERTEX_POINT('',#63635);
#8909=VERTEX_POINT('',#63637);
#8910=VERTEX_POINT('',#63641);
#8911=VERTEX_POINT('',#63643);
#8912=VERTEX_POINT('',#63650);
#8913=VERTEX_POINT('',#63652);
#8914=VERTEX_POINT('',#63656);
#8915=VERTEX_POINT('',#63658);
#8916=VERTEX_POINT('',#63665);
#8917=VERTEX_POINT('',#63667);
#8918=VERTEX_POINT('',#63671);
#8919=VERTEX_POINT('',#63673);
#8920=VERTEX_POINT('',#63680);
#8921=VERTEX_POINT('',#63681);
#8922=VERTEX_POINT('',#63683);
#8923=VERTEX_POINT('',#63685);
#8924=VERTEX_POINT('',#63689);
#8925=VERTEX_POINT('',#63693);
#8926=VERTEX_POINT('',#63695);
#8927=VERTEX_POINT('',#63697);
#8928=VERTEX_POINT('',#63701);
#8929=VERTEX_POINT('',#63707);
#8930=VERTEX_POINT('',#63709);
#8931=VERTEX_POINT('',#63736);
#8932=VERTEX_POINT('',#63741);
#8933=VERTEX_POINT('',#63748);
#8934=VERTEX_POINT('',#63778);
#8935=VERTEX_POINT('',#63785);
#8936=VERTEX_POINT('',#63787);
#8937=VERTEX_POINT('',#63792);
#8938=VERTEX_POINT('',#63796);
#8939=VERTEX_POINT('',#63797);
#8940=VERTEX_POINT('',#63812);
#8941=VERTEX_POINT('',#63821);
#8942=VERTEX_POINT('',#63825);
#8943=VERTEX_POINT('',#63826);
#8944=VERTEX_POINT('',#63828);
#8945=VERTEX_POINT('',#63830);
#8946=VERTEX_POINT('',#63832);
#8947=VERTEX_POINT('',#63834);
#8948=VERTEX_POINT('',#63836);
#8949=VERTEX_POINT('',#63838);
#8950=VERTEX_POINT('',#63840);
#8951=VERTEX_POINT('',#63842);
#8952=VERTEX_POINT('',#63844);
#8953=VERTEX_POINT('',#63846);
#8954=VERTEX_POINT('',#63848);
#8955=VERTEX_POINT('',#63850);
#8956=VERTEX_POINT('',#63852);
#8957=VERTEX_POINT('',#63854);
#8958=VERTEX_POINT('',#63860);
#8959=VERTEX_POINT('',#63861);
#8960=VERTEX_POINT('',#63863);
#8961=VERTEX_POINT('',#63881);
#8962=VERTEX_POINT('',#63885);
#8963=VERTEX_POINT('',#63886);
#8964=VERTEX_POINT('',#63888);
#8965=VERTEX_POINT('',#63924);
#8966=VERTEX_POINT('',#63928);
#8967=VERTEX_POINT('',#63935);
#8968=VERTEX_POINT('',#63939);
#8969=VERTEX_POINT('',#63956);
#8970=VERTEX_POINT('',#63958);
#8971=VERTEX_POINT('',#63960);
#8972=VERTEX_POINT('',#63964);
#8973=VERTEX_POINT('',#63965);
#8974=VERTEX_POINT('',#63967);
#8975=VERTEX_POINT('',#63971);
#8976=VERTEX_POINT('',#63973);
#8977=VERTEX_POINT('',#63977);
#8978=VERTEX_POINT('',#63981);
#8979=VERTEX_POINT('',#63985);
#8980=VERTEX_POINT('',#63986);
#8981=VERTEX_POINT('',#63988);
#8982=VERTEX_POINT('',#64056);
#8983=VERTEX_POINT('',#64071);
#8984=VERTEX_POINT('',#64077);
#8985=VERTEX_POINT('',#64079);
#8986=VERTEX_POINT('',#64086);
#8987=VERTEX_POINT('',#64090);
#8988=VERTEX_POINT('',#64107);
#8989=VERTEX_POINT('',#64109);
#8990=VERTEX_POINT('',#64115);
#8991=VERTEX_POINT('',#64119);
#8992=VERTEX_POINT('',#64121);
#8993=VERTEX_POINT('',#64136);
#8994=VERTEX_POINT('',#64138);
#8995=VERTEX_POINT('',#64145);
#8996=VERTEX_POINT('',#64164);
#8997=VERTEX_POINT('',#64191);
#8998=VERTEX_POINT('',#64199);
#8999=VERTEX_POINT('',#64201);
#9000=VERTEX_POINT('',#64221);
#9001=VERTEX_POINT('',#64223);
#9002=VERTEX_POINT('',#64225);
#9003=VERTEX_POINT('',#64232);
#9004=VERTEX_POINT('',#64236);
#9005=VERTEX_POINT('',#64240);
#9006=VERTEX_POINT('',#64244);
#9007=VERTEX_POINT('',#64248);
#9008=VERTEX_POINT('',#64265);
#9009=VERTEX_POINT('',#64267);
#9010=VERTEX_POINT('',#64269);
#9011=VERTEX_POINT('',#64273);
#9012=VERTEX_POINT('',#64274);
#9013=VERTEX_POINT('',#64287);
#9014=VERTEX_POINT('',#64289);
#9015=VERTEX_POINT('',#64311);
#9016=VERTEX_POINT('',#64315);
#9017=VERTEX_POINT('',#64317);
#9018=VERTEX_POINT('',#64332);
#9019=VERTEX_POINT('',#64353);
#9020=VERTEX_POINT('',#64368);
#9021=VERTEX_POINT('',#64370);
#9022=VERTEX_POINT('',#64372);
#9023=VERTEX_POINT('',#64375);
#9024=VERTEX_POINT('',#64377);
#9025=VERTEX_POINT('',#64380);
#9026=VERTEX_POINT('',#64382);
#9027=VERTEX_POINT('',#64387);
#9028=VERTEX_POINT('',#64389);
#9029=VERTEX_POINT('',#64392);
#9030=VERTEX_POINT('',#64394);
#9031=VERTEX_POINT('',#64396);
#9032=VERTEX_POINT('',#64399);
#9033=VERTEX_POINT('',#64401);
#9034=VERTEX_POINT('',#64404);
#9035=VERTEX_POINT('',#64408);
#9036=VERTEX_POINT('',#64423);
#9037=VERTEX_POINT('',#64436);
#9038=VERTEX_POINT('',#64441);
#9039=VERTEX_POINT('',#64448);
#9040=VERTEX_POINT('',#64450);
#9041=VERTEX_POINT('',#64454);
#9042=VERTEX_POINT('',#64469);
#9043=VERTEX_POINT('',#64482);
#9044=VERTEX_POINT('',#64487);
#9045=VERTEX_POINT('',#64494);
#9046=VERTEX_POINT('',#64496);
#9047=VERTEX_POINT('',#64513);
#9048=VERTEX_POINT('',#64515);
#9049=VERTEX_POINT('',#64517);
#9050=VERTEX_POINT('',#64535);
#9051=VERTEX_POINT('',#64539);
#9052=VERTEX_POINT('',#64565);
#9053=VERTEX_POINT('',#64567);
#9054=VERTEX_POINT('',#64600);
#9055=VERTEX_POINT('',#64604);
#9056=VERTEX_POINT('',#64619);
#9057=VERTEX_POINT('',#64621);
#9058=VERTEX_POINT('',#64640);
#9059=VERTEX_POINT('',#64655);
#9060=VERTEX_POINT('',#64660);
#9061=VERTEX_POINT('',#64662);
#9062=VERTEX_POINT('',#64664);
#9063=VERTEX_POINT('',#64726);
#9064=VERTEX_POINT('',#64730);
#9065=VERTEX_POINT('',#64737);
#9066=VERTEX_POINT('',#64739);
#9067=VERTEX_POINT('',#64752);
#9068=VERTEX_POINT('',#64753);
#9069=VERTEX_POINT('',#64772);
#9070=VERTEX_POINT('',#64776);
#9071=VERTEX_POINT('',#64777);
#9072=VERTEX_POINT('',#64782);
#9073=VERTEX_POINT('',#64783);
#9074=VERTEX_POINT('',#64787);
#9075=VERTEX_POINT('',#64790);
#9076=VERTEX_POINT('',#64792);
#9077=VERTEX_POINT('',#64796);
#9078=VERTEX_POINT('',#64801);
#9079=VERTEX_POINT('',#64806);
#9080=VERTEX_POINT('',#64811);
#9081=VERTEX_POINT('',#64815);
#9082=VERTEX_POINT('',#64817);
#9083=VERTEX_POINT('',#64828);
#9084=VERTEX_POINT('',#64830);
#9085=VERTEX_POINT('',#64841);
#9086=VERTEX_POINT('',#64849);
#9087=VERTEX_POINT('',#64915);
#9088=VERTEX_POINT('',#64917);
#9089=VERTEX_POINT('',#64928);
#9090=VERTEX_POINT('',#64936);
#9091=VERTEX_POINT('',#65002);
#9092=VERTEX_POINT('',#65004);
#9093=VERTEX_POINT('',#65015);
#9094=VERTEX_POINT('',#65023);
#9095=VERTEX_POINT('',#65087);
#9096=VERTEX_POINT('',#65088);
#9097=VERTEX_POINT('',#65095);
#9098=VERTEX_POINT('',#65097);
#9099=VERTEX_POINT('',#65099);
#9100=VERTEX_POINT('',#65103);
#9101=VERTEX_POINT('',#65143);
#9102=VERTEX_POINT('',#65212);
#9103=VERTEX_POINT('',#65221);
#9104=VERTEX_POINT('',#65225);
#9105=VERTEX_POINT('',#65304);
#9106=VERTEX_POINT('',#65373);
#9107=VERTEX_POINT('',#65374);
#9108=VERTEX_POINT('',#65376);
#9109=VERTEX_POINT('',#65378);
#9110=VERTEX_POINT('',#65382);
#9111=VERTEX_POINT('',#65393);
#9112=VERTEX_POINT('',#65397);
#9113=VERTEX_POINT('',#65404);
#9114=VERTEX_POINT('',#65406);
#9115=VERTEX_POINT('',#65417);
#9116=VERTEX_POINT('',#65419);
#9117=VERTEX_POINT('',#65421);
#9118=VERTEX_POINT('',#65427);
#9119=VERTEX_POINT('',#65429);
#9120=VERTEX_POINT('',#65433);
#9121=VERTEX_POINT('',#65438);
#9122=VERTEX_POINT('',#65458);
#9123=VERTEX_POINT('',#65460);
#9124=VERTEX_POINT('',#65463);
#9125=VERTEX_POINT('',#65465);
#9126=VERTEX_POINT('',#65470);
#9127=EDGE_CURVE('',#7226,#7227,#5442,.T.);
#9128=EDGE_CURVE('',#7226,#7228,#4669,.T.);
#9129=EDGE_CURVE('',#7228,#7229,#3542,.T.);
#9130=EDGE_CURVE('',#7229,#7230,#5443,.T.);
#9131=EDGE_CURVE('',#7230,#7231,#3543,.T.);
#9132=EDGE_CURVE('',#7231,#7232,#5444,.T.);
#9133=EDGE_CURVE('',#7232,#7233,#3544,.T.);
#9134=EDGE_CURVE('',#7233,#7234,#5445,.T.);
#9135=EDGE_CURVE('',#7234,#7234,#3545,.F.);
#9136=EDGE_CURVE('',#7233,#7235,#3546,.T.);
#9137=EDGE_CURVE('',#7235,#7236,#5446,.T.);
#9138=EDGE_CURVE('',#7236,#7230,#3547,.T.);
#9139=EDGE_CURVE('',#7229,#7237,#3548,.T.);
#9140=EDGE_CURVE('',#7237,#7227,#4670,.T.);
#9141=EDGE_CURVE('',#7238,#7239,#5447,.T.);
#9142=EDGE_CURVE('',#7239,#7240,#3549,.T.);
#9143=EDGE_CURVE('',#7240,#7241,#5448,.T.);
#9144=EDGE_CURVE('',#7241,#7238,#3550,.T.);
#9145=EDGE_CURVE('',#7242,#7243,#5449,.T.);
#9146=EDGE_CURVE('',#7242,#7226,#4671,.T.);
#9147=EDGE_CURVE('',#7227,#7243,#4672,.T.);
#9148=EDGE_CURVE('',#7244,#7245,#5450,.T.);
#9149=EDGE_CURVE('',#7244,#7242,#4673,.T.);
#9150=EDGE_CURVE('',#7243,#7245,#4674,.T.);
#9151=EDGE_CURVE('',#7246,#7247,#5451,.T.);
#9152=EDGE_CURVE('',#7246,#7244,#4675,.T.);
#9153=EDGE_CURVE('',#7245,#7247,#4676,.T.);
#9154=EDGE_CURVE('',#7248,#7249,#5452,.T.);
#9155=EDGE_CURVE('',#7248,#7246,#4677,.T.);
#9156=EDGE_CURVE('',#7247,#7249,#4678,.T.);
#9157=EDGE_CURVE('',#7250,#7251,#5453,.T.);
#9158=EDGE_CURVE('',#7250,#7248,#4679,.T.);
#9159=EDGE_CURVE('',#7249,#7251,#4680,.T.);
#9160=EDGE_CURVE('',#7252,#7253,#5454,.T.);
#9161=EDGE_CURVE('',#7252,#7250,#4681,.T.);
#9162=EDGE_CURVE('',#7251,#7253,#4682,.T.);
#9163=EDGE_CURVE('',#7254,#7255,#5455,.T.);
#9164=EDGE_CURVE('',#7254,#7252,#4683,.T.);
#9165=EDGE_CURVE('',#7253,#7255,#4684,.T.);
#9166=EDGE_CURVE('',#7256,#7257,#5456,.T.);
#9167=EDGE_CURVE('',#7256,#7254,#4685,.T.);
#9168=EDGE_CURVE('',#7255,#7257,#4686,.T.);
#9169=EDGE_CURVE('',#7258,#7259,#5457,.T.);
#9170=EDGE_CURVE('',#7258,#7256,#4687,.T.);
#9171=EDGE_CURVE('',#7257,#7259,#4688,.T.);
#9172=EDGE_CURVE('',#7260,#7261,#5458,.T.);
#9173=EDGE_CURVE('',#7260,#7258,#4689,.T.);
#9174=EDGE_CURVE('',#7259,#7261,#4690,.T.);
#9175=EDGE_CURVE('',#7262,#7263,#5459,.T.);
#9176=EDGE_CURVE('',#7262,#7260,#4691,.T.);
#9177=EDGE_CURVE('',#7261,#7263,#4692,.T.);
#9178=EDGE_CURVE('',#7264,#7265,#5460,.T.);
#9179=EDGE_CURVE('',#7264,#7262,#4693,.T.);
#9180=EDGE_CURVE('',#7263,#7265,#4694,.T.);
#9181=EDGE_CURVE('',#7266,#7267,#5461,.T.);
#9182=EDGE_CURVE('',#7266,#7264,#4695,.T.);
#9183=EDGE_CURVE('',#7265,#7267,#4696,.T.);
#9184=EDGE_CURVE('',#7268,#7269,#5462,.T.);
#9185=EDGE_CURVE('',#7268,#7266,#4697,.T.);
#9186=EDGE_CURVE('',#7267,#7269,#4698,.T.);
#9187=EDGE_CURVE('',#7270,#7271,#5463,.T.);
#9188=EDGE_CURVE('',#7270,#7268,#4699,.T.);
#9189=EDGE_CURVE('',#7269,#7271,#4700,.T.);
#9190=EDGE_CURVE('',#7272,#7273,#5464,.T.);
#9191=EDGE_CURVE('',#7272,#7270,#4701,.T.);
#9192=EDGE_CURVE('',#7271,#7273,#4702,.T.);
#9193=EDGE_CURVE('',#7274,#7275,#5465,.T.);
#9194=EDGE_CURVE('',#7274,#7272,#4703,.T.);
#9195=EDGE_CURVE('',#7273,#7275,#4704,.T.);
#9196=EDGE_CURVE('',#7276,#7277,#5466,.T.);
#9197=EDGE_CURVE('',#7276,#7274,#4705,.T.);
#9198=EDGE_CURVE('',#7275,#7277,#4706,.T.);
#9199=EDGE_CURVE('',#7278,#7279,#5467,.T.);
#9200=EDGE_CURVE('',#7278,#7276,#4707,.T.);
#9201=EDGE_CURVE('',#7277,#7279,#4708,.T.);
#9202=EDGE_CURVE('',#7280,#7281,#5468,.T.);
#9203=EDGE_CURVE('',#7280,#7278,#4709,.T.);
#9204=EDGE_CURVE('',#7279,#7281,#4710,.T.);
#9205=EDGE_CURVE('',#7282,#7283,#5469,.T.);
#9206=EDGE_CURVE('',#7282,#7280,#4711,.T.);
#9207=EDGE_CURVE('',#7281,#7283,#4712,.T.);
#9208=EDGE_CURVE('',#7284,#7285,#5470,.T.);
#9209=EDGE_CURVE('',#7284,#7282,#4713,.T.);
#9210=EDGE_CURVE('',#7283,#7285,#4714,.T.);
#9211=EDGE_CURVE('',#7286,#7287,#5471,.T.);
#9212=EDGE_CURVE('',#7286,#7284,#4715,.T.);
#9213=EDGE_CURVE('',#7285,#7287,#4716,.T.);
#9214=EDGE_CURVE('',#7288,#7289,#5472,.T.);
#9215=EDGE_CURVE('',#7288,#7286,#4717,.T.);
#9216=EDGE_CURVE('',#7287,#7289,#4718,.T.);
#9217=EDGE_CURVE('',#7290,#7291,#5473,.T.);
#9218=EDGE_CURVE('',#7290,#7288,#4719,.T.);
#9219=EDGE_CURVE('',#7289,#7291,#4720,.T.);
#9220=EDGE_CURVE('',#7292,#7293,#5474,.T.);
#9221=EDGE_CURVE('',#7292,#7290,#4721,.T.);
#9222=EDGE_CURVE('',#7291,#7293,#4722,.T.);
#9223=EDGE_CURVE('',#7294,#7295,#5475,.T.);
#9224=EDGE_CURVE('',#7294,#7292,#4723,.T.);
#9225=EDGE_CURVE('',#7293,#7295,#4724,.T.);
#9226=EDGE_CURVE('',#7296,#7297,#5476,.T.);
#9227=EDGE_CURVE('',#7296,#7294,#4725,.T.);
#9228=EDGE_CURVE('',#7295,#7297,#4726,.T.);
#9229=EDGE_CURVE('',#7298,#7299,#5477,.T.);
#9230=EDGE_CURVE('',#7298,#7296,#4727,.T.);
#9231=EDGE_CURVE('',#7297,#7299,#4728,.T.);
#9232=EDGE_CURVE('',#7300,#7301,#5478,.T.);
#9233=EDGE_CURVE('',#7300,#7298,#4729,.T.);
#9234=EDGE_CURVE('',#7299,#7301,#4730,.T.);
#9235=EDGE_CURVE('',#7302,#7303,#5479,.T.);
#9236=EDGE_CURVE('',#7302,#7300,#4731,.T.);
#9237=EDGE_CURVE('',#7301,#7303,#4732,.T.);
#9238=EDGE_CURVE('',#7304,#7305,#5480,.T.);
#9239=EDGE_CURVE('',#7304,#7302,#4733,.T.);
#9240=EDGE_CURVE('',#7303,#7305,#4734,.T.);
#9241=EDGE_CURVE('',#7306,#7307,#5481,.T.);
#9242=EDGE_CURVE('',#7306,#7304,#4735,.T.);
#9243=EDGE_CURVE('',#7305,#7307,#4736,.T.);
#9244=EDGE_CURVE('',#7308,#7309,#5482,.T.);
#9245=EDGE_CURVE('',#7308,#7306,#4737,.T.);
#9246=EDGE_CURVE('',#7307,#7309,#4738,.T.);
#9247=EDGE_CURVE('',#7310,#7311,#5483,.T.);
#9248=EDGE_CURVE('',#7310,#7308,#4739,.T.);
#9249=EDGE_CURVE('',#7309,#7311,#4740,.T.);
#9250=EDGE_CURVE('',#7312,#7313,#5484,.T.);
#9251=EDGE_CURVE('',#7312,#7310,#4741,.T.);
#9252=EDGE_CURVE('',#7311,#7313,#4742,.T.);
#9253=EDGE_CURVE('',#7314,#7315,#5485,.T.);
#9254=EDGE_CURVE('',#7314,#7312,#4743,.T.);
#9255=EDGE_CURVE('',#7313,#7315,#4744,.T.);
#9256=EDGE_CURVE('',#7316,#7317,#5486,.T.);
#9257=EDGE_CURVE('',#7316,#7314,#4745,.T.);
#9258=EDGE_CURVE('',#7315,#7317,#4746,.T.);
#9259=EDGE_CURVE('',#7318,#7319,#5487,.T.);
#9260=EDGE_CURVE('',#7318,#7316,#4747,.T.);
#9261=EDGE_CURVE('',#7317,#7319,#4748,.T.);
#9262=EDGE_CURVE('',#7320,#7321,#5488,.T.);
#9263=EDGE_CURVE('',#7320,#7318,#4749,.T.);
#9264=EDGE_CURVE('',#7319,#7321,#4750,.T.);
#9265=EDGE_CURVE('',#7322,#7323,#5489,.T.);
#9266=EDGE_CURVE('',#7322,#7320,#4751,.T.);
#9267=EDGE_CURVE('',#7321,#7323,#4752,.T.);
#9268=EDGE_CURVE('',#7324,#7325,#5490,.T.);
#9269=EDGE_CURVE('',#7324,#7322,#4753,.T.);
#9270=EDGE_CURVE('',#7323,#7325,#4754,.T.);
#9271=EDGE_CURVE('',#7326,#7327,#5491,.T.);
#9272=EDGE_CURVE('',#7326,#7324,#4755,.T.);
#9273=EDGE_CURVE('',#7325,#7327,#4756,.T.);
#9274=EDGE_CURVE('',#7328,#7329,#5492,.T.);
#9275=EDGE_CURVE('',#7328,#7326,#4757,.T.);
#9276=EDGE_CURVE('',#7327,#7329,#4758,.T.);
#9277=EDGE_CURVE('',#7330,#7331,#5493,.T.);
#9278=EDGE_CURVE('',#7330,#7328,#4759,.T.);
#9279=EDGE_CURVE('',#7329,#7331,#4760,.T.);
#9280=EDGE_CURVE('',#7332,#7333,#5494,.T.);
#9281=EDGE_CURVE('',#7332,#7330,#4761,.T.);
#9282=EDGE_CURVE('',#7331,#7333,#4762,.T.);
#9283=EDGE_CURVE('',#7334,#7335,#5495,.T.);
#9284=EDGE_CURVE('',#7334,#7332,#4763,.T.);
#9285=EDGE_CURVE('',#7333,#7335,#4764,.T.);
#9286=EDGE_CURVE('',#7336,#7337,#5496,.T.);
#9287=EDGE_CURVE('',#7336,#7334,#4765,.T.);
#9288=EDGE_CURVE('',#7335,#7337,#4766,.T.);
#9289=EDGE_CURVE('',#7338,#7339,#5497,.T.);
#9290=EDGE_CURVE('',#7338,#7336,#4767,.T.);
#9291=EDGE_CURVE('',#7337,#7339,#4768,.T.);
#9292=EDGE_CURVE('',#7340,#7341,#5498,.T.);
#9293=EDGE_CURVE('',#7340,#7338,#4769,.T.);
#9294=EDGE_CURVE('',#7339,#7341,#4770,.T.);
#9295=EDGE_CURVE('',#7342,#7343,#5499,.T.);
#9296=EDGE_CURVE('',#7342,#7340,#4771,.T.);
#9297=EDGE_CURVE('',#7341,#7343,#4772,.T.);
#9298=EDGE_CURVE('',#7344,#7345,#5500,.T.);
#9299=EDGE_CURVE('',#7344,#7342,#4773,.T.);
#9300=EDGE_CURVE('',#7343,#7345,#4774,.T.);
#9301=EDGE_CURVE('',#7346,#7347,#5501,.T.);
#9302=EDGE_CURVE('',#7346,#7344,#4775,.T.);
#9303=EDGE_CURVE('',#7345,#7347,#4776,.T.);
#9304=EDGE_CURVE('',#7348,#7349,#5502,.T.);
#9305=EDGE_CURVE('',#7348,#7346,#4777,.T.);
#9306=EDGE_CURVE('',#7347,#7349,#4778,.T.);
#9307=EDGE_CURVE('',#7350,#7351,#5503,.T.);
#9308=EDGE_CURVE('',#7350,#7348,#4779,.T.);
#9309=EDGE_CURVE('',#7349,#7351,#4780,.T.);
#9310=EDGE_CURVE('',#7352,#7353,#5504,.T.);
#9311=EDGE_CURVE('',#7352,#7350,#4781,.T.);
#9312=EDGE_CURVE('',#7351,#7353,#4782,.T.);
#9313=EDGE_CURVE('',#7354,#7355,#5505,.T.);
#9314=EDGE_CURVE('',#7354,#7352,#4783,.T.);
#9315=EDGE_CURVE('',#7353,#7355,#4784,.T.);
#9316=EDGE_CURVE('',#7356,#7357,#5506,.T.);
#9317=EDGE_CURVE('',#7356,#7354,#4785,.T.);
#9318=EDGE_CURVE('',#7355,#7357,#4786,.T.);
#9319=EDGE_CURVE('',#7358,#7359,#5507,.T.);
#9320=EDGE_CURVE('',#7358,#7356,#4787,.T.);
#9321=EDGE_CURVE('',#7357,#7359,#4788,.T.);
#9322=EDGE_CURVE('',#7360,#7361,#5508,.T.);
#9323=EDGE_CURVE('',#7360,#7358,#4789,.T.);
#9324=EDGE_CURVE('',#7359,#7361,#4790,.T.);
#9325=EDGE_CURVE('',#7362,#7363,#5509,.T.);
#9326=EDGE_CURVE('',#7362,#7360,#4791,.T.);
#9327=EDGE_CURVE('',#7361,#7363,#4792,.T.);
#9328=EDGE_CURVE('',#7364,#7365,#5510,.T.);
#9329=EDGE_CURVE('',#7364,#7366,#4793,.T.);
#9330=EDGE_CURVE('',#7366,#7367,#3551,.T.);
#9331=EDGE_CURVE('',#7367,#7368,#5511,.T.);
#9332=EDGE_CURVE('',#7368,#7368,#3552,.T.);
#9333=EDGE_CURVE('',#7367,#7369,#3553,.T.);
#9334=EDGE_CURVE('',#7369,#7365,#4794,.T.);
#9335=EDGE_CURVE('',#7370,#7371,#5512,.T.);
#9336=EDGE_CURVE('',#7370,#7364,#4795,.T.);
#9337=EDGE_CURVE('',#7365,#7371,#4796,.T.);
#9338=EDGE_CURVE('',#7372,#7373,#5513,.T.);
#9339=EDGE_CURVE('',#7372,#7370,#4797,.T.);
#9340=EDGE_CURVE('',#7371,#7373,#4798,.T.);
#9341=EDGE_CURVE('',#7374,#7375,#5514,.T.);
#9342=EDGE_CURVE('',#7374,#7372,#4799,.T.);
#9343=EDGE_CURVE('',#7373,#7375,#4800,.T.);
#9344=EDGE_CURVE('',#7376,#7377,#5515,.T.);
#9345=EDGE_CURVE('',#7376,#7374,#4801,.T.);
#9346=EDGE_CURVE('',#7375,#7377,#4802,.T.);
#9347=EDGE_CURVE('',#7378,#7379,#5516,.T.);
#9348=EDGE_CURVE('',#7378,#7376,#4803,.T.);
#9349=EDGE_CURVE('',#7377,#7379,#4804,.T.);
#9350=EDGE_CURVE('',#7380,#7381,#5517,.T.);
#9351=EDGE_CURVE('',#7380,#7378,#4805,.T.);
#9352=EDGE_CURVE('',#7379,#7381,#4806,.T.);
#9353=EDGE_CURVE('',#7382,#7383,#5518,.T.);
#9354=EDGE_CURVE('',#7382,#7380,#4807,.T.);
#9355=EDGE_CURVE('',#7381,#7383,#4808,.T.);
#9356=EDGE_CURVE('',#7384,#7385,#5519,.T.);
#9357=EDGE_CURVE('',#7384,#7382,#4809,.T.);
#9358=EDGE_CURVE('',#7383,#7385,#4810,.T.);
#9359=EDGE_CURVE('',#7386,#7387,#5520,.T.);
#9360=EDGE_CURVE('',#7386,#7384,#4811,.T.);
#9361=EDGE_CURVE('',#7385,#7387,#4812,.T.);
#9362=EDGE_CURVE('',#7388,#7389,#5521,.T.);
#9363=EDGE_CURVE('',#7388,#7386,#4813,.T.);
#9364=EDGE_CURVE('',#7387,#7389,#4814,.T.);
#9365=EDGE_CURVE('',#7390,#7391,#5522,.T.);
#9366=EDGE_CURVE('',#7390,#7388,#4815,.T.);
#9367=EDGE_CURVE('',#7389,#7391,#4816,.T.);
#9368=EDGE_CURVE('',#7392,#7393,#5523,.T.);
#9369=EDGE_CURVE('',#7392,#7390,#4817,.T.);
#9370=EDGE_CURVE('',#7391,#7393,#4818,.T.);
#9371=EDGE_CURVE('',#7394,#7395,#5524,.T.);
#9372=EDGE_CURVE('',#7394,#7392,#4819,.T.);
#9373=EDGE_CURVE('',#7393,#7395,#4820,.T.);
#9374=EDGE_CURVE('',#7396,#7397,#5525,.T.);
#9375=EDGE_CURVE('',#7396,#7394,#4821,.T.);
#9376=EDGE_CURVE('',#7395,#7397,#4822,.T.);
#9377=EDGE_CURVE('',#7398,#7399,#5526,.T.);
#9378=EDGE_CURVE('',#7398,#7396,#4823,.T.);
#9379=EDGE_CURVE('',#7397,#7399,#4824,.T.);
#9380=EDGE_CURVE('',#7400,#7401,#5527,.T.);
#9381=EDGE_CURVE('',#7400,#7402,#4825,.T.);
#9382=EDGE_CURVE('',#7403,#7402,#3554,.T.);
#9383=EDGE_CURVE('',#7401,#7403,#4826,.T.);
#9384=EDGE_CURVE('',#7404,#7405,#5528,.T.);
#9385=EDGE_CURVE('',#7404,#7400,#4827,.T.);
#9386=EDGE_CURVE('',#7405,#7401,#4828,.T.);
#9387=EDGE_CURVE('',#7406,#7407,#5529,.T.);
#9388=EDGE_CURVE('',#7406,#7404,#4829,.T.);
#9389=EDGE_CURVE('',#7407,#7405,#4830,.T.);
#9390=EDGE_CURVE('',#7408,#7409,#5530,.T.);
#9391=EDGE_CURVE('',#7408,#7406,#4831,.T.);
#9392=EDGE_CURVE('',#7409,#7407,#4832,.T.);
#9393=EDGE_CURVE('',#7410,#7411,#5531,.T.);
#9394=EDGE_CURVE('',#7410,#7408,#4833,.T.);
#9395=EDGE_CURVE('',#7411,#7409,#4834,.T.);
#9396=EDGE_CURVE('',#7412,#7413,#5532,.T.);
#9397=EDGE_CURVE('',#7412,#7410,#4835,.T.);
#9398=EDGE_CURVE('',#7413,#7411,#4836,.T.);
#9399=EDGE_CURVE('',#7414,#7415,#5533,.T.);
#9400=EDGE_CURVE('',#7414,#7412,#4837,.T.);
#9401=EDGE_CURVE('',#7415,#7413,#4838,.T.);
#9402=EDGE_CURVE('',#7416,#7417,#5534,.T.);
#9403=EDGE_CURVE('',#7416,#7414,#4839,.T.);
#9404=EDGE_CURVE('',#7417,#7415,#4840,.T.);
#9405=EDGE_CURVE('',#7418,#7419,#5535,.T.);
#9406=EDGE_CURVE('',#7418,#7416,#4841,.T.);
#9407=EDGE_CURVE('',#7419,#7417,#4842,.T.);
#9408=EDGE_CURVE('',#7420,#7421,#5536,.T.);
#9409=EDGE_CURVE('',#7420,#7418,#4843,.T.);
#9410=EDGE_CURVE('',#7421,#7419,#4844,.T.);
#9411=EDGE_CURVE('',#7422,#7423,#5537,.T.);
#9412=EDGE_CURVE('',#7422,#7420,#4845,.T.);
#9413=EDGE_CURVE('',#7423,#7421,#4846,.T.);
#9414=EDGE_CURVE('',#7424,#7425,#5538,.T.);
#9415=EDGE_CURVE('',#7424,#7422,#4847,.T.);
#9416=EDGE_CURVE('',#7425,#7423,#4848,.T.);
#9417=EDGE_CURVE('',#7426,#7427,#5539,.T.);
#9418=EDGE_CURVE('',#7426,#7424,#4849,.T.);
#9419=EDGE_CURVE('',#7427,#7425,#4850,.T.);
#9420=EDGE_CURVE('',#7428,#7429,#5540,.T.);
#9421=EDGE_CURVE('',#7428,#7426,#4851,.T.);
#9422=EDGE_CURVE('',#7429,#7427,#4852,.T.);
#9423=EDGE_CURVE('',#7430,#7431,#5541,.T.);
#9424=EDGE_CURVE('',#7430,#7428,#4853,.T.);
#9425=EDGE_CURVE('',#7431,#7429,#4854,.T.);
#9426=EDGE_CURVE('',#7432,#7433,#5542,.T.);
#9427=EDGE_CURVE('',#7432,#7430,#4855,.T.);
#9428=EDGE_CURVE('',#7433,#7431,#4856,.T.);
#9429=EDGE_CURVE('',#7434,#7435,#5543,.T.);
#9430=EDGE_CURVE('',#7434,#7436,#4857,.T.);
#9431=EDGE_CURVE('',#7435,#7436,#3555,.T.);
#9432=EDGE_CURVE('',#7437,#7438,#5544,.T.);
#9433=EDGE_CURVE('',#7437,#7434,#4858,.T.);
#9434=EDGE_CURVE('',#7439,#7435,#3556,.T.);
#9435=EDGE_CURVE('',#7438,#7439,#4859,.T.);
#9436=EDGE_CURVE('',#7440,#7441,#5545,.T.);
#9437=EDGE_CURVE('',#7440,#7437,#4860,.T.);
#9438=EDGE_CURVE('',#7441,#7438,#4861,.T.);
#9439=EDGE_CURVE('',#7442,#7443,#5546,.T.);
#9440=EDGE_CURVE('',#7442,#7440,#4862,.T.);
#9441=EDGE_CURVE('',#7443,#7441,#4863,.T.);
#9442=EDGE_CURVE('',#7444,#7445,#5547,.T.);
#9443=EDGE_CURVE('',#7444,#7442,#4864,.T.);
#9444=EDGE_CURVE('',#7445,#7443,#4865,.T.);
#9445=EDGE_CURVE('',#7446,#7447,#5548,.T.);
#9446=EDGE_CURVE('',#7446,#7444,#4866,.T.);
#9447=EDGE_CURVE('',#7447,#7445,#4867,.T.);
#9448=EDGE_CURVE('',#7448,#7449,#5549,.T.);
#9449=EDGE_CURVE('',#7448,#7446,#4868,.T.);
#9450=EDGE_CURVE('',#7449,#7447,#4869,.T.);
#9451=EDGE_CURVE('',#7450,#7451,#5550,.T.);
#9452=EDGE_CURVE('',#7450,#7448,#4870,.T.);
#9453=EDGE_CURVE('',#7451,#7449,#4871,.T.);
#9454=EDGE_CURVE('',#7452,#7453,#5551,.T.);
#9455=EDGE_CURVE('',#7452,#7450,#4872,.T.);
#9456=EDGE_CURVE('',#7453,#7451,#4873,.T.);
#9457=EDGE_CURVE('',#7454,#7455,#5552,.T.);
#9458=EDGE_CURVE('',#7454,#7452,#4874,.T.);
#9459=EDGE_CURVE('',#7455,#7453,#4875,.T.);
#9460=EDGE_CURVE('',#7456,#7457,#5553,.T.);
#9461=EDGE_CURVE('',#7456,#7454,#4876,.T.);
#9462=EDGE_CURVE('',#7457,#7455,#4877,.T.);
#9463=EDGE_CURVE('',#7458,#7459,#5554,.T.);
#9464=EDGE_CURVE('',#7458,#7456,#4878,.T.);
#9465=EDGE_CURVE('',#7459,#7457,#4879,.T.);
#9466=EDGE_CURVE('',#7460,#7461,#5555,.T.);
#9467=EDGE_CURVE('',#7460,#7458,#4880,.T.);
#9468=EDGE_CURVE('',#7461,#7459,#4881,.T.);
#9469=EDGE_CURVE('',#7462,#7463,#5556,.T.);
#9470=EDGE_CURVE('',#7462,#7460,#4882,.T.);
#9471=EDGE_CURVE('',#7463,#7461,#4883,.T.);
#9472=EDGE_CURVE('',#7464,#7465,#5557,.T.);
#9473=EDGE_CURVE('',#7464,#7462,#4884,.T.);
#9474=EDGE_CURVE('',#7465,#7463,#4885,.T.);
#9475=EDGE_CURVE('',#7466,#7467,#5558,.T.);
#9476=EDGE_CURVE('',#7466,#7464,#4886,.T.);
#9477=EDGE_CURVE('',#7467,#7465,#4887,.T.);
#9478=EDGE_CURVE('',#7468,#7469,#5559,.T.);
#9479=EDGE_CURVE('',#7468,#7466,#4888,.T.);
#9480=EDGE_CURVE('',#7469,#7467,#4889,.T.);
#9481=EDGE_CURVE('',#7470,#7471,#5560,.T.);
#9482=EDGE_CURVE('',#7470,#7468,#4890,.T.);
#9483=EDGE_CURVE('',#7471,#7469,#4891,.T.);
#9484=EDGE_CURVE('',#7472,#7473,#5561,.T.);
#9485=EDGE_CURVE('',#7472,#7470,#4892,.T.);
#9486=EDGE_CURVE('',#7473,#7471,#4893,.T.);
#9487=EDGE_CURVE('',#7474,#7475,#5562,.T.);
#9488=EDGE_CURVE('',#7474,#7472,#4894,.T.);
#9489=EDGE_CURVE('',#7475,#7473,#4895,.T.);
#9490=EDGE_CURVE('',#7476,#7477,#5563,.T.);
#9491=EDGE_CURVE('',#7476,#7474,#4896,.T.);
#9492=EDGE_CURVE('',#7477,#7475,#4897,.T.);
#9493=EDGE_CURVE('',#7478,#7479,#5564,.T.);
#9494=EDGE_CURVE('',#7478,#7476,#4898,.T.);
#9495=EDGE_CURVE('',#7479,#7477,#4899,.T.);
#9496=EDGE_CURVE('',#7480,#7481,#5565,.T.);
#9497=EDGE_CURVE('',#7480,#7478,#4900,.T.);
#9498=EDGE_CURVE('',#7481,#7479,#4901,.T.);
#9499=EDGE_CURVE('',#7482,#7483,#5566,.T.);
#9500=EDGE_CURVE('',#7482,#7480,#4902,.T.);
#9501=EDGE_CURVE('',#7483,#7481,#4903,.T.);
#9502=EDGE_CURVE('',#7484,#7485,#5567,.T.);
#9503=EDGE_CURVE('',#7484,#7482,#4904,.T.);
#9504=EDGE_CURVE('',#7485,#7483,#4905,.T.);
#9505=EDGE_CURVE('',#7486,#7487,#5568,.T.);
#9506=EDGE_CURVE('',#7486,#7484,#4906,.T.);
#9507=EDGE_CURVE('',#7487,#7485,#4907,.T.);
#9508=EDGE_CURVE('',#7488,#7489,#5569,.T.);
#9509=EDGE_CURVE('',#7488,#7486,#4908,.T.);
#9510=EDGE_CURVE('',#7489,#7487,#4909,.T.);
#9511=EDGE_CURVE('',#7490,#7491,#5570,.T.);
#9512=EDGE_CURVE('',#7490,#7488,#4910,.T.);
#9513=EDGE_CURVE('',#7491,#7489,#4911,.T.);
#9514=EDGE_CURVE('',#7492,#7493,#5571,.T.);
#9515=EDGE_CURVE('',#7492,#7490,#4912,.T.);
#9516=EDGE_CURVE('',#7493,#7491,#4913,.T.);
#9517=EDGE_CURVE('',#7494,#7495,#5572,.T.);
#9518=EDGE_CURVE('',#7494,#7492,#4914,.T.);
#9519=EDGE_CURVE('',#7495,#7493,#4915,.T.);
#9520=EDGE_CURVE('',#7496,#7497,#5573,.T.);
#9521=EDGE_CURVE('',#7496,#7494,#4916,.T.);
#9522=EDGE_CURVE('',#7497,#7495,#4917,.T.);
#9523=EDGE_CURVE('',#7498,#7499,#5574,.T.);
#9524=EDGE_CURVE('',#7498,#7496,#4918,.T.);
#9525=EDGE_CURVE('',#7499,#7497,#4919,.T.);
#9526=EDGE_CURVE('',#7500,#7501,#5575,.T.);
#9527=EDGE_CURVE('',#7500,#7498,#4920,.T.);
#9528=EDGE_CURVE('',#7501,#7499,#4921,.T.);
#9529=EDGE_CURVE('',#7502,#7503,#5576,.T.);
#9530=EDGE_CURVE('',#7502,#7500,#4922,.T.);
#9531=EDGE_CURVE('',#7503,#7501,#4923,.T.);
#9532=EDGE_CURVE('',#7504,#7505,#5577,.T.);
#9533=EDGE_CURVE('',#7504,#7502,#4924,.T.);
#9534=EDGE_CURVE('',#7505,#7503,#4925,.T.);
#9535=EDGE_CURVE('',#7506,#7507,#5578,.T.);
#9536=EDGE_CURVE('',#7506,#7504,#4926,.T.);
#9537=EDGE_CURVE('',#7507,#7505,#4927,.T.);
#9538=EDGE_CURVE('',#7508,#7509,#5579,.T.);
#9539=EDGE_CURVE('',#7508,#7506,#4928,.T.);
#9540=EDGE_CURVE('',#7509,#7507,#4929,.T.);
#9541=EDGE_CURVE('',#7510,#7511,#5580,.T.);
#9542=EDGE_CURVE('',#7510,#7508,#4930,.T.);
#9543=EDGE_CURVE('',#7511,#7509,#4931,.T.);
#9544=EDGE_CURVE('',#7512,#7513,#5581,.T.);
#9545=EDGE_CURVE('',#7512,#7510,#4932,.T.);
#9546=EDGE_CURVE('',#7513,#7511,#4933,.T.);
#9547=EDGE_CURVE('',#7514,#7515,#5582,.T.);
#9548=EDGE_CURVE('',#7514,#7512,#4934,.T.);
#9549=EDGE_CURVE('',#7515,#7513,#4935,.T.);
#9550=EDGE_CURVE('',#7516,#7517,#5583,.T.);
#9551=EDGE_CURVE('',#7516,#7514,#4936,.T.);
#9552=EDGE_CURVE('',#7517,#7515,#4937,.T.);
#9553=EDGE_CURVE('',#7518,#7519,#5584,.T.);
#9554=EDGE_CURVE('',#7518,#7516,#4938,.T.);
#9555=EDGE_CURVE('',#7519,#7517,#4939,.T.);
#9556=EDGE_CURVE('',#7520,#7521,#5585,.T.);
#9557=EDGE_CURVE('',#7520,#7518,#4940,.T.);
#9558=EDGE_CURVE('',#7521,#7519,#4941,.T.);
#9559=EDGE_CURVE('',#7522,#7523,#5586,.T.);
#9560=EDGE_CURVE('',#7522,#7520,#4942,.T.);
#9561=EDGE_CURVE('',#7523,#7521,#4943,.T.);
#9562=EDGE_CURVE('',#7524,#7525,#5587,.T.);
#9563=EDGE_CURVE('',#7524,#7522,#4944,.T.);
#9564=EDGE_CURVE('',#7525,#7523,#4945,.T.);
#9565=EDGE_CURVE('',#7526,#7527,#5588,.T.);
#9566=EDGE_CURVE('',#7526,#7524,#4946,.T.);
#9567=EDGE_CURVE('',#7527,#7525,#4947,.T.);
#9568=EDGE_CURVE('',#7528,#7529,#5589,.T.);
#9569=EDGE_CURVE('',#7528,#7526,#4948,.T.);
#9570=EDGE_CURVE('',#7529,#7527,#4949,.T.);
#9571=EDGE_CURVE('',#7530,#7531,#5590,.T.);
#9572=EDGE_CURVE('',#7530,#7528,#4950,.T.);
#9573=EDGE_CURVE('',#7531,#7529,#4951,.T.);
#9574=EDGE_CURVE('',#7532,#7533,#5591,.T.);
#9575=EDGE_CURVE('',#7532,#7530,#4952,.T.);
#9576=EDGE_CURVE('',#7533,#7531,#4953,.T.);
#9577=EDGE_CURVE('',#7534,#7535,#5592,.T.);
#9578=EDGE_CURVE('',#7534,#7532,#4954,.T.);
#9579=EDGE_CURVE('',#7535,#7533,#4955,.T.);
#9580=EDGE_CURVE('',#7536,#7537,#5593,.T.);
#9581=EDGE_CURVE('',#7536,#7534,#4956,.T.);
#9582=EDGE_CURVE('',#7537,#7535,#4957,.T.);
#9583=EDGE_CURVE('',#7538,#7539,#5594,.T.);
#9584=EDGE_CURVE('',#7538,#7536,#4958,.T.);
#9585=EDGE_CURVE('',#7539,#7537,#4959,.T.);
#9586=EDGE_CURVE('',#7540,#7541,#5595,.T.);
#9587=EDGE_CURVE('',#7540,#7538,#4960,.T.);
#9588=EDGE_CURVE('',#7541,#7539,#4961,.T.);
#9589=EDGE_CURVE('',#7542,#7543,#5596,.T.);
#9590=EDGE_CURVE('',#7542,#7540,#4962,.T.);
#9591=EDGE_CURVE('',#7543,#7541,#4963,.T.);
#9592=EDGE_CURVE('',#7544,#7545,#5597,.T.);
#9593=EDGE_CURVE('',#7544,#7542,#4964,.T.);
#9594=EDGE_CURVE('',#7545,#7543,#4965,.T.);
#9595=EDGE_CURVE('',#7546,#7547,#5598,.T.);
#9596=EDGE_CURVE('',#7546,#7544,#4966,.T.);
#9597=EDGE_CURVE('',#7547,#7545,#4967,.T.);
#9598=EDGE_CURVE('',#7548,#7549,#5599,.T.);
#9599=EDGE_CURVE('',#7548,#7546,#4968,.T.);
#9600=EDGE_CURVE('',#7549,#7547,#4969,.T.);
#9601=EDGE_CURVE('',#7550,#7551,#5600,.T.);
#9602=EDGE_CURVE('',#7550,#7548,#4970,.T.);
#9603=EDGE_CURVE('',#7551,#7549,#4971,.T.);
#9604=EDGE_CURVE('',#7552,#7553,#5601,.T.);
#9605=EDGE_CURVE('',#7552,#7550,#4972,.T.);
#9606=EDGE_CURVE('',#7553,#7551,#4973,.T.);
#9607=EDGE_CURVE('',#7554,#7555,#5602,.T.);
#9608=EDGE_CURVE('',#7554,#7552,#4974,.T.);
#9609=EDGE_CURVE('',#7555,#7553,#4975,.T.);
#9610=EDGE_CURVE('',#7556,#7557,#5603,.T.);
#9611=EDGE_CURVE('',#7556,#7554,#4976,.T.);
#9612=EDGE_CURVE('',#7557,#7555,#4977,.T.);
#9613=EDGE_CURVE('',#7558,#7559,#5604,.T.);
#9614=EDGE_CURVE('',#7558,#7556,#4978,.T.);
#9615=EDGE_CURVE('',#7559,#7557,#4979,.T.);
#9616=EDGE_CURVE('',#7560,#7561,#5605,.T.);
#9617=EDGE_CURVE('',#7560,#7558,#4980,.T.);
#9618=EDGE_CURVE('',#7561,#7559,#4981,.T.);
#9619=EDGE_CURVE('',#7236,#7240,#5606,.T.);
#9620=EDGE_CURVE('',#7241,#7235,#5607,.T.);
#9621=EDGE_CURVE('',#7232,#7238,#5608,.T.);
#9622=EDGE_CURVE('',#7239,#7231,#5609,.T.);
#9623=EDGE_CURVE('',#7436,#7562,#4982,.T.);
#9624=EDGE_CURVE('',#7563,#7562,#3557,.F.);
#9625=EDGE_CURVE('',#7564,#7563,#3558,.F.);
#9626=EDGE_CURVE('',#7564,#7439,#4983,.T.);
#9627=EDGE_CURVE('',#7363,#7564,#4984,.T.);
#9628=EDGE_CURVE('',#7565,#7237,#4985,.T.);
#9629=EDGE_CURVE('',#7565,#7561,#4986,.T.);
#9630=EDGE_CURVE('',#7228,#7566,#4987,.T.);
#9631=EDGE_CURVE('',#7566,#7565,#3559,.T.);
#9632=EDGE_CURVE('',#7566,#7560,#4988,.T.);
#9633=EDGE_CURVE('',#7562,#7362,#4989,.T.);
#9634=EDGE_CURVE('',#7402,#7567,#4990,.T.);
#9635=EDGE_CURVE('',#7568,#7567,#3560,.T.);
#9636=EDGE_CURVE('',#7569,#7568,#3561,.T.);
#9637=EDGE_CURVE('',#7569,#7403,#4991,.T.);
#9638=EDGE_CURVE('',#7399,#7569,#4992,.T.);
#9639=EDGE_CURVE('',#7570,#7369,#4993,.T.);
#9640=EDGE_CURVE('',#7570,#7433,#4994,.T.);
#9641=EDGE_CURVE('',#7366,#7571,#4995,.T.);
#9642=EDGE_CURVE('',#7571,#7570,#3562,.T.);
#9643=EDGE_CURVE('',#7571,#7432,#4996,.T.);
#9644=EDGE_CURVE('',#7567,#7398,#4997,.T.);
#9645=EDGE_CURVE('',#7567,#7569,#3563,.T.);
#9646=EDGE_CURVE('',#7572,#7573,#3564,.T.);
#9647=EDGE_CURVE('',#7574,#7573,#608,.T.);
#9648=EDGE_CURVE('',#7575,#7574,#3565,.T.);
#9649=EDGE_CURVE('',#7572,#7575,#609,.T.);
#9650=EDGE_CURVE('',#7572,#7576,#4998,.T.);
#9651=EDGE_CURVE('',#7575,#7577,#5610,.T.);
#9652=EDGE_CURVE('',#7577,#7578,#610,.T.);
#9653=EDGE_CURVE('',#7579,#7578,#4999,.T.);
#9654=EDGE_CURVE('',#7576,#7579,#5000,.T.);
#9655=EDGE_CURVE('',#7574,#7580,#5611,.T.);
#9656=EDGE_CURVE('',#7580,#7577,#3566,.T.);
#9657=EDGE_CURVE('',#7581,#7573,#5001,.T.);
#9658=EDGE_CURVE('',#7582,#7581,#5002,.T.);
#9659=EDGE_CURVE('',#7583,#7582,#5003,.T.);
#9660=EDGE_CURVE('',#7583,#7580,#611,.T.);
#9661=EDGE_CURVE('',#7578,#7583,#3567,.T.);
#9662=EDGE_CURVE('',#7584,#7576,#3568,.T.);
#9663=EDGE_CURVE('',#7584,#7585,#5004,.T.);
#9664=EDGE_CURVE('',#7585,#7572,#3569,.T.);
#9665=EDGE_CURVE('',#7573,#7586,#3570,.T.);
#9666=EDGE_CURVE('',#7586,#7587,#5005,.T.);
#9667=EDGE_CURVE('',#7581,#7587,#3571,.T.);
#9668=EDGE_CURVE('',#7588,#7579,#3572,.T.);
#9669=EDGE_CURVE('',#7588,#7584,#5006,.T.);
#9670=EDGE_CURVE('',#7589,#7578,#3573,.T.);
#9671=EDGE_CURVE('',#7589,#7588,#5007,.T.);
#9672=EDGE_CURVE('',#7590,#7585,#3574,.T.);
#9673=EDGE_CURVE('',#7591,#7585,#612,.T.);
#9674=EDGE_CURVE('',#7592,#7591,#3575,.T.);
#9675=EDGE_CURVE('',#7590,#7592,#613,.T.);
#9676=EDGE_CURVE('',#7590,#7593,#5008,.T.);
#9677=EDGE_CURVE('',#7592,#7594,#5612,.T.);
#9678=EDGE_CURVE('',#7594,#7595,#614,.T.);
#9679=EDGE_CURVE('',#7596,#7595,#5009,.T.);
#9680=EDGE_CURVE('',#7593,#7596,#5010,.T.);
#9681=EDGE_CURVE('',#7591,#7597,#5613,.T.);
#9682=EDGE_CURVE('',#7597,#7594,#3576,.T.);
#9683=EDGE_CURVE('',#7589,#7597,#615,.T.);
#9684=EDGE_CURVE('',#7595,#7589,#3577,.T.);
#9685=EDGE_CURVE('',#7598,#7593,#3578,.T.);
#9686=EDGE_CURVE('',#7598,#7599,#5011,.T.);
#9687=EDGE_CURVE('',#7599,#7590,#3579,.T.);
#9688=EDGE_CURVE('',#7600,#7596,#3580,.T.);
#9689=EDGE_CURVE('',#7600,#7598,#5012,.T.);
#9690=EDGE_CURVE('',#7601,#7595,#3581,.T.);
#9691=EDGE_CURVE('',#7601,#7600,#5013,.T.);
#9692=EDGE_CURVE('',#7602,#7599,#3582,.T.);
#9693=EDGE_CURVE('',#7603,#7599,#616,.T.);
#9694=EDGE_CURVE('',#7604,#7603,#3583,.T.);
#9695=EDGE_CURVE('',#7602,#7604,#617,.T.);
#9696=EDGE_CURVE('',#7602,#7605,#5014,.T.);
#9697=EDGE_CURVE('',#7604,#7606,#5614,.T.);
#9698=EDGE_CURVE('',#7606,#7607,#618,.T.);
#9699=EDGE_CURVE('',#7608,#7607,#5015,.T.);
#9700=EDGE_CURVE('',#7605,#7608,#5016,.T.);
#9701=EDGE_CURVE('',#7603,#7609,#5615,.T.);
#9702=EDGE_CURVE('',#7609,#7606,#3584,.T.);
#9703=EDGE_CURVE('',#7601,#7609,#619,.T.);
#9704=EDGE_CURVE('',#7607,#7601,#3585,.T.);
#9705=EDGE_CURVE('',#7610,#7605,#3586,.T.);
#9706=EDGE_CURVE('',#7610,#7611,#5017,.T.);
#9707=EDGE_CURVE('',#7611,#7602,#3587,.T.);
#9708=EDGE_CURVE('',#7612,#7608,#3588,.T.);
#9709=EDGE_CURVE('',#7612,#7610,#5018,.T.);
#9710=EDGE_CURVE('',#7613,#7607,#3589,.T.);
#9711=EDGE_CURVE('',#7613,#7612,#5019,.T.);
#9712=EDGE_CURVE('',#7614,#7611,#3590,.T.);
#9713=EDGE_CURVE('',#7615,#7611,#620,.T.);
#9714=EDGE_CURVE('',#7616,#7615,#3591,.T.);
#9715=EDGE_CURVE('',#7614,#7616,#621,.T.);
#9716=EDGE_CURVE('',#7614,#7617,#5020,.T.);
#9717=EDGE_CURVE('',#7616,#7618,#5616,.T.);
#9718=EDGE_CURVE('',#7618,#7619,#622,.T.);
#9719=EDGE_CURVE('',#7620,#7619,#5021,.T.);
#9720=EDGE_CURVE('',#7617,#7620,#5022,.T.);
#9721=EDGE_CURVE('',#7615,#7621,#5617,.T.);
#9722=EDGE_CURVE('',#7621,#7618,#3592,.T.);
#9723=EDGE_CURVE('',#7613,#7621,#623,.T.);
#9724=EDGE_CURVE('',#7619,#7613,#3593,.T.);
#9725=EDGE_CURVE('',#7622,#7617,#3594,.T.);
#9726=EDGE_CURVE('',#7622,#7623,#5023,.T.);
#9727=EDGE_CURVE('',#7623,#7614,#3595,.T.);
#9728=EDGE_CURVE('',#7624,#7620,#3596,.T.);
#9729=EDGE_CURVE('',#7624,#7622,#5024,.T.);
#9730=EDGE_CURVE('',#7625,#7619,#3597,.T.);
#9731=EDGE_CURVE('',#7625,#7624,#5025,.T.);
#9732=EDGE_CURVE('',#7626,#7623,#3598,.T.);
#9733=EDGE_CURVE('',#7627,#7623,#624,.T.);
#9734=EDGE_CURVE('',#7628,#7627,#3599,.T.);
#9735=EDGE_CURVE('',#7626,#7628,#625,.T.);
#9736=EDGE_CURVE('',#7626,#7629,#5026,.T.);
#9737=EDGE_CURVE('',#7628,#7630,#5618,.T.);
#9738=EDGE_CURVE('',#7630,#7631,#626,.T.);
#9739=EDGE_CURVE('',#7632,#7631,#5027,.T.);
#9740=EDGE_CURVE('',#7629,#7632,#5028,.T.);
#9741=EDGE_CURVE('',#7627,#7633,#5619,.T.);
#9742=EDGE_CURVE('',#7633,#7630,#3600,.T.);
#9743=EDGE_CURVE('',#7625,#7633,#627,.T.);
#9744=EDGE_CURVE('',#7631,#7625,#3601,.T.);
#9745=EDGE_CURVE('',#7634,#7629,#3602,.T.);
#9746=EDGE_CURVE('',#7634,#7635,#5029,.T.);
#9747=EDGE_CURVE('',#7635,#7626,#3603,.T.);
#9748=EDGE_CURVE('',#7636,#7632,#3604,.T.);
#9749=EDGE_CURVE('',#7636,#7634,#5030,.T.);
#9750=EDGE_CURVE('',#7637,#7631,#3605,.T.);
#9751=EDGE_CURVE('',#7637,#7636,#5031,.T.);
#9752=EDGE_CURVE('',#7638,#7635,#3606,.T.);
#9753=EDGE_CURVE('',#7639,#7635,#628,.T.);
#9754=EDGE_CURVE('',#7640,#7639,#3607,.T.);
#9755=EDGE_CURVE('',#7638,#7640,#629,.T.);
#9756=EDGE_CURVE('',#7638,#7641,#5032,.T.);
#9757=EDGE_CURVE('',#7640,#7642,#5620,.T.);
#9758=EDGE_CURVE('',#7642,#7643,#630,.T.);
#9759=EDGE_CURVE('',#7644,#7643,#5033,.T.);
#9760=EDGE_CURVE('',#7641,#7644,#5034,.T.);
#9761=EDGE_CURVE('',#7639,#7645,#5621,.T.);
#9762=EDGE_CURVE('',#7645,#7642,#3608,.T.);
#9763=EDGE_CURVE('',#7637,#7645,#631,.T.);
#9764=EDGE_CURVE('',#7643,#7637,#3609,.T.);
#9765=EDGE_CURVE('',#7646,#7641,#3610,.T.);
#9766=EDGE_CURVE('',#7646,#7647,#5035,.T.);
#9767=EDGE_CURVE('',#7647,#7638,#3611,.T.);
#9768=EDGE_CURVE('',#7648,#7644,#3612,.T.);
#9769=EDGE_CURVE('',#7648,#7646,#5036,.T.);
#9770=EDGE_CURVE('',#7649,#7643,#3613,.T.);
#9771=EDGE_CURVE('',#7649,#7648,#5037,.T.);
#9772=EDGE_CURVE('',#7650,#7647,#3614,.T.);
#9773=EDGE_CURVE('',#7651,#7647,#632,.T.);
#9774=EDGE_CURVE('',#7652,#7651,#3615,.T.);
#9775=EDGE_CURVE('',#7650,#7652,#633,.T.);
#9776=EDGE_CURVE('',#7650,#7653,#5038,.T.);
#9777=EDGE_CURVE('',#7652,#7654,#5622,.T.);
#9778=EDGE_CURVE('',#7654,#7655,#634,.T.);
#9779=EDGE_CURVE('',#7656,#7655,#5039,.T.);
#9780=EDGE_CURVE('',#7653,#7656,#5040,.T.);
#9781=EDGE_CURVE('',#7651,#7657,#5623,.T.);
#9782=EDGE_CURVE('',#7657,#7654,#3616,.T.);
#9783=EDGE_CURVE('',#7649,#7657,#635,.T.);
#9784=EDGE_CURVE('',#7655,#7649,#3617,.T.);
#9785=EDGE_CURVE('',#7658,#7653,#3618,.T.);
#9786=EDGE_CURVE('',#7658,#7659,#5041,.T.);
#9787=EDGE_CURVE('',#7659,#7650,#3619,.T.);
#9788=EDGE_CURVE('',#7660,#7656,#3620,.T.);
#9789=EDGE_CURVE('',#7660,#7658,#5042,.T.);
#9790=EDGE_CURVE('',#7661,#7655,#3621,.T.);
#9791=EDGE_CURVE('',#7661,#7660,#5043,.T.);
#9792=EDGE_CURVE('',#7662,#7663,#3622,.T.);
#9793=EDGE_CURVE('',#7663,#7659,#3623,.T.);
#9794=EDGE_CURVE('',#7664,#7659,#636,.T.);
#9795=EDGE_CURVE('',#7665,#7664,#3624,.T.);
#9796=EDGE_CURVE('',#7662,#7665,#637,.T.);
#9797=EDGE_CURVE('',#7662,#7666,#5044,.T.);
#9798=EDGE_CURVE('',#7665,#7667,#5624,.T.);
#9799=EDGE_CURVE('',#7667,#7668,#638,.T.);
#9800=EDGE_CURVE('',#7669,#7668,#5045,.T.);
#9801=EDGE_CURVE('',#7666,#7669,#5046,.T.);
#9802=EDGE_CURVE('',#7664,#7670,#5625,.T.);
#9803=EDGE_CURVE('',#7670,#7667,#3625,.T.);
#9804=EDGE_CURVE('',#7661,#7670,#639,.T.);
#9805=EDGE_CURVE('',#7668,#7671,#3626,.T.);
#9806=EDGE_CURVE('',#7671,#7661,#3627,.T.);
#9807=EDGE_CURVE('',#7672,#7666,#3628,.T.);
#9808=EDGE_CURVE('',#7672,#7673,#5047,.T.);
#9809=EDGE_CURVE('',#7673,#7662,#3629,.T.);
#9810=EDGE_CURVE('',#7674,#7669,#3630,.T.);
#9811=EDGE_CURVE('',#7674,#7672,#5048,.T.);
#9812=EDGE_CURVE('',#7675,#7668,#3631,.T.);
#9813=EDGE_CURVE('',#7675,#7674,#5049,.T.);
#9814=EDGE_CURVE('',#7676,#7673,#3632,.T.);
#9815=EDGE_CURVE('',#7677,#7673,#640,.T.);
#9816=EDGE_CURVE('',#7678,#7677,#3633,.T.);
#9817=EDGE_CURVE('',#7676,#7678,#641,.T.);
#9818=EDGE_CURVE('',#7676,#7679,#5050,.T.);
#9819=EDGE_CURVE('',#7678,#7680,#5626,.T.);
#9820=EDGE_CURVE('',#7680,#7681,#642,.T.);
#9821=EDGE_CURVE('',#7682,#7681,#5051,.T.);
#9822=EDGE_CURVE('',#7679,#7682,#5052,.T.);
#9823=EDGE_CURVE('',#7677,#7683,#5627,.T.);
#9824=EDGE_CURVE('',#7683,#7680,#3634,.T.);
#9825=EDGE_CURVE('',#7675,#7683,#643,.T.);
#9826=EDGE_CURVE('',#7681,#7675,#3635,.T.);
#9827=EDGE_CURVE('',#7684,#7679,#3636,.T.);
#9828=EDGE_CURVE('',#7684,#7685,#5053,.T.);
#9829=EDGE_CURVE('',#7685,#7676,#3637,.T.);
#9830=EDGE_CURVE('',#7686,#7682,#3638,.T.);
#9831=EDGE_CURVE('',#7686,#7684,#5054,.T.);
#9832=EDGE_CURVE('',#7687,#7681,#3639,.T.);
#9833=EDGE_CURVE('',#7687,#7686,#5055,.T.);
#9834=EDGE_CURVE('',#7688,#7685,#3640,.T.);
#9835=EDGE_CURVE('',#7689,#7685,#644,.T.);
#9836=EDGE_CURVE('',#7690,#7689,#3641,.T.);
#9837=EDGE_CURVE('',#7688,#7690,#645,.T.);
#9838=EDGE_CURVE('',#7688,#7691,#5056,.T.);
#9839=EDGE_CURVE('',#7690,#7692,#5628,.T.);
#9840=EDGE_CURVE('',#7692,#7693,#646,.T.);
#9841=EDGE_CURVE('',#7694,#7693,#5057,.T.);
#9842=EDGE_CURVE('',#7691,#7694,#5058,.T.);
#9843=EDGE_CURVE('',#7689,#7695,#5629,.T.);
#9844=EDGE_CURVE('',#7695,#7692,#3642,.T.);
#9845=EDGE_CURVE('',#7687,#7695,#647,.T.);
#9846=EDGE_CURVE('',#7693,#7687,#3643,.T.);
#9847=EDGE_CURVE('',#7696,#7691,#3644,.T.);
#9848=EDGE_CURVE('',#7696,#7697,#5059,.T.);
#9849=EDGE_CURVE('',#7697,#7688,#3645,.T.);
#9850=EDGE_CURVE('',#7698,#7694,#3646,.T.);
#9851=EDGE_CURVE('',#7698,#7696,#5060,.T.);
#9852=EDGE_CURVE('',#7699,#7693,#3647,.T.);
#9853=EDGE_CURVE('',#7699,#7698,#5061,.T.);
#9854=EDGE_CURVE('',#7700,#7697,#3648,.T.);
#9855=EDGE_CURVE('',#7701,#7697,#648,.T.);
#9856=EDGE_CURVE('',#7702,#7701,#3649,.T.);
#9857=EDGE_CURVE('',#7700,#7702,#649,.T.);
#9858=EDGE_CURVE('',#7700,#7703,#5062,.T.);
#9859=EDGE_CURVE('',#7702,#7704,#5630,.T.);
#9860=EDGE_CURVE('',#7704,#7705,#650,.T.);
#9861=EDGE_CURVE('',#7706,#7705,#5063,.T.);
#9862=EDGE_CURVE('',#7703,#7706,#5064,.T.);
#9863=EDGE_CURVE('',#7701,#7707,#5631,.T.);
#9864=EDGE_CURVE('',#7707,#7704,#3650,.T.);
#9865=EDGE_CURVE('',#7699,#7707,#651,.T.);
#9866=EDGE_CURVE('',#7705,#7699,#3651,.T.);
#9867=EDGE_CURVE('',#7708,#7703,#3652,.T.);
#9868=EDGE_CURVE('',#7708,#7709,#5065,.T.);
#9869=EDGE_CURVE('',#7709,#7700,#3653,.T.);
#9870=EDGE_CURVE('',#7710,#7706,#3654,.T.);
#9871=EDGE_CURVE('',#7710,#7708,#5066,.T.);
#9872=EDGE_CURVE('',#7711,#7705,#3655,.T.);
#9873=EDGE_CURVE('',#7711,#7710,#5067,.T.);
#9874=EDGE_CURVE('',#7712,#7709,#3656,.T.);
#9875=EDGE_CURVE('',#7713,#7709,#652,.T.);
#9876=EDGE_CURVE('',#7714,#7713,#3657,.T.);
#9877=EDGE_CURVE('',#7712,#7714,#653,.T.);
#9878=EDGE_CURVE('',#7712,#7715,#5068,.T.);
#9879=EDGE_CURVE('',#7714,#7716,#5632,.T.);
#9880=EDGE_CURVE('',#7716,#7717,#654,.T.);
#9881=EDGE_CURVE('',#7718,#7717,#5069,.T.);
#9882=EDGE_CURVE('',#7715,#7718,#5070,.T.);
#9883=EDGE_CURVE('',#7713,#7719,#5633,.T.);
#9884=EDGE_CURVE('',#7719,#7716,#3658,.T.);
#9885=EDGE_CURVE('',#7711,#7719,#655,.T.);
#9886=EDGE_CURVE('',#7717,#7711,#3659,.T.);
#9887=EDGE_CURVE('',#7720,#7715,#3660,.T.);
#9888=EDGE_CURVE('',#7720,#7721,#5071,.T.);
#9889=EDGE_CURVE('',#7721,#7712,#3661,.T.);
#9890=EDGE_CURVE('',#7722,#7718,#3662,.T.);
#9891=EDGE_CURVE('',#7722,#7720,#5072,.T.);
#9892=EDGE_CURVE('',#7723,#7717,#3663,.T.);
#9893=EDGE_CURVE('',#7723,#7722,#5073,.T.);
#9894=EDGE_CURVE('',#7724,#7721,#3664,.T.);
#9895=EDGE_CURVE('',#7725,#7721,#656,.T.);
#9896=EDGE_CURVE('',#7726,#7725,#3665,.T.);
#9897=EDGE_CURVE('',#7724,#7726,#657,.T.);
#9898=EDGE_CURVE('',#7724,#7727,#5074,.T.);
#9899=EDGE_CURVE('',#7726,#7728,#5634,.T.);
#9900=EDGE_CURVE('',#7728,#7729,#658,.T.);
#9901=EDGE_CURVE('',#7730,#7729,#5075,.T.);
#9902=EDGE_CURVE('',#7727,#7730,#5076,.T.);
#9903=EDGE_CURVE('',#7725,#7731,#5635,.T.);
#9904=EDGE_CURVE('',#7731,#7728,#3666,.T.);
#9905=EDGE_CURVE('',#7723,#7731,#659,.T.);
#9906=EDGE_CURVE('',#7729,#7723,#3667,.T.);
#9907=EDGE_CURVE('',#7732,#7727,#3668,.T.);
#9908=EDGE_CURVE('',#7732,#7733,#5077,.T.);
#9909=EDGE_CURVE('',#7733,#7724,#3669,.T.);
#9910=EDGE_CURVE('',#7734,#7730,#3670,.T.);
#9911=EDGE_CURVE('',#7734,#7732,#5078,.T.);
#9912=EDGE_CURVE('',#7735,#7729,#3671,.T.);
#9913=EDGE_CURVE('',#7735,#7734,#5079,.T.);
#9914=EDGE_CURVE('',#7736,#7733,#3672,.T.);
#9915=EDGE_CURVE('',#7737,#7733,#660,.T.);
#9916=EDGE_CURVE('',#7738,#7737,#3673,.T.);
#9917=EDGE_CURVE('',#7736,#7738,#661,.T.);
#9918=EDGE_CURVE('',#7736,#7739,#5080,.T.);
#9919=EDGE_CURVE('',#7738,#7740,#5636,.T.);
#9920=EDGE_CURVE('',#7740,#7741,#662,.T.);
#9921=EDGE_CURVE('',#7742,#7741,#5081,.T.);
#9922=EDGE_CURVE('',#7739,#7742,#5082,.T.);
#9923=EDGE_CURVE('',#7737,#7743,#5637,.T.);
#9924=EDGE_CURVE('',#7743,#7740,#3674,.T.);
#9925=EDGE_CURVE('',#7735,#7743,#663,.T.);
#9926=EDGE_CURVE('',#7741,#7735,#3675,.T.);
#9927=EDGE_CURVE('',#7744,#7739,#3676,.T.);
#9928=EDGE_CURVE('',#7744,#7745,#5083,.T.);
#9929=EDGE_CURVE('',#7745,#7736,#3677,.T.);
#9930=EDGE_CURVE('',#7746,#7742,#3678,.T.);
#9931=EDGE_CURVE('',#7746,#7744,#5084,.T.);
#9932=EDGE_CURVE('',#7747,#7741,#3679,.T.);
#9933=EDGE_CURVE('',#7747,#7746,#5085,.T.);
#9934=EDGE_CURVE('',#7747,#7748,#664,.T.);
#9935=EDGE_CURVE('',#7749,#7748,#5638,.T.);
#9936=EDGE_CURVE('',#7749,#7745,#665,.T.);
#9937=EDGE_CURVE('',#7586,#7745,#3680,.T.);
#9938=EDGE_CURVE('',#7750,#7749,#3681,.T.);
#9939=EDGE_CURVE('',#7586,#7750,#666,.T.);
#9940=EDGE_CURVE('',#7748,#7751,#3682,.T.);
#9941=EDGE_CURVE('',#7750,#7751,#5639,.T.);
#9942=EDGE_CURVE('',#7752,#7753,#5086,.T.);
#9943=EDGE_CURVE('',#7587,#7752,#5087,.T.);
#9944=EDGE_CURVE('',#7751,#7753,#667,.T.);
#9945=EDGE_CURVE('',#7753,#7747,#3683,.T.);
#9946=EDGE_CURVE('',#7582,#7752,#3684,.T.);
#9947=EDGE_CURVE('',#7583,#7753,#3685,.T.);
#9948=EDGE_CURVE('',#7754,#7754,#3686,.T.);
#9949=EDGE_CURVE('',#7368,#7754,#5640,.T.);
#9950=EDGE_CURVE('',#7663,#7568,#5641,.T.);
#9951=EDGE_CURVE('',#7234,#7671,#5642,.T.);
#9952=EDGE_CURVE('',#7562,#7564,#3687,.F.);
#9953=EDGE_CURVE('',#7755,#7755,#3688,.T.);
#9954=EDGE_CURVE('',#7755,#7563,#5643,.T.);
#9955=EDGE_CURVE('',#7756,#7757,#3689,.T.);
#9956=EDGE_CURVE('',#7757,#7758,#5644,.T.);
#9957=EDGE_CURVE('',#7758,#7759,#3690,.T.);
#9958=EDGE_CURVE('',#7759,#7756,#5645,.T.);
#9959=EDGE_CURVE('',#7760,#7761,#3691,.T.);
#9960=EDGE_CURVE('',#7761,#7759,#3692,.T.);
#9961=EDGE_CURVE('',#7758,#7760,#3693,.T.);
#9962=EDGE_CURVE('',#7762,#7763,#3694,.T.);
#9963=EDGE_CURVE('',#7763,#7757,#5646,.T.);
#9964=EDGE_CURVE('',#7764,#7757,#3695,.T.);
#9965=EDGE_CURVE('',#7764,#7762,#5647,.T.);
#9966=EDGE_CURVE('',#7765,#7766,#3696,.T.);
#9967=EDGE_CURVE('',#7766,#7767,#5648,.T.);
#9968=EDGE_CURVE('',#7767,#7762,#3697,.T.);
#9969=EDGE_CURVE('',#7762,#7765,#5649,.T.);
#9970=EDGE_CURVE('',#7767,#7763,#3698,.T.);
#9971=EDGE_CURVE('',#7768,#7769,#3699,.T.);
#9972=EDGE_CURVE('',#7768,#7770,#3700,.T.);
#9973=EDGE_CURVE('',#7770,#7771,#3701,.T.);
#9974=EDGE_CURVE('',#7771,#7769,#3702,.T.);
#9975=EDGE_CURVE('',#7772,#7773,#3703,.T.);
#9976=EDGE_CURVE('',#7773,#7771,#5650,.T.);
#9977=EDGE_CURVE('',#7770,#7772,#5651,.T.);
#9978=EDGE_CURVE('',#7774,#7765,#3704,.T.);
#9979=EDGE_CURVE('',#7765,#7775,#5652,.T.);
#9980=EDGE_CURVE('',#7772,#7775,#3705,.T.);
#9981=EDGE_CURVE('',#7772,#7774,#5653,.T.);
#9982=EDGE_CURVE('',#7774,#7766,#3706,.T.);
#9983=EDGE_CURVE('',#7758,#7776,#5654,.T.);
#9984=EDGE_CURVE('',#7776,#7777,#3707,.T.);
#9985=EDGE_CURVE('',#7777,#7760,#5655,.T.);
#9986=EDGE_CURVE('',#7776,#7763,#5656,.T.);
#9987=EDGE_CURVE('',#7767,#7778,#5657,.T.);
#9988=EDGE_CURVE('',#7778,#7776,#3708,.T.);
#9989=EDGE_CURVE('',#7779,#7766,#5658,.T.);
#9990=EDGE_CURVE('',#7778,#7779,#5659,.T.);
#9991=EDGE_CURVE('',#7774,#7780,#5660,.T.);
#9992=EDGE_CURVE('',#7779,#7780,#3709,.T.);
#9993=EDGE_CURVE('',#7780,#7770,#5661,.T.);
#9994=EDGE_CURVE('',#7760,#7768,#5662,.T.);
#9995=EDGE_CURVE('',#7769,#7761,#5663,.T.);
#9996=EDGE_CURVE('',#7768,#7781,#5664,.T.);
#9997=EDGE_CURVE('',#7781,#7780,#3710,.T.);
#9998=EDGE_CURVE('',#7778,#7777,#3711,.T.);
#9999=EDGE_CURVE('',#7781,#7777,#5665,.T.);
#10000=EDGE_CURVE('',#7779,#7781,#3712,.T.);
#10001=EDGE_CURVE('',#7775,#7764,#5666,.T.);
#10002=EDGE_CURVE('',#7782,#7783,#5088,.F.);
#10003=EDGE_CURVE('',#7784,#7783,#200,.T.);
#10004=EDGE_CURVE('',#7785,#7784,#201,.T.);
#10005=EDGE_CURVE('',#7785,#7786,#5667,.T.);
#10006=EDGE_CURVE('',#7786,#7756,#3713,.T.);
#10007=EDGE_CURVE('',#7756,#7782,#5668,.T.);
#10008=EDGE_CURVE('',#7786,#7764,#3714,.T.);
#10009=EDGE_CURVE('',#7787,#7759,#5669,.T.);
#10010=EDGE_CURVE('',#7788,#7787,#3715,.F.);
#10011=EDGE_CURVE('',#7788,#7789,#5670,.T.);
#10012=EDGE_CURVE('',#7782,#7789,#3716,.F.);
#10013=EDGE_CURVE('',#7786,#7790,#5671,.T.);
#10014=EDGE_CURVE('',#7790,#7775,#3717,.T.);
#10015=EDGE_CURVE('',#7790,#7773,#3718,.T.);
#10016=EDGE_CURVE('',#7790,#7791,#5672,.T.);
#10017=EDGE_CURVE('',#7791,#7792,#3719,.F.);
#10018=EDGE_CURVE('',#7792,#7773,#5673,.T.);
#10019=EDGE_CURVE('',#7793,#7785,#5674,.T.);
#10020=EDGE_CURVE('',#7794,#7793,#5675,.T.);
#10021=EDGE_CURVE('',#7791,#7794,#5676,.T.);
#10022=EDGE_CURVE('',#7795,#7796,#3720,.T.);
#10023=EDGE_CURVE('',#7796,#7793,#3721,.T.);
#10024=EDGE_CURVE('',#7793,#7797,#3722,.T.);
#10025=EDGE_CURVE('',#7797,#7795,#3723,.T.);
#10026=EDGE_CURVE('',#7784,#7797,#5677,.F.);
#10027=EDGE_CURVE('',#7796,#7798,#5678,.T.);
#10028=EDGE_CURVE('',#7798,#7799,#5089,.F.);
#10029=EDGE_CURVE('',#7799,#7794,#3724,.F.);
#10030=EDGE_CURVE('',#7795,#7800,#5679,.T.);
#10031=EDGE_CURVE('',#7800,#7801,#3725,.T.);
#10032=EDGE_CURVE('',#7801,#7796,#5680,.T.);
#10033=EDGE_CURVE('',#7797,#7802,#5681,.T.);
#10034=EDGE_CURVE('',#7802,#7803,#3726,.T.);
#10035=EDGE_CURVE('',#7803,#7795,#5682,.T.);
#10036=EDGE_CURVE('',#7804,#7802,#3727,.T.);
#10037=EDGE_CURVE('',#7802,#7783,#5683,.T.);
#10038=EDGE_CURVE('',#7789,#7804,#5684,.T.);
#10039=EDGE_CURVE('',#7804,#7803,#3728,.T.);
#10040=EDGE_CURVE('',#7805,#7803,#5685,.T.);
#10041=EDGE_CURVE('',#7800,#7805,#5686,.T.);
#10042=EDGE_CURVE('',#7804,#7806,#5687,.T.);
#10043=EDGE_CURVE('',#7805,#7806,#3729,.T.);
#10044=EDGE_CURVE('',#7806,#7788,#5688,.T.);
#10045=EDGE_CURVE('',#7771,#7807,#5689,.T.);
#10046=EDGE_CURVE('',#7807,#7808,#3730,.F.);
#10047=EDGE_CURVE('',#7808,#7769,#5690,.T.);
#10048=EDGE_CURVE('',#7809,#7808,#5691,.T.);
#10049=EDGE_CURVE('',#7810,#7809,#5692,.T.);
#10050=EDGE_CURVE('',#7811,#7810,#5693,.T.);
#10051=EDGE_CURVE('',#7761,#7811,#5694,.T.);
#10052=EDGE_CURVE('',#7811,#7812,#202,.F.);
#10053=EDGE_CURVE('',#7812,#7813,#203,.F.);
#10054=EDGE_CURVE('',#7787,#7813,#5090,.T.);
#10055=EDGE_CURVE('',#7814,#7806,#3731,.T.);
#10056=EDGE_CURVE('',#7813,#7814,#5695,.F.);
#10057=EDGE_CURVE('',#7814,#7805,#3732,.T.);
#10058=EDGE_CURVE('',#7800,#7815,#3733,.T.);
#10059=EDGE_CURVE('',#7814,#7815,#5696,.T.);
#10060=EDGE_CURVE('',#7816,#7801,#5697,.T.);
#10061=EDGE_CURVE('',#7817,#7816,#5091,.F.);
#10062=EDGE_CURVE('',#7818,#7817,#5698,.T.);
#10063=EDGE_CURVE('',#7818,#7798,#5092,.T.);
#10064=EDGE_CURVE('',#7810,#7815,#3734,.T.);
#10065=EDGE_CURVE('',#7815,#7812,#5699,.T.);
#10066=EDGE_CURVE('',#7810,#7801,#3735,.T.);
#10067=EDGE_CURVE('',#7819,#7809,#3736,.T.);
#10068=EDGE_CURVE('',#7816,#7819,#5093,.T.);
#10069=EDGE_CURVE('',#7820,#7821,#3737,.T.);
#10070=EDGE_CURVE('',#7821,#7822,#5700,.T.);
#10071=EDGE_CURVE('',#7822,#7823,#3738,.F.);
#10072=EDGE_CURVE('',#7823,#7820,#5701,.T.);
#10073=EDGE_CURVE('',#7824,#7820,#3739,.T.);
#10074=EDGE_CURVE('',#7820,#7825,#5702,.T.);
#10075=EDGE_CURVE('',#7825,#7826,#3740,.T.);
#10076=EDGE_CURVE('',#7826,#7824,#5703,.T.);
#10077=EDGE_CURVE('',#7827,#7828,#3741,.T.);
#10078=EDGE_CURVE('',#7827,#7826,#3742,.T.);
#10079=EDGE_CURVE('',#7825,#7828,#3743,.T.);
#10080=EDGE_CURVE('',#7829,#7821,#5704,.T.);
#10081=EDGE_CURVE('',#7830,#7829,#5705,.T.);
#10082=EDGE_CURVE('',#7822,#7830,#5706,.T.);
#10083=EDGE_CURVE('',#7831,#7826,#5707,.T.);
#10084=EDGE_CURVE('',#7832,#7831,#5708,.T.);
#10085=EDGE_CURVE('',#7824,#7832,#5709,.T.);
#10086=EDGE_CURVE('',#7833,#7824,#3744,.T.);
#10087=EDGE_CURVE('',#7832,#7834,#3745,.T.);
#10088=EDGE_CURVE('',#7834,#7833,#5710,.T.);
#10089=EDGE_CURVE('',#7833,#7821,#3746,.T.);
#10090=EDGE_CURVE('',#7831,#7835,#3747,.T.);
#10091=EDGE_CURVE('',#7835,#7836,#5711,.T.);
#10092=EDGE_CURVE('',#7836,#7832,#3748,.T.);
#10093=EDGE_CURVE('',#7836,#7834,#3749,.T.);
#10094=EDGE_CURVE('',#7827,#7837,#5712,.T.);
#10095=EDGE_CURVE('',#7837,#7831,#3750,.T.);
#10096=EDGE_CURVE('',#7837,#7835,#3751,.T.);
#10097=EDGE_CURVE('',#7833,#7838,#5713,.T.);
#10098=EDGE_CURVE('',#7838,#7829,#3752,.T.);
#10099=EDGE_CURVE('',#7839,#7834,#5714,.T.);
#10100=EDGE_CURVE('',#7838,#7839,#5715,.T.);
#10101=EDGE_CURVE('',#7836,#7840,#5716,.T.);
#10102=EDGE_CURVE('',#7839,#7840,#3753,.T.);
#10103=EDGE_CURVE('',#7841,#7835,#5717,.T.);
#10104=EDGE_CURVE('',#7840,#7841,#5718,.T.);
#10105=EDGE_CURVE('',#7837,#7842,#5719,.T.);
#10106=EDGE_CURVE('',#7841,#7842,#3754,.T.);
#10107=EDGE_CURVE('',#7843,#7827,#5720,.T.);
#10108=EDGE_CURVE('',#7842,#7843,#5721,.T.);
#10109=EDGE_CURVE('',#7828,#7844,#5722,.T.);
#10110=EDGE_CURVE('',#7844,#7843,#3755,.T.);
#10111=EDGE_CURVE('',#7845,#7846,#3756,.T.);
#10112=EDGE_CURVE('',#7846,#7847,#5723,.T.);
#10113=EDGE_CURVE('',#7847,#7848,#204,.F.);
#10114=EDGE_CURVE('',#7848,#7845,#5724,.T.);
#10115=EDGE_CURVE('',#7849,#7850,#5094,.T.);
#10116=EDGE_CURVE('',#7849,#7851,#5725,.T.);
#10117=EDGE_CURVE('',#7851,#7845,#3757,.T.);
#10118=EDGE_CURVE('',#7845,#7852,#5726,.T.);
#10119=EDGE_CURVE('',#7850,#7852,#3758,.T.);
#10120=EDGE_CURVE('',#7851,#7846,#3759,.T.);
#10121=EDGE_CURVE('',#7853,#7846,#5727,.T.);
#10122=EDGE_CURVE('',#7854,#7853,#5728,.T.);
#10123=EDGE_CURVE('',#7847,#7854,#5729,.T.);
#10124=EDGE_CURVE('',#7851,#7855,#5730,.T.);
#10125=EDGE_CURVE('',#7855,#7853,#3760,.T.);
#10126=EDGE_CURVE('',#7856,#7849,#5095,.F.);
#10127=EDGE_CURVE('',#7857,#7856,#5731,.T.);
#10128=EDGE_CURVE('',#7857,#7858,#5096,.T.);
#10129=EDGE_CURVE('',#7855,#7858,#5732,.T.);
#10130=EDGE_CURVE('',#7855,#7859,#3761,.T.);
#10131=EDGE_CURVE('',#7859,#7853,#3762,.T.);
#10132=EDGE_CURVE('',#7852,#7823,#5733,.T.);
#10133=EDGE_CURVE('',#7825,#7848,#5734,.T.);
#10134=EDGE_CURVE('',#7858,#7860,#5097,.F.);
#10135=EDGE_CURVE('',#7860,#7861,#3763,.F.);
#10136=EDGE_CURVE('',#7861,#7859,#5735,.T.);
#10137=EDGE_CURVE('',#7859,#7862,#5736,.T.);
#10138=EDGE_CURVE('',#7862,#7854,#205,.F.);
#10139=EDGE_CURVE('',#7863,#7842,#3764,.T.);
#10140=EDGE_CURVE('',#7864,#7843,#3765,.T.);
#10141=EDGE_CURVE('',#7864,#7863,#5737,.T.);
#10142=EDGE_CURVE('',#7865,#7840,#3766,.T.);
#10143=EDGE_CURVE('',#7841,#7863,#3767,.T.);
#10144=EDGE_CURVE('',#7863,#7865,#5738,.T.);
#10145=EDGE_CURVE('',#7865,#7839,#3768,.T.);
#10146=EDGE_CURVE('',#7866,#7838,#3769,.T.);
#10147=EDGE_CURVE('',#7865,#7866,#5739,.T.);
#10148=EDGE_CURVE('',#7866,#7864,#5740,.T.);
#10149=EDGE_CURVE('',#7847,#7828,#5741,.T.);
#10150=EDGE_CURVE('',#7844,#7854,#5742,.T.);
#10151=EDGE_CURVE('',#7867,#7844,#3770,.T.);
#10152=EDGE_CURVE('',#7862,#7867,#5743,.T.);
#10153=EDGE_CURVE('',#7867,#7864,#3771,.T.);
#10154=EDGE_CURVE('',#7867,#7868,#5744,.T.);
#10155=EDGE_CURVE('',#7868,#7866,#3772,.T.);
#10156=EDGE_CURVE('',#7869,#7861,#5745,.T.);
#10157=EDGE_CURVE('',#7868,#7869,#5746,.T.);
#10158=EDGE_CURVE('',#7868,#7829,#3773,.T.);
#10159=EDGE_CURVE('',#7869,#7830,#3774,.F.);
#10160=EDGE_CURVE('',#7870,#7871,#5098,.T.);
#10161=EDGE_CURVE('',#7870,#7872,#5747,.T.);
#10162=EDGE_CURVE('',#7872,#7873,#3775,.T.);
#10163=EDGE_CURVE('',#7873,#7874,#5748,.T.);
#10164=EDGE_CURVE('',#7871,#7874,#3776,.T.);
#10165=EDGE_CURVE('',#7875,#7876,#206,.T.);
#10166=EDGE_CURVE('',#7876,#7877,#5749,.T.);
#10167=EDGE_CURVE('',#7877,#7872,#3777,.T.);
#10168=EDGE_CURVE('',#7872,#7878,#5750,.T.);
#10169=EDGE_CURVE('',#7878,#7875,#207,.T.);
#10170=EDGE_CURVE('',#7877,#7873,#3778,.T.);
#10171=EDGE_CURVE('',#7879,#7873,#5751,.T.);
#10172=EDGE_CURVE('',#7880,#7879,#5752,.T.);
#10173=EDGE_CURVE('',#7874,#7880,#5753,.T.);
#10174=EDGE_CURVE('',#7877,#7881,#5754,.T.);
#10175=EDGE_CURVE('',#7882,#7881,#208,.T.);
#10176=EDGE_CURVE('',#7879,#7882,#209,.T.);
#10177=EDGE_CURVE('',#7883,#7876,#5755,.T.);
#10178=EDGE_CURVE('',#7881,#7883,#5756,.T.);
#10179=EDGE_CURVE('',#7884,#7875,#210,.T.);
#10180=EDGE_CURVE('',#7884,#7885,#5757,.T.);
#10181=EDGE_CURVE('',#7885,#7883,#3779,.T.);
#10182=EDGE_CURVE('',#7878,#7886,#211,.T.);
#10183=EDGE_CURVE('',#7886,#7887,#5758,.T.);
#10184=EDGE_CURVE('',#7888,#7887,#3780,.T.);
#10185=EDGE_CURVE('',#7888,#7884,#5759,.T.);
#10186=EDGE_CURVE('',#7889,#7890,#3781,.T.);
#10187=EDGE_CURVE('',#7890,#7891,#5760,.T.);
#10188=EDGE_CURVE('',#7891,#7892,#3782,.T.);
#10189=EDGE_CURVE('',#7892,#7889,#5761,.T.);
#10190=EDGE_CURVE('',#7893,#7894,#3783,.T.);
#10191=EDGE_CURVE('',#7893,#7892,#3784,.T.);
#10192=EDGE_CURVE('',#7891,#7894,#3785,.T.);
#10193=EDGE_CURVE('',#7895,#7896,#3786,.T.);
#10194=EDGE_CURVE('',#7896,#7890,#3787,.T.);
#10195=EDGE_CURVE('',#7889,#7895,#3788,.T.);
#10196=EDGE_CURVE('',#7896,#7897,#5762,.T.);
#10197=EDGE_CURVE('',#7897,#7898,#3789,.F.);
#10198=EDGE_CURVE('',#7898,#7890,#5763,.T.);
#10199=EDGE_CURVE('',#7895,#7899,#5764,.T.);
#10200=EDGE_CURVE('',#7900,#7899,#3790,.T.);
#10201=EDGE_CURVE('',#7900,#7896,#5765,.T.);
#10202=EDGE_CURVE('',#7889,#7901,#5766,.T.);
#10203=EDGE_CURVE('',#7901,#7902,#3791,.T.);
#10204=EDGE_CURVE('',#7902,#7895,#5767,.T.);
#10205=EDGE_CURVE('',#7903,#7892,#5768,.T.);
#10206=EDGE_CURVE('',#7901,#7903,#5769,.T.);
#10207=EDGE_CURVE('',#7893,#7904,#5770,.T.);
#10208=EDGE_CURVE('',#7904,#7903,#3792,.T.);
#10209=EDGE_CURVE('',#7905,#7906,#3793,.T.);
#10210=EDGE_CURVE('',#7906,#7907,#5771,.T.);
#10211=EDGE_CURVE('',#7907,#7904,#3794,.T.);
#10212=EDGE_CURVE('',#7904,#7905,#5772,.T.);
#10213=EDGE_CURVE('',#7905,#7908,#3795,.T.);
#10214=EDGE_CURVE('',#7908,#7906,#3796,.T.);
#10215=EDGE_CURVE('',#7907,#7903,#3797,.T.);
#10216=EDGE_CURVE('',#7909,#7910,#212,.T.);
#10217=EDGE_CURVE('',#7910,#7908,#5773,.T.);
#10218=EDGE_CURVE('',#7905,#7911,#5774,.T.);
#10219=EDGE_CURVE('',#7911,#7909,#213,.T.);
#10220=EDGE_CURVE('',#7907,#7912,#5775,.T.);
#10221=EDGE_CURVE('',#7912,#7901,#3798,.T.);
#10222=EDGE_CURVE('',#7913,#7906,#5776,.T.);
#10223=EDGE_CURVE('',#7912,#7913,#5777,.T.);
#10224=EDGE_CURVE('',#7908,#7914,#5778,.T.);
#10225=EDGE_CURVE('',#7913,#7914,#3799,.T.);
#10226=EDGE_CURVE('',#7915,#7910,#5779,.T.);
#10227=EDGE_CURVE('',#7914,#7915,#5780,.T.);
#10228=EDGE_CURVE('',#7916,#7909,#214,.T.);
#10229=EDGE_CURVE('',#7910,#7916,#3800,.T.);
#10230=EDGE_CURVE('',#7894,#7916,#5781,.T.);
#10231=EDGE_CURVE('',#7911,#7893,#5782,.T.);
#10232=EDGE_CURVE('',#7891,#7917,#5783,.T.);
#10233=EDGE_CURVE('',#7917,#7918,#3801,.F.);
#10234=EDGE_CURVE('',#7918,#7894,#5784,.T.);
#10235=EDGE_CURVE('',#7917,#7898,#5785,.T.);
#10236=EDGE_CURVE('',#7919,#7916,#3802,.T.);
#10237=EDGE_CURVE('',#7916,#7920,#5786,.T.);
#10238=EDGE_CURVE('',#7920,#7870,#215,.F.);
#10239=EDGE_CURVE('',#7871,#7919,#5787,.T.);
#10240=EDGE_CURVE('',#7919,#7910,#3803,.T.);
#10241=EDGE_CURVE('',#7919,#7921,#5788,.T.);
#10242=EDGE_CURVE('',#7915,#7921,#3804,.T.);
#10243=EDGE_CURVE('',#7922,#7880,#3805,.F.);
#10244=EDGE_CURVE('',#7921,#7922,#5789,.T.);
#10245=EDGE_CURVE('',#7887,#7918,#5790,.T.);
#10246=EDGE_CURVE('',#7920,#7886,#5791,.T.);
#10247=EDGE_CURVE('',#7923,#7924,#216,.T.);
#10248=EDGE_CURVE('',#7924,#7925,#5792,.T.);
#10249=EDGE_CURVE('',#7925,#7926,#217,.F.);
#10250=EDGE_CURVE('',#7926,#7923,#5793,.T.);
#10251=EDGE_CURVE('',#7925,#7900,#5794,.T.);
#10252=EDGE_CURVE('',#7927,#7924,#5795,.T.);
#10253=EDGE_CURVE('',#7897,#7927,#5796,.T.);
#10254=EDGE_CURVE('',#7923,#7928,#218,.T.);
#10255=EDGE_CURVE('',#7928,#7882,#5099,.T.);
#10256=EDGE_CURVE('',#7924,#7883,#3806,.T.);
#10257=EDGE_CURVE('',#7885,#7924,#3807,.T.);
#10258=EDGE_CURVE('',#7928,#7929,#5797,.T.);
#10259=EDGE_CURVE('',#7929,#7922,#5100,.F.);
#10260=EDGE_CURVE('',#7912,#7902,#3808,.T.);
#10261=EDGE_CURVE('',#7885,#7930,#5798,.T.);
#10262=EDGE_CURVE('',#7930,#7931,#5101,.F.);
#10263=EDGE_CURVE('',#7931,#7927,#3809,.F.);
#10264=EDGE_CURVE('',#7929,#7926,#219,.F.);
#10265=EDGE_CURVE('',#7932,#7914,#3810,.T.);
#10266=EDGE_CURVE('',#7915,#7899,#3811,.T.);
#10267=EDGE_CURVE('',#7899,#7932,#5799,.T.);
#10268=EDGE_CURVE('',#7921,#7900,#3812,.T.);
#10269=EDGE_CURVE('',#7913,#7932,#3813,.T.);
#10270=EDGE_CURVE('',#7932,#7902,#5800,.T.);
#10271=EDGE_CURVE('',#7933,#7934,#3814,.T.);
#10272=EDGE_CURVE('',#7934,#7935,#3815,.T.);
#10273=EDGE_CURVE('',#7935,#7935,#3816,.T.);
#10274=EDGE_CURVE('',#7934,#7933,#3817,.T.);
#10275=EDGE_CURVE('',#7933,#7936,#5801,.T.);
#10276=EDGE_CURVE('',#7937,#7936,#3818,.T.);
#10277=EDGE_CURVE('',#7938,#7937,#5802,.T.);
#10278=EDGE_CURVE('',#7938,#7939,#3819,.T.);
#10279=EDGE_CURVE('',#7940,#7939,#5803,.T.);
#10280=EDGE_CURVE('',#7941,#7940,#3820,.T.);
#10281=EDGE_CURVE('',#7942,#7941,#5804,.T.);
#10282=EDGE_CURVE('',#7942,#7943,#3821,.T.);
#10283=EDGE_CURVE('',#7944,#7943,#5805,.T.);
#10284=EDGE_CURVE('',#7945,#7944,#3822,.T.);
#10285=EDGE_CURVE('',#7946,#7945,#5806,.T.);
#10286=EDGE_CURVE('',#7946,#7947,#3823,.T.);
#10287=EDGE_CURVE('',#7948,#7947,#5807,.T.);
#10288=EDGE_CURVE('',#7949,#7948,#3824,.T.);
#10289=EDGE_CURVE('',#7950,#7949,#5808,.T.);
#10290=EDGE_CURVE('',#7950,#7951,#3825,.T.);
#10291=EDGE_CURVE('',#7952,#7951,#5809,.T.);
#10292=EDGE_CURVE('',#7936,#7952,#3826,.T.);
#10293=EDGE_CURVE('',#7953,#7953,#3827,.T.);
#10294=EDGE_CURVE('',#7954,#7955,#5102,.T.);
#10295=EDGE_CURVE('',#7955,#7956,#5810,.T.);
#10296=EDGE_CURVE('',#7956,#7957,#3828,.T.);
#10297=EDGE_CURVE('',#7957,#7958,#5811,.T.);
#10298=EDGE_CURVE('',#7958,#7954,#5103,.T.);
#10299=EDGE_CURVE('',#7959,#7960,#3829,.T.);
#10300=EDGE_CURVE('',#7960,#7957,#3830,.T.);
#10301=EDGE_CURVE('',#7956,#7959,#3831,.T.);
#10302=EDGE_CURVE('',#7961,#7962,#3832,.T.);
#10303=EDGE_CURVE('',#7962,#7960,#5812,.T.);
#10304=EDGE_CURVE('',#7959,#7961,#5813,.T.);
#10305=EDGE_CURVE('',#7961,#7963,#3833,.T.);
#10306=EDGE_CURVE('',#7963,#7962,#3834,.T.);
#10307=EDGE_CURVE('',#7964,#7965,#3835,.T.);
#10308=EDGE_CURVE('',#7965,#7966,#3836,.T.);
#10309=EDGE_CURVE('',#7967,#7966,#3837,.T.);
#10310=EDGE_CURVE('',#7966,#7945,#3838,.T.);
#10311=EDGE_CURVE('',#7945,#7964,#3839,.T.);
#10312=EDGE_CURVE('',#7964,#7963,#5104,.T.);
#10313=EDGE_CURVE('',#7961,#7965,#5105,.T.);
#10314=EDGE_CURVE('',#7968,#7962,#3840,.T.);
#10315=EDGE_CURVE('',#7969,#7968,#5814,.T.);
#10316=EDGE_CURVE('',#7970,#7969,#3841,.T.);
#10317=EDGE_CURVE('',#7971,#7970,#5815,.T.);
#10318=EDGE_CURVE('',#7972,#7971,#3842,.T.);
#10319=EDGE_CURVE('',#7973,#7972,#5816,.T.);
#10320=EDGE_CURVE('',#7974,#7973,#3843,.T.);
#10321=EDGE_CURVE('',#7975,#7974,#5817,.T.);
#10322=EDGE_CURVE('',#7976,#7975,#3844,.T.);
#10323=EDGE_CURVE('',#7977,#7976,#5818,.T.);
#10324=EDGE_CURVE('',#7978,#7977,#3845,.T.);
#10325=EDGE_CURVE('',#7979,#7978,#5819,.T.);
#10326=EDGE_CURVE('',#7958,#7979,#3846,.T.);
#10327=EDGE_CURVE('',#7980,#7980,#3847,.T.);
#10328=EDGE_CURVE('',#7963,#7981,#3848,.T.);
#10329=EDGE_CURVE('',#7981,#7968,#3849,.T.);
#10330=EDGE_CURVE('',#7982,#7964,#3850,.T.);
#10331=EDGE_CURVE('',#7981,#7982,#5106,.T.);
#10332=EDGE_CURVE('',#7944,#7982,#3851,.T.);
#10333=EDGE_CURVE('',#7965,#7983,#5820,.T.);
#10334=EDGE_CURVE('',#7984,#7983,#3852,.T.);
#10335=EDGE_CURVE('',#7946,#7984,#5107,.T.);
#10336=EDGE_CURVE('',#7985,#7986,#5108,.T.);
#10337=EDGE_CURVE('',#7986,#7987,#5821,.T.);
#10338=EDGE_CURVE('',#7987,#7977,#3853,.T.);
#10339=EDGE_CURVE('',#7976,#7985,#5109,.T.);
#10340=EDGE_CURVE('',#7988,#7978,#3854,.T.);
#10341=EDGE_CURVE('',#7987,#7988,#3855,.T.);
#10342=EDGE_CURVE('',#7989,#7979,#5110,.T.);
#10343=EDGE_CURVE('',#7988,#7990,#5822,.T.);
#10344=EDGE_CURVE('',#7990,#7989,#220,.T.);
#10345=EDGE_CURVE('',#7975,#7991,#3856,.T.);
#10346=EDGE_CURVE('',#7991,#7985,#3857,.T.);
#10347=EDGE_CURVE('',#7989,#7992,#5111,.T.);
#10348=EDGE_CURVE('',#7992,#7954,#3858,.T.);
#10349=EDGE_CURVE('',#7993,#7955,#668,.T.);
#10350=EDGE_CURVE('',#7994,#7993,#5112,.T.);
#10351=EDGE_CURVE('',#7995,#7994,#5823,.T.);
#10352=EDGE_CURVE('',#7996,#7995,#5113,.F.);
#10353=EDGE_CURVE('',#7996,#7997,#5824,.T.);
#10354=EDGE_CURVE('',#7956,#7997,#5825,.T.);
#10355=EDGE_CURVE('',#7998,#7992,#5114,.T.);
#10356=EDGE_CURVE('',#7993,#7998,#3859,.T.);
#10357=EDGE_CURVE('',#7990,#7999,#5826,.T.);
#10358=EDGE_CURVE('',#8000,#7999,#3860,.T.);
#10359=EDGE_CURVE('',#7950,#8000,#5115,.T.);
#10360=EDGE_CURVE('',#7949,#7998,#5116,.T.);
#10361=EDGE_CURVE('',#8001,#8002,#3861,.T.);
#10362=EDGE_CURVE('',#8002,#7991,#5117,.T.);
#10363=EDGE_CURVE('',#7991,#8003,#3862,.T.);
#10364=EDGE_CURVE('',#8003,#8001,#5118,.T.);
#10365=EDGE_CURVE('',#7975,#8003,#3863,.T.);
#10366=EDGE_CURVE('',#7938,#8004,#5119,.T.);
#10367=EDGE_CURVE('',#7937,#8005,#3864,.T.);
#10368=EDGE_CURVE('',#8005,#8001,#3865,.T.);
#10369=EDGE_CURVE('',#8001,#8006,#5827,.T.);
#10370=EDGE_CURVE('',#8004,#8006,#3866,.T.);
#10371=EDGE_CURVE('',#7937,#8002,#3867,.T.);
#10372=EDGE_CURVE('',#8005,#8007,#3868,.T.);
#10373=EDGE_CURVE('',#8008,#7986,#669,.T.);
#10374=EDGE_CURVE('',#8009,#8008,#5120,.T.);
#10375=EDGE_CURVE('',#8010,#8009,#5828,.T.);
#10376=EDGE_CURVE('',#8011,#8010,#5121,.F.);
#10377=EDGE_CURVE('',#8011,#8012,#5829,.T.);
#10378=EDGE_CURVE('',#7987,#8012,#5830,.T.);
#10379=EDGE_CURVE('',#8008,#8002,#3869,.T.);
#10380=EDGE_CURVE('',#7952,#8009,#5122,.T.);
#10381=EDGE_CURVE('',#7951,#8010,#5123,.F.);
#10382=EDGE_CURVE('',#7988,#8013,#5831,.T.);
#10383=EDGE_CURVE('',#8013,#7999,#5832,.T.);
#10384=EDGE_CURVE('',#7948,#7994,#5124,.T.);
#10385=EDGE_CURVE('',#7947,#7995,#5125,.F.);
#10386=EDGE_CURVE('',#7959,#8014,#5833,.T.);
#10387=EDGE_CURVE('',#8014,#7983,#5834,.T.);
#10388=EDGE_CURVE('',#8015,#7981,#3870,.T.);
#10389=EDGE_CURVE('',#7982,#8016,#3871,.T.);
#10390=EDGE_CURVE('',#8016,#8015,#5126,.T.);
#10391=EDGE_CURVE('',#8015,#7968,#3872,.T.);
#10392=EDGE_CURVE('',#7944,#8016,#3873,.T.);
#10393=EDGE_CURVE('',#8015,#8017,#5835,.T.);
#10394=EDGE_CURVE('',#8017,#7969,#3874,.T.);
#10395=EDGE_CURVE('',#8018,#8016,#5836,.T.);
#10396=EDGE_CURVE('',#8019,#8018,#5127,.F.);
#10397=EDGE_CURVE('',#8019,#8020,#5837,.T.);
#10398=EDGE_CURVE('',#8017,#8020,#5838,.T.);
#10399=EDGE_CURVE('',#7943,#8018,#5128,.F.);
#10400=EDGE_CURVE('',#8021,#7940,#3875,.T.);
#10401=EDGE_CURVE('',#7939,#8022,#5129,.F.);
#10402=EDGE_CURVE('',#8022,#8021,#5839,.T.);
#10403=EDGE_CURVE('',#8023,#8024,#3876,.T.);
#10404=EDGE_CURVE('',#8024,#8025,#5130,.T.);
#10405=EDGE_CURVE('',#8025,#8021,#3877,.T.);
#10406=EDGE_CURVE('',#8021,#8023,#5131,.T.);
#10407=EDGE_CURVE('',#8023,#7972,#3878,.T.);
#10408=EDGE_CURVE('',#7972,#8024,#3879,.T.);
#10409=EDGE_CURVE('',#8025,#7940,#3880,.T.);
#10410=EDGE_CURVE('',#8025,#8026,#3881,.T.);
#10411=EDGE_CURVE('',#8026,#7941,#3882,.F.);
#10412=EDGE_CURVE('',#8027,#8024,#3883,.T.);
#10413=EDGE_CURVE('',#8026,#8027,#5132,.T.);
#10414=EDGE_CURVE('',#8004,#8028,#3884,.T.);
#10415=EDGE_CURVE('',#8028,#8022,#5133,.F.);
#10416=EDGE_CURVE('',#8029,#8006,#5840,.T.);
#10417=EDGE_CURVE('',#8030,#8029,#3885,.T.);
#10418=EDGE_CURVE('',#8028,#8030,#5841,.T.);
#10419=EDGE_CURVE('',#8031,#8031,#3886,.T.);
#10420=EDGE_CURVE('',#8032,#8026,#3887,.F.);
#10421=EDGE_CURVE('',#7941,#8032,#3888,.F.);
#10422=EDGE_CURVE('',#8027,#8033,#3889,.T.);
#10423=EDGE_CURVE('',#8033,#8032,#5134,.T.);
#10424=EDGE_CURVE('',#7942,#8034,#5135,.T.);
#10425=EDGE_CURVE('',#8032,#8035,#5842,.T.);
#10426=EDGE_CURVE('',#8034,#8035,#3890,.T.);
#10427=EDGE_CURVE('',#7971,#8027,#3891,.T.);
#10428=EDGE_CURVE('',#8023,#8036,#5843,.T.);
#10429=EDGE_CURVE('',#8036,#7973,#3892,.T.);
#10430=EDGE_CURVE('',#8037,#7974,#3893,.T.);
#10431=EDGE_CURVE('',#8036,#8037,#3894,.T.);
#10432=EDGE_CURVE('',#8037,#8003,#5844,.T.);
#10433=EDGE_CURVE('',#7971,#8033,#3895,.T.);
#10434=EDGE_CURVE('',#8036,#8030,#5845,.T.);
#10435=EDGE_CURVE('',#8038,#8033,#5846,.T.);
#10436=EDGE_CURVE('',#8038,#8039,#5847,.T.);
#10437=EDGE_CURVE('',#8039,#8035,#5848,.T.);
#10438=EDGE_CURVE('',#8038,#7970,#3896,.T.);
#10439=EDGE_CURVE('',#8017,#8038,#3897,.T.);
#10440=EDGE_CURVE('',#8020,#8039,#3898,.T.);
#10441=EDGE_CURVE('',#8031,#8040,#3899,.T.);
#10442=EDGE_CURVE('',#8040,#8040,#3900,.T.);
#10443=EDGE_CURVE('',#8040,#8041,#5849,.T.);
#10444=EDGE_CURVE('',#8042,#8041,#3901,.T.);
#10445=EDGE_CURVE('',#8041,#8042,#3902,.T.);
#10446=EDGE_CURVE('',#8043,#8044,#3903,.T.);
#10447=EDGE_CURVE('',#8044,#8045,#3904,.T.);
#10448=EDGE_CURVE('',#8045,#8043,#3905,.T.);
#10449=EDGE_CURVE('',#8046,#8047,#221,.F.);
#10450=EDGE_CURVE('',#8047,#8044,#5850,.T.);
#10451=EDGE_CURVE('',#8043,#8046,#5851,.T.);
#10452=EDGE_CURVE('',#8046,#8048,#5852,.T.);
#10453=EDGE_CURVE('',#8049,#8043,#5853,.T.);
#10454=EDGE_CURVE('',#8050,#8049,#5854,.T.);
#10455=EDGE_CURVE('',#8051,#8050,#5855,.T.);
#10456=EDGE_CURVE('',#8048,#8051,#5856,.T.);
#10457=EDGE_CURVE('',#8045,#8052,#5857,.T.);
#10458=EDGE_CURVE('',#8052,#8049,#3906,.F.);
#10459=EDGE_CURVE('',#8053,#8054,#222,.T.);
#10460=EDGE_CURVE('',#8054,#8055,#5858,.T.);
#10461=EDGE_CURVE('',#8055,#8056,#223,.T.);
#10462=EDGE_CURVE('',#8056,#8057,#224,.T.);
#10463=EDGE_CURVE('',#8057,#8058,#5859,.T.);
#10464=EDGE_CURVE('',#8058,#8053,#225,.T.);
#10465=EDGE_CURVE('',#8055,#8059,#5860,.T.);
#10466=EDGE_CURVE('',#8060,#8059,#3907,.T.);
#10467=EDGE_CURVE('',#8060,#8061,#5861,.T.);
#10468=EDGE_CURVE('',#8061,#8056,#226,.T.);
#10469=EDGE_CURVE('',#8062,#8054,#5862,.T.);
#10470=EDGE_CURVE('',#8059,#8062,#5863,.T.);
#10471=EDGE_CURVE('',#8053,#8063,#227,.T.);
#10472=EDGE_CURVE('',#8063,#8064,#5864,.T.);
#10473=EDGE_CURVE('',#8062,#8064,#3908,.T.);
#10474=EDGE_CURVE('',#8062,#8048,#3909,.T.);
#10475=EDGE_CURVE('',#8051,#8059,#3910,.T.);
#10476=EDGE_CURVE('',#8065,#8060,#5865,.T.);
#10477=EDGE_CURVE('',#8066,#8065,#5866,.T.);
#10478=EDGE_CURVE('',#8061,#8066,#5867,.T.);
#10479=EDGE_CURVE('',#8067,#8063,#5868,.T.);
#10480=EDGE_CURVE('',#8068,#8067,#228,.T.);
#10481=EDGE_CURVE('',#8064,#8068,#5869,.T.);
#10482=EDGE_CURVE('',#8058,#8069,#5870,.T.);
#10483=EDGE_CURVE('',#8069,#8070,#229,.T.);
#10484=EDGE_CURVE('',#8070,#8067,#5136,.T.);
#10485=EDGE_CURVE('',#7984,#7996,#3911,.T.);
#10486=EDGE_CURVE('',#7997,#8014,#3912,.T.);
#10487=EDGE_CURVE('',#8071,#8071,#3913,.T.);
#10488=EDGE_CURVE('',#8071,#8072,#3914,.T.);
#10489=EDGE_CURVE('',#8072,#8072,#3915,.T.);
#10490=EDGE_CURVE('',#8072,#8073,#5871,.T.);
#10491=EDGE_CURVE('',#8074,#8073,#3916,.T.);
#10492=EDGE_CURVE('',#8073,#8074,#3917,.T.);
#10493=EDGE_CURVE('',#8075,#8051,#3918,.T.);
#10494=EDGE_CURVE('',#8050,#8076,#3919,.F.);
#10495=EDGE_CURVE('',#8076,#8075,#5872,.T.);
#10496=EDGE_CURVE('',#8075,#8060,#3920,.T.);
#10497=EDGE_CURVE('',#8048,#8077,#3921,.T.);
#10498=EDGE_CURVE('',#8077,#8047,#5873,.T.);
#10499=EDGE_CURVE('',#8064,#8077,#3922,.T.);
#10500=EDGE_CURVE('',#8075,#8078,#5874,.T.);
#10501=EDGE_CURVE('',#8078,#8065,#3923,.T.);
#10502=EDGE_CURVE('',#8079,#8080,#3924,.T.);
#10503=EDGE_CURVE('',#8079,#8065,#3925,.T.);
#10504=EDGE_CURVE('',#8078,#8080,#3926,.T.);
#10505=EDGE_CURVE('',#8078,#8081,#5875,.T.);
#10506=EDGE_CURVE('',#8081,#8082,#3927,.F.);
#10507=EDGE_CURVE('',#8082,#8080,#5876,.T.);
#10508=EDGE_CURVE('',#8081,#8076,#5877,.T.);
#10509=EDGE_CURVE('',#8066,#8083,#3928,.T.);
#10510=EDGE_CURVE('',#8083,#8057,#5878,.T.);
#10511=EDGE_CURVE('',#8079,#8084,#5879,.T.);
#10512=EDGE_CURVE('',#8084,#8066,#3929,.T.);
#10513=EDGE_CURVE('',#8084,#8083,#3930,.T.);
#10514=EDGE_CURVE('',#8069,#8083,#5880,.T.);
#10515=EDGE_CURVE('',#8084,#8085,#5881,.T.);
#10516=EDGE_CURVE('',#8085,#8070,#230,.T.);
#10517=EDGE_CURVE('',#8086,#8079,#5882,.T.);
#10518=EDGE_CURVE('',#8085,#8086,#5883,.T.);
#10519=EDGE_CURVE('',#8087,#8088,#3931,.T.);
#10520=EDGE_CURVE('',#8088,#8089,#3932,.T.);
#10521=EDGE_CURVE('',#8089,#8089,#3933,.T.);
#10522=EDGE_CURVE('',#8088,#8087,#3934,.T.);
#10523=EDGE_CURVE('',#8090,#8091,#3935,.T.);
#10524=EDGE_CURVE('',#8090,#8087,#5884,.T.);
#10525=EDGE_CURVE('',#8091,#8090,#3936,.T.);
#10526=EDGE_CURVE('',#8092,#8092,#3937,.T.);
#10527=EDGE_CURVE('',#8093,#8094,#3938,.T.);
#10528=EDGE_CURVE('',#8094,#8093,#3939,.T.);
#10529=EDGE_CURVE('',#8093,#8091,#3940,.T.);
#10530=EDGE_CURVE('',#8095,#8096,#3941,.T.);
#10531=EDGE_CURVE('',#8095,#8094,#5885,.T.);
#10532=EDGE_CURVE('',#8096,#8095,#3942,.T.);
#10533=EDGE_CURVE('',#8000,#8011,#3943,.T.);
#10534=EDGE_CURVE('',#8012,#8013,#3944,.T.);
#10535=EDGE_CURVE('',#8097,#8097,#3945,.T.);
#10536=EDGE_CURVE('',#8034,#8019,#3946,.T.);
#10537=EDGE_CURVE('',#8098,#8098,#3947,.T.);
#10538=EDGE_CURVE('',#8099,#8086,#3948,.T.);
#10539=EDGE_CURVE('',#8068,#8099,#231,.T.);
#10540=EDGE_CURVE('',#8099,#8077,#5886,.T.);
#10541=EDGE_CURVE('',#8100,#8099,#5887,.T.);
#10542=EDGE_CURVE('',#8100,#8047,#5888,.T.);
#10543=EDGE_CURVE('',#8080,#8101,#5889,.T.);
#10544=EDGE_CURVE('',#8101,#8086,#3949,.T.);
#10545=EDGE_CURVE('',#8101,#8099,#3950,.T.);
#10546=EDGE_CURVE('',#8102,#8082,#5890,.T.);
#10547=EDGE_CURVE('',#8103,#8102,#5891,.T.);
#10548=EDGE_CURVE('',#8104,#8103,#5892,.T.);
#10549=EDGE_CURVE('',#8101,#8104,#5893,.T.);
#10550=EDGE_CURVE('',#8104,#8100,#232,.F.);
#10551=EDGE_CURVE('',#8098,#8105,#3951,.T.);
#10552=EDGE_CURVE('',#8105,#8105,#3952,.T.);
#10553=EDGE_CURVE('',#8105,#8106,#5894,.T.);
#10554=EDGE_CURVE('',#8107,#8106,#3953,.T.);
#10555=EDGE_CURVE('',#8106,#8107,#3954,.T.);
#10556=EDGE_CURVE('',#8097,#8108,#3955,.T.);
#10557=EDGE_CURVE('',#8108,#8108,#3956,.T.);
#10558=EDGE_CURVE('',#8108,#8109,#5895,.T.);
#10559=EDGE_CURVE('',#8110,#8109,#3957,.T.);
#10560=EDGE_CURVE('',#8109,#8110,#3958,.T.);
#10561=EDGE_CURVE('',#8111,#8111,#3959,.T.);
#10562=EDGE_CURVE('',#8111,#8112,#3960,.T.);
#10563=EDGE_CURVE('',#8112,#8113,#3961,.T.);
#10564=EDGE_CURVE('',#8113,#8112,#3962,.T.);
#10565=EDGE_CURVE('',#8114,#8114,#3963,.T.);
#10566=EDGE_CURVE('',#8115,#8115,#3964,.T.);
#10567=EDGE_CURVE('',#8116,#8116,#3965,.T.);
#10568=EDGE_CURVE('',#8117,#8117,#3966,.T.);
#10569=EDGE_CURVE('',#8118,#8118,#3967,.T.);
#10570=EDGE_CURVE('',#8119,#8119,#3968,.T.);
#10571=EDGE_CURVE('',#8120,#8120,#3969,.T.);
#10572=EDGE_CURVE('',#8121,#8121,#3970,.T.);
#10573=EDGE_CURVE('',#8122,#8122,#3971,.T.);
#10574=EDGE_CURVE('',#8123,#8123,#3972,.T.);
#10575=EDGE_CURVE('',#8124,#8124,#3973,.T.);
#10576=EDGE_CURVE('',#8125,#8125,#3974,.T.);
#10577=EDGE_CURVE('',#8125,#8113,#5896,.T.);
#10578=EDGE_CURVE('',#8115,#8126,#3975,.T.);
#10579=EDGE_CURVE('',#8126,#8127,#3976,.T.);
#10580=EDGE_CURVE('',#8127,#8126,#3977,.T.);
#10581=EDGE_CURVE('',#8128,#8128,#3978,.T.);
#10582=EDGE_CURVE('',#8128,#8127,#5897,.T.);
#10583=EDGE_CURVE('',#8114,#8096,#3979,.T.);
#10584=EDGE_CURVE('',#8116,#8074,#3980,.T.);
#10585=EDGE_CURVE('',#8124,#8042,#3981,.T.);
#10586=EDGE_CURVE('',#8117,#8129,#3982,.T.);
#10587=EDGE_CURVE('',#8129,#8130,#3983,.T.);
#10588=EDGE_CURVE('',#8130,#8129,#3984,.T.);
#10589=EDGE_CURVE('',#8131,#8131,#3985,.T.);
#10590=EDGE_CURVE('',#8131,#8130,#5898,.T.);
#10591=EDGE_CURVE('',#8123,#8110,#3986,.T.);
#10592=EDGE_CURVE('',#8118,#8107,#3987,.T.);
#10593=EDGE_CURVE('',#8132,#8132,#3988,.T.);
#10594=EDGE_CURVE('',#8132,#8133,#3989,.T.);
#10595=EDGE_CURVE('',#8133,#8133,#3990,.T.);
#10596=EDGE_CURVE('',#8134,#8134,#3991,.T.);
#10597=EDGE_CURVE('',#8134,#8132,#5899,.T.);
#10598=EDGE_CURVE('',#8135,#8135,#3992,.T.);
#10599=EDGE_CURVE('',#8136,#8136,#3993,.T.);
#10600=EDGE_CURVE('',#8136,#8137,#3994,.T.);
#10601=EDGE_CURVE('',#8137,#8137,#3995,.T.);
#10602=EDGE_CURVE('',#8138,#8138,#3996,.T.);
#10603=EDGE_CURVE('',#8138,#8136,#5900,.T.);
#10604=EDGE_CURVE('',#8139,#8139,#3997,.T.);
#10605=EDGE_CURVE('',#8140,#8140,#3998,.T.);
#10606=EDGE_CURVE('',#8140,#8141,#3999,.T.);
#10607=EDGE_CURVE('',#8141,#8141,#4000,.T.);
#10608=EDGE_CURVE('',#8142,#8142,#4001,.T.);
#10609=EDGE_CURVE('',#8142,#8140,#5901,.T.);
#10610=EDGE_CURVE('',#8143,#8143,#4002,.T.);
#10611=EDGE_CURVE('',#8044,#8144,#5902,.T.);
#10612=EDGE_CURVE('',#8144,#8145,#4003,.T.);
#10613=EDGE_CURVE('',#8145,#8045,#5903,.T.);
#10614=EDGE_CURVE('',#8103,#8144,#4004,.T.);
#10615=EDGE_CURVE('',#8144,#8100,#5904,.T.);
#10616=EDGE_CURVE('',#8103,#8145,#4005,.T.);
#10617=EDGE_CURVE('',#8052,#8146,#5905,.T.);
#10618=EDGE_CURVE('',#8147,#8145,#5906,.T.);
#10619=EDGE_CURVE('',#8148,#8147,#5137,.F.);
#10620=EDGE_CURVE('',#8149,#8148,#5907,.T.);
#10621=EDGE_CURVE('',#8150,#8149,#5138,.F.);
#10622=EDGE_CURVE('',#8150,#8146,#670,.T.);
#10623=EDGE_CURVE('',#8151,#8102,#4006,.T.);
#10624=EDGE_CURVE('',#8147,#8151,#5139,.T.);
#10625=EDGE_CURVE('',#8152,#8153,#4007,.T.);
#10626=EDGE_CURVE('',#8153,#8152,#4008,.T.);
#10627=EDGE_CURVE('',#8152,#8154,#4009,.T.);
#10628=EDGE_CURVE('',#8154,#8155,#4010,.T.);
#10629=EDGE_CURVE('',#8155,#8154,#4011,.T.);
#10630=EDGE_CURVE('',#8155,#8156,#5908,.T.);
#10631=EDGE_CURVE('',#8157,#8156,#4012,.T.);
#10632=EDGE_CURVE('',#8156,#8157,#4013,.T.);
#10633=EDGE_CURVE('',#8158,#8159,#4014,.T.);
#10634=EDGE_CURVE('',#8158,#8153,#5909,.T.);
#10635=EDGE_CURVE('',#8159,#8158,#4015,.T.);
#10636=EDGE_CURVE('',#8157,#8160,#4016,.T.);
#10637=EDGE_CURVE('',#8160,#8160,#4017,.T.);
#10638=EDGE_CURVE('',#8161,#8161,#4018,.T.);
#10639=EDGE_CURVE('',#8162,#8162,#4019,.T.);
#10640=EDGE_CURVE('',#8163,#8163,#4020,.T.);
#10641=EDGE_CURVE('',#8164,#8164,#4021,.T.);
#10642=EDGE_CURVE('',#8165,#8165,#4022,.T.);
#10643=EDGE_CURVE('',#8166,#8166,#4023,.T.);
#10644=EDGE_CURVE('',#8167,#8167,#4024,.T.);
#10645=EDGE_CURVE('',#8161,#8142,#4025,.T.);
#10646=EDGE_CURVE('',#8167,#8138,#4026,.T.);
#10647=EDGE_CURVE('',#8162,#8134,#4027,.T.);
#10648=EDGE_CURVE('',#8168,#8169,#4028,.T.);
#10649=EDGE_CURVE('',#8169,#8168,#4029,.T.);
#10650=EDGE_CURVE('',#8168,#8122,#4030,.T.);
#10651=EDGE_CURVE('',#8169,#8170,#5910,.T.);
#10652=EDGE_CURVE('',#8171,#8170,#4031,.T.);
#10653=EDGE_CURVE('',#8170,#8171,#4032,.T.);
#10654=EDGE_CURVE('',#8172,#8173,#4033,.T.);
#10655=EDGE_CURVE('',#8173,#7980,#4034,.T.);
#10656=EDGE_CURVE('',#8173,#8172,#4035,.T.);
#10657=EDGE_CURVE('',#8172,#8174,#5911,.T.);
#10658=EDGE_CURVE('',#8175,#8174,#4036,.T.);
#10659=EDGE_CURVE('',#8174,#8175,#4037,.T.);
#10660=EDGE_CURVE('',#8175,#8171,#4038,.T.);
#10661=EDGE_CURVE('',#8166,#8176,#4039,.T.);
#10662=EDGE_CURVE('',#8176,#8177,#4040,.T.);
#10663=EDGE_CURVE('',#8177,#8176,#4041,.T.);
#10664=EDGE_CURVE('',#8178,#8179,#4042,.T.);
#10665=EDGE_CURVE('',#8178,#8177,#5912,.T.);
#10666=EDGE_CURVE('',#8179,#8178,#4043,.T.);
#10667=EDGE_CURVE('',#8180,#8181,#4044,.T.);
#10668=EDGE_CURVE('',#8181,#8180,#4045,.T.);
#10669=EDGE_CURVE('',#8180,#8159,#4046,.T.);
#10670=EDGE_CURVE('',#8182,#8150,#4047,.T.);
#10671=EDGE_CURVE('',#8182,#8181,#5913,.T.);
#10672=EDGE_CURVE('',#8183,#8182,#4048,.T.);
#10673=EDGE_CURVE('',#8184,#8183,#671,.T.);
#10674=EDGE_CURVE('',#8146,#8184,#4049,.T.);
#10675=EDGE_CURVE('',#8151,#7799,#4050,.F.);
#10676=EDGE_CURVE('',#7818,#7817,#4051,.T.);
#10677=EDGE_CURVE('',#7819,#7860,#4052,.F.);
#10678=EDGE_CURVE('',#7857,#7856,#4053,.T.);
#10679=EDGE_CURVE('',#7850,#7931,#4054,.F.);
#10680=EDGE_CURVE('',#8185,#7930,#5140,.T.);
#10681=EDGE_CURVE('',#8185,#8186,#4055,.T.);
#10682=EDGE_CURVE('',#8183,#8186,#5141,.T.);
#10683=EDGE_CURVE('',#8149,#8148,#4056,.T.);
#10684=EDGE_CURVE('',#8187,#8187,#4057,.T.);
#10685=EDGE_CURVE('',#8187,#8188,#4058,.T.);
#10686=EDGE_CURVE('',#8188,#8189,#4059,.T.);
#10687=EDGE_CURVE('',#8189,#8188,#4060,.T.);
#10688=EDGE_CURVE('',#8184,#7888,#5914,.T.);
#10689=EDGE_CURVE('',#7807,#7792,#5915,.T.);
#10690=EDGE_CURVE('',#8190,#8190,#4061,.T.);
#10691=EDGE_CURVE('',#8191,#8191,#4062,.T.);
#10692=EDGE_CURVE('',#8192,#8192,#4063,.T.);
#10693=EDGE_CURVE('',#8143,#8189,#5916,.T.);
#10694=EDGE_CURVE('',#8190,#8193,#4064,.T.);
#10695=EDGE_CURVE('',#8193,#8194,#4065,.T.);
#10696=EDGE_CURVE('',#8194,#8193,#4066,.T.);
#10697=EDGE_CURVE('',#8139,#8194,#5917,.T.);
#10698=EDGE_CURVE('',#8192,#8195,#4067,.T.);
#10699=EDGE_CURVE('',#8195,#8196,#4068,.T.);
#10700=EDGE_CURVE('',#8196,#8195,#4069,.T.);
#10701=EDGE_CURVE('',#8135,#8196,#5918,.T.);
#10702=EDGE_CURVE('',#8197,#8198,#4070,.T.);
#10703=EDGE_CURVE('',#8198,#8179,#4071,.T.);
#10704=EDGE_CURVE('',#8198,#8197,#4072,.T.);
#10705=EDGE_CURVE('',#8197,#8199,#5919,.T.);
#10706=EDGE_CURVE('',#8200,#8199,#4073,.T.);
#10707=EDGE_CURVE('',#8199,#8200,#4074,.T.);
#10708=EDGE_CURVE('',#8200,#8191,#4075,.T.);
#10709=EDGE_CURVE('',#8037,#8029,#5920,.T.);
#10710=EDGE_CURVE('',#8185,#8186,#5921,.T.);
#10711=EDGE_CURVE('',#7953,#8092,#5922,.T.);
#10712=EDGE_CURVE('',#8163,#8119,#5923,.T.);
#10713=EDGE_CURVE('',#8164,#8120,#5924,.T.);
#10714=EDGE_CURVE('',#8165,#8121,#5925,.T.);
#10715=EDGE_CURVE('',#8201,#8202,#4076,.T.);
#10716=EDGE_CURVE('',#8202,#8201,#4077,.T.);
#10717=EDGE_CURVE('',#8201,#8203,#5926,.T.);
#10718=EDGE_CURVE('',#8203,#8203,#4078,.T.);
#10719=EDGE_CURVE('',#8202,#8204,#5927,.T.);
#10720=EDGE_CURVE('',#8205,#8204,#4079,.T.);
#10721=EDGE_CURVE('',#8204,#8205,#4080,.T.);
#10722=EDGE_CURVE('',#8206,#8207,#672,.T.);
#10723=EDGE_CURVE('',#8207,#8208,#4081,.T.);
#10724=EDGE_CURVE('',#8208,#8209,#673,.T.);
#10725=EDGE_CURVE('',#8209,#8210,#4082,.T.);
#10726=EDGE_CURVE('',#8210,#8211,#674,.T.);
#10727=EDGE_CURVE('',#8211,#8212,#4083,.T.);
#10728=EDGE_CURVE('',#8212,#8213,#675,.T.);
#10729=EDGE_CURVE('',#8213,#8214,#4084,.T.);
#10730=EDGE_CURVE('',#8214,#8215,#676,.T.);
#10731=EDGE_CURVE('',#8215,#8216,#4085,.T.);
#10732=EDGE_CURVE('',#8216,#8217,#677,.T.);
#10733=EDGE_CURVE('',#8217,#8218,#4086,.T.);
#10734=EDGE_CURVE('',#8218,#8219,#678,.T.);
#10735=EDGE_CURVE('',#8219,#8220,#4087,.T.);
#10736=EDGE_CURVE('',#8220,#8221,#679,.T.);
#10737=EDGE_CURVE('',#8221,#8222,#4088,.T.);
#10738=EDGE_CURVE('',#8222,#8223,#680,.T.);
#10739=EDGE_CURVE('',#8223,#8224,#4089,.T.);
#10740=EDGE_CURVE('',#8224,#8225,#681,.T.);
#10741=EDGE_CURVE('',#8225,#8226,#4090,.T.);
#10742=EDGE_CURVE('',#8226,#8227,#682,.T.);
#10743=EDGE_CURVE('',#8227,#8228,#4091,.T.);
#10744=EDGE_CURVE('',#8228,#8229,#683,.T.);
#10745=EDGE_CURVE('',#8229,#8230,#4092,.T.);
#10746=EDGE_CURVE('',#8230,#8231,#684,.T.);
#10747=EDGE_CURVE('',#8231,#8232,#4093,.T.);
#10748=EDGE_CURVE('',#8232,#8233,#685,.T.);
#10749=EDGE_CURVE('',#8233,#8234,#4094,.T.);
#10750=EDGE_CURVE('',#8234,#8235,#686,.T.);
#10751=EDGE_CURVE('',#8235,#8236,#4095,.T.);
#10752=EDGE_CURVE('',#8236,#8237,#687,.T.);
#10753=EDGE_CURVE('',#8237,#8238,#4096,.T.);
#10754=EDGE_CURVE('',#8238,#8239,#688,.T.);
#10755=EDGE_CURVE('',#8239,#8240,#4097,.T.);
#10756=EDGE_CURVE('',#8240,#8241,#689,.T.);
#10757=EDGE_CURVE('',#8241,#8242,#4098,.T.);
#10758=EDGE_CURVE('',#8242,#8243,#690,.T.);
#10759=EDGE_CURVE('',#8243,#8244,#4099,.T.);
#10760=EDGE_CURVE('',#8244,#8245,#691,.T.);
#10761=EDGE_CURVE('',#8245,#8246,#4100,.T.);
#10762=EDGE_CURVE('',#8246,#8247,#692,.T.);
#10763=EDGE_CURVE('',#8247,#8248,#4101,.T.);
#10764=EDGE_CURVE('',#8248,#8249,#693,.T.);
#10765=EDGE_CURVE('',#8249,#8250,#4102,.T.);
#10766=EDGE_CURVE('',#8250,#8251,#694,.T.);
#10767=EDGE_CURVE('',#8251,#8252,#4103,.T.);
#10768=EDGE_CURVE('',#8252,#8253,#695,.T.);
#10769=EDGE_CURVE('',#8253,#8254,#4104,.T.);
#10770=EDGE_CURVE('',#8254,#8255,#696,.T.);
#10771=EDGE_CURVE('',#8255,#8256,#4105,.T.);
#10772=EDGE_CURVE('',#8256,#8257,#697,.T.);
#10773=EDGE_CURVE('',#8257,#8258,#4106,.T.);
#10774=EDGE_CURVE('',#8258,#8259,#698,.T.);
#10775=EDGE_CURVE('',#8259,#8260,#4107,.T.);
#10776=EDGE_CURVE('',#8260,#8261,#699,.T.);
#10777=EDGE_CURVE('',#8261,#8206,#4108,.T.);
#10778=EDGE_CURVE('',#8262,#8262,#4109,.T.);
#10779=EDGE_CURVE('',#8262,#8205,#5928,.T.);
#10780=EDGE_CURVE('',#8263,#8264,#700,.T.);
#10781=EDGE_CURVE('',#8264,#8265,#4110,.T.);
#10782=EDGE_CURVE('',#8265,#8266,#701,.T.);
#10783=EDGE_CURVE('',#8267,#8266,#4111,.T.);
#10784=EDGE_CURVE('',#8267,#8268,#702,.T.);
#10785=EDGE_CURVE('',#8268,#8269,#4112,.T.);
#10786=EDGE_CURVE('',#8269,#8270,#703,.T.);
#10787=EDGE_CURVE('',#8271,#8270,#4113,.T.);
#10788=EDGE_CURVE('',#8271,#8272,#704,.T.);
#10789=EDGE_CURVE('',#8272,#8273,#4114,.T.);
#10790=EDGE_CURVE('',#8273,#8274,#705,.T.);
#10791=EDGE_CURVE('',#8275,#8274,#4115,.T.);
#10792=EDGE_CURVE('',#8275,#8276,#706,.T.);
#10793=EDGE_CURVE('',#8276,#8277,#4116,.T.);
#10794=EDGE_CURVE('',#8277,#8278,#707,.T.);
#10795=EDGE_CURVE('',#8279,#8278,#4117,.T.);
#10796=EDGE_CURVE('',#8279,#8280,#708,.T.);
#10797=EDGE_CURVE('',#8280,#8281,#4118,.T.);
#10798=EDGE_CURVE('',#8281,#8282,#709,.T.);
#10799=EDGE_CURVE('',#8283,#8282,#4119,.T.);
#10800=EDGE_CURVE('',#8283,#8284,#710,.T.);
#10801=EDGE_CURVE('',#8284,#8285,#4120,.T.);
#10802=EDGE_CURVE('',#8285,#8286,#711,.T.);
#10803=EDGE_CURVE('',#8287,#8286,#4121,.T.);
#10804=EDGE_CURVE('',#8287,#8288,#712,.T.);
#10805=EDGE_CURVE('',#8288,#8289,#4122,.T.);
#10806=EDGE_CURVE('',#8289,#8290,#713,.T.);
#10807=EDGE_CURVE('',#8291,#8290,#4123,.T.);
#10808=EDGE_CURVE('',#8291,#8292,#714,.T.);
#10809=EDGE_CURVE('',#8292,#8293,#4124,.T.);
#10810=EDGE_CURVE('',#8293,#8294,#715,.T.);
#10811=EDGE_CURVE('',#8295,#8294,#4125,.T.);
#10812=EDGE_CURVE('',#8295,#8296,#716,.T.);
#10813=EDGE_CURVE('',#8296,#8297,#4126,.T.);
#10814=EDGE_CURVE('',#8297,#8298,#717,.T.);
#10815=EDGE_CURVE('',#8299,#8298,#4127,.T.);
#10816=EDGE_CURVE('',#8299,#8300,#718,.T.);
#10817=EDGE_CURVE('',#8300,#8301,#4128,.T.);
#10818=EDGE_CURVE('',#8301,#8302,#719,.T.);
#10819=EDGE_CURVE('',#8303,#8302,#4129,.T.);
#10820=EDGE_CURVE('',#8303,#8304,#720,.T.);
#10821=EDGE_CURVE('',#8304,#8305,#4130,.T.);
#10822=EDGE_CURVE('',#8305,#8306,#721,.T.);
#10823=EDGE_CURVE('',#8307,#8306,#4131,.T.);
#10824=EDGE_CURVE('',#8307,#8308,#722,.T.);
#10825=EDGE_CURVE('',#8308,#8309,#4132,.T.);
#10826=EDGE_CURVE('',#8309,#8310,#723,.T.);
#10827=EDGE_CURVE('',#8311,#8310,#4133,.T.);
#10828=EDGE_CURVE('',#8311,#8312,#724,.T.);
#10829=EDGE_CURVE('',#8312,#8313,#4134,.T.);
#10830=EDGE_CURVE('',#8313,#8314,#725,.T.);
#10831=EDGE_CURVE('',#8315,#8314,#4135,.T.);
#10832=EDGE_CURVE('',#8315,#8316,#726,.T.);
#10833=EDGE_CURVE('',#8316,#8317,#4136,.T.);
#10834=EDGE_CURVE('',#8317,#8318,#727,.T.);
#10835=EDGE_CURVE('',#8319,#8318,#4137,.T.);
#10836=EDGE_CURVE('',#8319,#8320,#728,.T.);
#10837=EDGE_CURVE('',#8320,#8321,#4138,.T.);
#10838=EDGE_CURVE('',#8321,#8322,#729,.T.);
#10839=EDGE_CURVE('',#8323,#8322,#4139,.T.);
#10840=EDGE_CURVE('',#8323,#8324,#730,.T.);
#10841=EDGE_CURVE('',#8324,#8325,#4140,.T.);
#10842=EDGE_CURVE('',#8325,#8326,#731,.T.);
#10843=EDGE_CURVE('',#8327,#8326,#4141,.T.);
#10844=EDGE_CURVE('',#8327,#8328,#732,.T.);
#10845=EDGE_CURVE('',#8328,#8329,#4142,.T.);
#10846=EDGE_CURVE('',#8329,#8330,#733,.T.);
#10847=EDGE_CURVE('',#8331,#8330,#4143,.T.);
#10848=EDGE_CURVE('',#8331,#8332,#734,.T.);
#10849=EDGE_CURVE('',#8332,#8333,#4144,.T.);
#10850=EDGE_CURVE('',#8333,#8334,#735,.T.);
#10851=EDGE_CURVE('',#8335,#8334,#4145,.T.);
#10852=EDGE_CURVE('',#8335,#8336,#736,.T.);
#10853=EDGE_CURVE('',#8336,#8337,#4146,.T.);
#10854=EDGE_CURVE('',#8337,#8338,#737,.T.);
#10855=EDGE_CURVE('',#8339,#8338,#4147,.T.);
#10856=EDGE_CURVE('',#8339,#8340,#738,.T.);
#10857=EDGE_CURVE('',#8340,#8341,#4148,.T.);
#10858=EDGE_CURVE('',#8341,#8342,#739,.T.);
#10859=EDGE_CURVE('',#8343,#8342,#4149,.T.);
#10860=EDGE_CURVE('',#8343,#8344,#740,.T.);
#10861=EDGE_CURVE('',#8344,#8345,#4150,.T.);
#10862=EDGE_CURVE('',#8345,#8346,#741,.T.);
#10863=EDGE_CURVE('',#8347,#8346,#4151,.T.);
#10864=EDGE_CURVE('',#8347,#8348,#742,.T.);
#10865=EDGE_CURVE('',#8348,#8349,#4152,.T.);
#10866=EDGE_CURVE('',#8349,#8350,#743,.T.);
#10867=EDGE_CURVE('',#8351,#8350,#4153,.T.);
#10868=EDGE_CURVE('',#8351,#8352,#744,.T.);
#10869=EDGE_CURVE('',#8352,#8353,#4154,.T.);
#10870=EDGE_CURVE('',#8353,#8354,#745,.T.);
#10871=EDGE_CURVE('',#8355,#8354,#4155,.T.);
#10872=EDGE_CURVE('',#8355,#8356,#746,.T.);
#10873=EDGE_CURVE('',#8356,#8357,#4156,.T.);
#10874=EDGE_CURVE('',#8357,#8358,#747,.T.);
#10875=EDGE_CURVE('',#8359,#8358,#4157,.T.);
#10876=EDGE_CURVE('',#8359,#8360,#748,.T.);
#10877=EDGE_CURVE('',#8360,#8361,#4158,.T.);
#10878=EDGE_CURVE('',#8361,#8362,#749,.T.);
#10879=EDGE_CURVE('',#8263,#8362,#4159,.T.);
#10880=EDGE_CURVE('',#8209,#8363,#5142,.T.);
#10881=EDGE_CURVE('',#8364,#8208,#5929,.T.);
#10882=EDGE_CURVE('',#8364,#8365,#750,.T.);
#10883=EDGE_CURVE('',#8363,#8365,#5143,.T.);
#10884=EDGE_CURVE('',#8366,#8364,#4160,.T.);
#10885=EDGE_CURVE('',#8366,#8207,#5930,.T.);
#10886=EDGE_CURVE('',#8367,#8206,#5144,.T.);
#10887=EDGE_CURVE('',#8368,#8367,#5145,.T.);
#10888=EDGE_CURVE('',#8368,#8366,#751,.T.);
#10889=EDGE_CURVE('',#8363,#8369,#4161,.T.);
#10890=EDGE_CURVE('',#8369,#8210,#5146,.T.);
#10891=EDGE_CURVE('',#8365,#8370,#4162,.T.);
#10892=EDGE_CURVE('',#8370,#8369,#5147,.T.);
#10893=EDGE_CURVE('',#8371,#8372,#5148,.T.);
#10894=EDGE_CURVE('',#8371,#8373,#752,.T.);
#10895=EDGE_CURVE('',#8373,#8259,#5931,.T.);
#10896=EDGE_CURVE('',#8372,#8258,#5149,.T.);
#10897=EDGE_CURVE('',#8373,#8374,#4163,.T.);
#10898=EDGE_CURVE('',#8374,#8260,#5932,.T.);
#10899=EDGE_CURVE('',#8375,#8376,#5150,.T.);
#10900=EDGE_CURVE('',#8261,#8375,#5151,.T.);
#10901=EDGE_CURVE('',#8374,#8376,#753,.T.);
#10902=EDGE_CURVE('',#8377,#8378,#754,.T.);
#10903=EDGE_CURVE('',#8378,#8379,#4164,.T.);
#10904=EDGE_CURVE('',#8379,#8380,#755,.T.);
#10905=EDGE_CURVE('',#8380,#8381,#4165,.T.);
#10906=EDGE_CURVE('',#8381,#8382,#756,.T.);
#10907=EDGE_CURVE('',#8382,#8383,#4166,.T.);
#10908=EDGE_CURVE('',#8383,#8384,#757,.T.);
#10909=EDGE_CURVE('',#8384,#8385,#4167,.T.);
#10910=EDGE_CURVE('',#8385,#8386,#758,.T.);
#10911=EDGE_CURVE('',#8386,#8387,#4168,.T.);
#10912=EDGE_CURVE('',#8387,#8388,#759,.T.);
#10913=EDGE_CURVE('',#8388,#8389,#4169,.T.);
#10914=EDGE_CURVE('',#8389,#8390,#760,.T.);
#10915=EDGE_CURVE('',#8390,#8391,#4170,.T.);
#10916=EDGE_CURVE('',#8391,#8392,#761,.T.);
#10917=EDGE_CURVE('',#8392,#8393,#4171,.T.);
#10918=EDGE_CURVE('',#8393,#8394,#762,.T.);
#10919=EDGE_CURVE('',#8394,#8395,#4172,.T.);
#10920=EDGE_CURVE('',#8395,#8396,#763,.T.);
#10921=EDGE_CURVE('',#8396,#8397,#4173,.T.);
#10922=EDGE_CURVE('',#8397,#8398,#764,.T.);
#10923=EDGE_CURVE('',#8398,#8399,#4174,.T.);
#10924=EDGE_CURVE('',#8399,#8400,#765,.T.);
#10925=EDGE_CURVE('',#8400,#8401,#4175,.T.);
#10926=EDGE_CURVE('',#8401,#8402,#766,.T.);
#10927=EDGE_CURVE('',#8402,#8403,#4176,.T.);
#10928=EDGE_CURVE('',#8403,#8404,#767,.T.);
#10929=EDGE_CURVE('',#8404,#8405,#4177,.T.);
#10930=EDGE_CURVE('',#8405,#8406,#768,.T.);
#10931=EDGE_CURVE('',#8406,#8407,#4178,.T.);
#10932=EDGE_CURVE('',#8407,#8408,#769,.T.);
#10933=EDGE_CURVE('',#8408,#8409,#4179,.T.);
#10934=EDGE_CURVE('',#8409,#8410,#770,.T.);
#10935=EDGE_CURVE('',#8410,#8411,#4180,.T.);
#10936=EDGE_CURVE('',#8411,#8412,#771,.T.);
#10937=EDGE_CURVE('',#8412,#8413,#4181,.T.);
#10938=EDGE_CURVE('',#8413,#8414,#772,.T.);
#10939=EDGE_CURVE('',#8414,#8415,#4182,.T.);
#10940=EDGE_CURVE('',#8415,#8416,#773,.T.);
#10941=EDGE_CURVE('',#8416,#8417,#4183,.T.);
#10942=EDGE_CURVE('',#8417,#8418,#774,.T.);
#10943=EDGE_CURVE('',#8418,#8419,#4184,.T.);
#10944=EDGE_CURVE('',#8419,#8420,#775,.T.);
#10945=EDGE_CURVE('',#8420,#8421,#4185,.T.);
#10946=EDGE_CURVE('',#8421,#8422,#776,.T.);
#10947=EDGE_CURVE('',#8422,#8423,#4186,.T.);
#10948=EDGE_CURVE('',#8423,#8424,#777,.T.);
#10949=EDGE_CURVE('',#8424,#8425,#4187,.T.);
#10950=EDGE_CURVE('',#8425,#8426,#778,.T.);
#10951=EDGE_CURVE('',#8426,#8427,#4188,.T.);
#10952=EDGE_CURVE('',#8427,#8428,#779,.T.);
#10953=EDGE_CURVE('',#8428,#8429,#4189,.T.);
#10954=EDGE_CURVE('',#8429,#8430,#780,.T.);
#10955=EDGE_CURVE('',#8430,#8431,#4190,.T.);
#10956=EDGE_CURVE('',#8431,#8432,#781,.T.);
#10957=EDGE_CURVE('',#8432,#8433,#4191,.T.);
#10958=EDGE_CURVE('',#8433,#8434,#782,.T.);
#10959=EDGE_CURVE('',#8434,#8435,#4192,.T.);
#10960=EDGE_CURVE('',#8435,#8436,#783,.T.);
#10961=EDGE_CURVE('',#8436,#8437,#4193,.T.);
#10962=EDGE_CURVE('',#8437,#8438,#784,.T.);
#10963=EDGE_CURVE('',#8438,#8439,#4194,.T.);
#10964=EDGE_CURVE('',#8439,#8440,#785,.T.);
#10965=EDGE_CURVE('',#8440,#8441,#4195,.T.);
#10966=EDGE_CURVE('',#8441,#8442,#786,.T.);
#10967=EDGE_CURVE('',#8442,#8443,#4196,.T.);
#10968=EDGE_CURVE('',#8443,#8444,#787,.T.);
#10969=EDGE_CURVE('',#8444,#8445,#4197,.T.);
#10970=EDGE_CURVE('',#8445,#8446,#788,.T.);
#10971=EDGE_CURVE('',#8446,#8447,#4198,.T.);
#10972=EDGE_CURVE('',#8447,#8448,#789,.T.);
#10973=EDGE_CURVE('',#8448,#8449,#4199,.T.);
#10974=EDGE_CURVE('',#8449,#8450,#790,.T.);
#10975=EDGE_CURVE('',#8450,#8451,#4200,.T.);
#10976=EDGE_CURVE('',#8451,#8452,#791,.T.);
#10977=EDGE_CURVE('',#8452,#8453,#4201,.T.);
#10978=EDGE_CURVE('',#8453,#8454,#792,.T.);
#10979=EDGE_CURVE('',#8454,#8455,#4202,.T.);
#10980=EDGE_CURVE('',#8455,#8456,#793,.T.);
#10981=EDGE_CURVE('',#8456,#8457,#4203,.T.);
#10982=EDGE_CURVE('',#8457,#8458,#794,.T.);
#10983=EDGE_CURVE('',#8458,#8459,#4204,.T.);
#10984=EDGE_CURVE('',#8459,#8460,#795,.T.);
#10985=EDGE_CURVE('',#8460,#8461,#4205,.T.);
#10986=EDGE_CURVE('',#8461,#8462,#796,.T.);
#10987=EDGE_CURVE('',#8462,#8463,#4206,.T.);
#10988=EDGE_CURVE('',#8463,#8464,#797,.T.);
#10989=EDGE_CURVE('',#8464,#8465,#4207,.T.);
#10990=EDGE_CURVE('',#8465,#8466,#798,.T.);
#10991=EDGE_CURVE('',#8466,#8467,#4208,.T.);
#10992=EDGE_CURVE('',#8467,#8468,#799,.T.);
#10993=EDGE_CURVE('',#8468,#8469,#4209,.T.);
#10994=EDGE_CURVE('',#8469,#8470,#800,.T.);
#10995=EDGE_CURVE('',#8470,#8471,#4210,.T.);
#10996=EDGE_CURVE('',#8471,#8472,#801,.T.);
#10997=EDGE_CURVE('',#8472,#8473,#4211,.T.);
#10998=EDGE_CURVE('',#8473,#8474,#802,.T.);
#10999=EDGE_CURVE('',#8474,#8475,#4212,.T.);
#11000=EDGE_CURVE('',#8475,#8476,#803,.T.);
#11001=EDGE_CURVE('',#8476,#8377,#4213,.T.);
#11002=EDGE_CURVE('',#8376,#8368,#4214,.T.);
#11003=EDGE_CURVE('',#8477,#8371,#4215,.T.);
#11004=EDGE_CURVE('',#8478,#8477,#804,.T.);
#11005=EDGE_CURVE('',#8479,#8478,#4216,.T.);
#11006=EDGE_CURVE('',#8480,#8479,#805,.T.);
#11007=EDGE_CURVE('',#8481,#8480,#4217,.T.);
#11008=EDGE_CURVE('',#8482,#8481,#806,.T.);
#11009=EDGE_CURVE('',#8483,#8482,#4218,.T.);
#11010=EDGE_CURVE('',#8484,#8483,#807,.T.);
#11011=EDGE_CURVE('',#8485,#8484,#4219,.T.);
#11012=EDGE_CURVE('',#8486,#8485,#808,.T.);
#11013=EDGE_CURVE('',#8487,#8486,#4220,.T.);
#11014=EDGE_CURVE('',#8488,#8487,#809,.T.);
#11015=EDGE_CURVE('',#8489,#8488,#4221,.T.);
#11016=EDGE_CURVE('',#8490,#8489,#810,.T.);
#11017=EDGE_CURVE('',#8491,#8490,#4222,.T.);
#11018=EDGE_CURVE('',#8492,#8491,#811,.T.);
#11019=EDGE_CURVE('',#8493,#8492,#4223,.T.);
#11020=EDGE_CURVE('',#8494,#8493,#812,.T.);
#11021=EDGE_CURVE('',#8495,#8494,#4224,.T.);
#11022=EDGE_CURVE('',#8496,#8495,#813,.T.);
#11023=EDGE_CURVE('',#8497,#8496,#4225,.T.);
#11024=EDGE_CURVE('',#8498,#8497,#814,.T.);
#11025=EDGE_CURVE('',#8499,#8498,#4226,.T.);
#11026=EDGE_CURVE('',#8500,#8499,#815,.T.);
#11027=EDGE_CURVE('',#8501,#8500,#4227,.T.);
#11028=EDGE_CURVE('',#8502,#8501,#816,.T.);
#11029=EDGE_CURVE('',#8503,#8502,#4228,.T.);
#11030=EDGE_CURVE('',#8504,#8503,#817,.T.);
#11031=EDGE_CURVE('',#8505,#8504,#4229,.T.);
#11032=EDGE_CURVE('',#8506,#8505,#818,.T.);
#11033=EDGE_CURVE('',#8507,#8506,#4230,.T.);
#11034=EDGE_CURVE('',#8508,#8507,#819,.T.);
#11035=EDGE_CURVE('',#8509,#8508,#4231,.T.);
#11036=EDGE_CURVE('',#8510,#8509,#820,.T.);
#11037=EDGE_CURVE('',#8511,#8510,#4232,.T.);
#11038=EDGE_CURVE('',#8512,#8511,#821,.T.);
#11039=EDGE_CURVE('',#8513,#8512,#4233,.T.);
#11040=EDGE_CURVE('',#8514,#8513,#822,.T.);
#11041=EDGE_CURVE('',#8515,#8514,#4234,.T.);
#11042=EDGE_CURVE('',#8516,#8515,#823,.T.);
#11043=EDGE_CURVE('',#8517,#8516,#4235,.T.);
#11044=EDGE_CURVE('',#8518,#8517,#824,.T.);
#11045=EDGE_CURVE('',#8519,#8518,#4236,.T.);
#11046=EDGE_CURVE('',#8520,#8519,#825,.T.);
#11047=EDGE_CURVE('',#8521,#8520,#4237,.T.);
#11048=EDGE_CURVE('',#8522,#8521,#826,.T.);
#11049=EDGE_CURVE('',#8523,#8522,#4238,.T.);
#11050=EDGE_CURVE('',#8370,#8523,#827,.T.);
#11051=EDGE_CURVE('',#8524,#8372,#4239,.T.);
#11052=EDGE_CURVE('',#8524,#8477,#5152,.T.);
#11053=EDGE_CURVE('',#8257,#8524,#5153,.T.);
#11054=EDGE_CURVE('',#8478,#8256,#5933,.T.);
#11055=EDGE_CURVE('',#8479,#8255,#5934,.T.);
#11056=EDGE_CURVE('',#8525,#8254,#5154,.T.);
#11057=EDGE_CURVE('',#8480,#8525,#5155,.T.);
#11058=EDGE_CURVE('',#8375,#8367,#4240,.T.);
#11059=EDGE_CURVE('',#8484,#8526,#5156,.T.);
#11060=EDGE_CURVE('',#8483,#8251,#5935,.T.);
#11061=EDGE_CURVE('',#8526,#8250,#5157,.T.);
#11062=EDGE_CURVE('',#8482,#8252,#5936,.T.);
#11063=EDGE_CURVE('',#8527,#8481,#5158,.T.);
#11064=EDGE_CURVE('',#8253,#8527,#5159,.T.);
#11065=EDGE_CURVE('',#8528,#8526,#4241,.T.);
#11066=EDGE_CURVE('',#8528,#8485,#5160,.T.);
#11067=EDGE_CURVE('',#8249,#8528,#5161,.T.);
#11068=EDGE_CURVE('',#8486,#8248,#5937,.T.);
#11069=EDGE_CURVE('',#8487,#8247,#5938,.T.);
#11070=EDGE_CURVE('',#8529,#8246,#5162,.T.);
#11071=EDGE_CURVE('',#8488,#8529,#5163,.T.);
#11072=EDGE_CURVE('',#8527,#8525,#4242,.T.);
#11073=EDGE_CURVE('',#8492,#8530,#5164,.T.);
#11074=EDGE_CURVE('',#8491,#8243,#5939,.T.);
#11075=EDGE_CURVE('',#8530,#8242,#5165,.T.);
#11076=EDGE_CURVE('',#8490,#8244,#5940,.T.);
#11077=EDGE_CURVE('',#8531,#8489,#5166,.T.);
#11078=EDGE_CURVE('',#8245,#8531,#5167,.T.);
#11079=EDGE_CURVE('',#8532,#8530,#4243,.T.);
#11080=EDGE_CURVE('',#8532,#8493,#5168,.T.);
#11081=EDGE_CURVE('',#8241,#8532,#5169,.T.);
#11082=EDGE_CURVE('',#8494,#8240,#5941,.T.);
#11083=EDGE_CURVE('',#8495,#8239,#5942,.T.);
#11084=EDGE_CURVE('',#8533,#8238,#5170,.T.);
#11085=EDGE_CURVE('',#8496,#8533,#5171,.T.);
#11086=EDGE_CURVE('',#8531,#8529,#4244,.T.);
#11087=EDGE_CURVE('',#8500,#8534,#5172,.T.);
#11088=EDGE_CURVE('',#8499,#8235,#5943,.T.);
#11089=EDGE_CURVE('',#8534,#8234,#5173,.T.);
#11090=EDGE_CURVE('',#8498,#8236,#5944,.T.);
#11091=EDGE_CURVE('',#8535,#8497,#5174,.T.);
#11092=EDGE_CURVE('',#8237,#8535,#5175,.T.);
#11093=EDGE_CURVE('',#8536,#8534,#4245,.T.);
#11094=EDGE_CURVE('',#8536,#8501,#5176,.T.);
#11095=EDGE_CURVE('',#8233,#8536,#5177,.T.);
#11096=EDGE_CURVE('',#8502,#8232,#5945,.T.);
#11097=EDGE_CURVE('',#8503,#8231,#5946,.T.);
#11098=EDGE_CURVE('',#8537,#8230,#5178,.T.);
#11099=EDGE_CURVE('',#8504,#8537,#5179,.T.);
#11100=EDGE_CURVE('',#8535,#8533,#4246,.T.);
#11101=EDGE_CURVE('',#8508,#8538,#5180,.T.);
#11102=EDGE_CURVE('',#8507,#8227,#5947,.T.);
#11103=EDGE_CURVE('',#8538,#8226,#5181,.T.);
#11104=EDGE_CURVE('',#8506,#8228,#5948,.T.);
#11105=EDGE_CURVE('',#8539,#8505,#5182,.T.);
#11106=EDGE_CURVE('',#8229,#8539,#5183,.T.);
#11107=EDGE_CURVE('',#8540,#8538,#4247,.T.);
#11108=EDGE_CURVE('',#8540,#8509,#5184,.T.);
#11109=EDGE_CURVE('',#8225,#8540,#5185,.T.);
#11110=EDGE_CURVE('',#8510,#8224,#5949,.T.);
#11111=EDGE_CURVE('',#8511,#8223,#5950,.T.);
#11112=EDGE_CURVE('',#8541,#8222,#5186,.T.);
#11113=EDGE_CURVE('',#8512,#8541,#5187,.T.);
#11114=EDGE_CURVE('',#8539,#8537,#4248,.T.);
#11115=EDGE_CURVE('',#8516,#8542,#5188,.T.);
#11116=EDGE_CURVE('',#8515,#8219,#5951,.T.);
#11117=EDGE_CURVE('',#8542,#8218,#5189,.T.);
#11118=EDGE_CURVE('',#8514,#8220,#5952,.T.);
#11119=EDGE_CURVE('',#8543,#8513,#5190,.T.);
#11120=EDGE_CURVE('',#8221,#8543,#5191,.T.);
#11121=EDGE_CURVE('',#8544,#8542,#4249,.T.);
#11122=EDGE_CURVE('',#8544,#8517,#5192,.T.);
#11123=EDGE_CURVE('',#8217,#8544,#5193,.T.);
#11124=EDGE_CURVE('',#8518,#8216,#5953,.T.);
#11125=EDGE_CURVE('',#8519,#8215,#5954,.T.);
#11126=EDGE_CURVE('',#8545,#8214,#5194,.T.);
#11127=EDGE_CURVE('',#8520,#8545,#5195,.T.);
#11128=EDGE_CURVE('',#8543,#8541,#4250,.T.);
#11129=EDGE_CURVE('',#8213,#8546,#5196,.T.);
#11130=EDGE_CURVE('',#8522,#8212,#5955,.T.);
#11131=EDGE_CURVE('',#8546,#8521,#5197,.T.);
#11132=EDGE_CURVE('',#8523,#8211,#5956,.T.);
#11133=EDGE_CURVE('',#8266,#8547,#5198,.T.);
#11134=EDGE_CURVE('',#8265,#8476,#5957,.T.);
#11135=EDGE_CURVE('',#8548,#8475,#5199,.T.);
#11136=EDGE_CURVE('',#8547,#8548,#5200,.T.);
#11137=EDGE_CURVE('',#8264,#8377,#5958,.T.);
#11138=EDGE_CURVE('',#8549,#8263,#5201,.T.);
#11139=EDGE_CURVE('',#8550,#8549,#5202,.T.);
#11140=EDGE_CURVE('',#8378,#8550,#5203,.T.);
#11141=EDGE_CURVE('',#8551,#8547,#4251,.T.);
#11142=EDGE_CURVE('',#8551,#8267,#5204,.T.);
#11143=EDGE_CURVE('',#8552,#8548,#4252,.T.);
#11144=EDGE_CURVE('',#8552,#8551,#5205,.T.);
#11145=EDGE_CURVE('',#8474,#8552,#5206,.T.);
#11146=EDGE_CURVE('',#8270,#8553,#5207,.T.);
#11147=EDGE_CURVE('',#8269,#8472,#5959,.T.);
#11148=EDGE_CURVE('',#8554,#8471,#5208,.T.);
#11149=EDGE_CURVE('',#8553,#8554,#5209,.T.);
#11150=EDGE_CURVE('',#8268,#8473,#5960,.T.);
#11151=EDGE_CURVE('',#8555,#8553,#4253,.T.);
#11152=EDGE_CURVE('',#8555,#8271,#5210,.T.);
#11153=EDGE_CURVE('',#8556,#8554,#4254,.T.);
#11154=EDGE_CURVE('',#8556,#8555,#5211,.T.);
#11155=EDGE_CURVE('',#8470,#8556,#5212,.T.);
#11156=EDGE_CURVE('',#8274,#8557,#5213,.T.);
#11157=EDGE_CURVE('',#8273,#8468,#5961,.T.);
#11158=EDGE_CURVE('',#8558,#8467,#5214,.T.);
#11159=EDGE_CURVE('',#8557,#8558,#5215,.T.);
#11160=EDGE_CURVE('',#8272,#8469,#5962,.T.);
#11161=EDGE_CURVE('',#8559,#8557,#4255,.T.);
#11162=EDGE_CURVE('',#8559,#8275,#5216,.T.);
#11163=EDGE_CURVE('',#8560,#8558,#4256,.T.);
#11164=EDGE_CURVE('',#8560,#8559,#5217,.T.);
#11165=EDGE_CURVE('',#8466,#8560,#5218,.T.);
#11166=EDGE_CURVE('',#8278,#8561,#5219,.T.);
#11167=EDGE_CURVE('',#8277,#8464,#5963,.T.);
#11168=EDGE_CURVE('',#8562,#8463,#5220,.T.);
#11169=EDGE_CURVE('',#8561,#8562,#5221,.T.);
#11170=EDGE_CURVE('',#8276,#8465,#5964,.T.);
#11171=EDGE_CURVE('',#8563,#8561,#4257,.T.);
#11172=EDGE_CURVE('',#8563,#8279,#5222,.T.);
#11173=EDGE_CURVE('',#8564,#8562,#4258,.T.);
#11174=EDGE_CURVE('',#8564,#8563,#5223,.T.);
#11175=EDGE_CURVE('',#8462,#8564,#5224,.T.);
#11176=EDGE_CURVE('',#8282,#8565,#5225,.T.);
#11177=EDGE_CURVE('',#8281,#8460,#5965,.T.);
#11178=EDGE_CURVE('',#8566,#8459,#5226,.T.);
#11179=EDGE_CURVE('',#8565,#8566,#5227,.T.);
#11180=EDGE_CURVE('',#8280,#8461,#5966,.T.);
#11181=EDGE_CURVE('',#8567,#8565,#4259,.T.);
#11182=EDGE_CURVE('',#8567,#8283,#5228,.T.);
#11183=EDGE_CURVE('',#8568,#8566,#4260,.T.);
#11184=EDGE_CURVE('',#8568,#8567,#5229,.T.);
#11185=EDGE_CURVE('',#8458,#8568,#5230,.T.);
#11186=EDGE_CURVE('',#8286,#8569,#5231,.T.);
#11187=EDGE_CURVE('',#8285,#8456,#5967,.T.);
#11188=EDGE_CURVE('',#8570,#8455,#5232,.T.);
#11189=EDGE_CURVE('',#8569,#8570,#5233,.T.);
#11190=EDGE_CURVE('',#8284,#8457,#5968,.T.);
#11191=EDGE_CURVE('',#8571,#8569,#4261,.T.);
#11192=EDGE_CURVE('',#8571,#8287,#5234,.T.);
#11193=EDGE_CURVE('',#8572,#8570,#4262,.T.);
#11194=EDGE_CURVE('',#8572,#8571,#5235,.T.);
#11195=EDGE_CURVE('',#8454,#8572,#5236,.T.);
#11196=EDGE_CURVE('',#8290,#8573,#5237,.T.);
#11197=EDGE_CURVE('',#8289,#8452,#5969,.T.);
#11198=EDGE_CURVE('',#8574,#8451,#5238,.T.);
#11199=EDGE_CURVE('',#8573,#8574,#5239,.T.);
#11200=EDGE_CURVE('',#8288,#8453,#5970,.T.);
#11201=EDGE_CURVE('',#8575,#8573,#4263,.T.);
#11202=EDGE_CURVE('',#8575,#8291,#5240,.T.);
#11203=EDGE_CURVE('',#8576,#8574,#4264,.T.);
#11204=EDGE_CURVE('',#8576,#8575,#5241,.T.);
#11205=EDGE_CURVE('',#8450,#8576,#5242,.T.);
#11206=EDGE_CURVE('',#8294,#8577,#5243,.T.);
#11207=EDGE_CURVE('',#8293,#8448,#5971,.T.);
#11208=EDGE_CURVE('',#8578,#8447,#5244,.T.);
#11209=EDGE_CURVE('',#8577,#8578,#5245,.T.);
#11210=EDGE_CURVE('',#8292,#8449,#5972,.T.);
#11211=EDGE_CURVE('',#8579,#8577,#4265,.T.);
#11212=EDGE_CURVE('',#8579,#8295,#5246,.T.);
#11213=EDGE_CURVE('',#8580,#8578,#4266,.T.);
#11214=EDGE_CURVE('',#8580,#8579,#5247,.T.);
#11215=EDGE_CURVE('',#8446,#8580,#5248,.T.);
#11216=EDGE_CURVE('',#8298,#8581,#5249,.T.);
#11217=EDGE_CURVE('',#8297,#8444,#5973,.T.);
#11218=EDGE_CURVE('',#8582,#8443,#5250,.T.);
#11219=EDGE_CURVE('',#8581,#8582,#5251,.T.);
#11220=EDGE_CURVE('',#8296,#8445,#5974,.T.);
#11221=EDGE_CURVE('',#8583,#8581,#4267,.T.);
#11222=EDGE_CURVE('',#8583,#8299,#5252,.T.);
#11223=EDGE_CURVE('',#8584,#8582,#4268,.T.);
#11224=EDGE_CURVE('',#8584,#8583,#5253,.T.);
#11225=EDGE_CURVE('',#8442,#8584,#5254,.T.);
#11226=EDGE_CURVE('',#8302,#8585,#5255,.T.);
#11227=EDGE_CURVE('',#8301,#8440,#5975,.T.);
#11228=EDGE_CURVE('',#8586,#8439,#5256,.T.);
#11229=EDGE_CURVE('',#8585,#8586,#5257,.T.);
#11230=EDGE_CURVE('',#8300,#8441,#5976,.T.);
#11231=EDGE_CURVE('',#8587,#8585,#4269,.T.);
#11232=EDGE_CURVE('',#8587,#8303,#5258,.T.);
#11233=EDGE_CURVE('',#8588,#8586,#4270,.T.);
#11234=EDGE_CURVE('',#8588,#8587,#5259,.T.);
#11235=EDGE_CURVE('',#8438,#8588,#5260,.T.);
#11236=EDGE_CURVE('',#8306,#8589,#5261,.T.);
#11237=EDGE_CURVE('',#8305,#8436,#5977,.T.);
#11238=EDGE_CURVE('',#8590,#8435,#5262,.T.);
#11239=EDGE_CURVE('',#8589,#8590,#5263,.T.);
#11240=EDGE_CURVE('',#8304,#8437,#5978,.T.);
#11241=EDGE_CURVE('',#8591,#8589,#4271,.T.);
#11242=EDGE_CURVE('',#8591,#8307,#5264,.T.);
#11243=EDGE_CURVE('',#8592,#8590,#4272,.T.);
#11244=EDGE_CURVE('',#8592,#8591,#5265,.T.);
#11245=EDGE_CURVE('',#8434,#8592,#5266,.T.);
#11246=EDGE_CURVE('',#8310,#8593,#5267,.T.);
#11247=EDGE_CURVE('',#8309,#8432,#5979,.T.);
#11248=EDGE_CURVE('',#8594,#8431,#5268,.T.);
#11249=EDGE_CURVE('',#8593,#8594,#5269,.T.);
#11250=EDGE_CURVE('',#8308,#8433,#5980,.T.);
#11251=EDGE_CURVE('',#8595,#8593,#4273,.T.);
#11252=EDGE_CURVE('',#8595,#8311,#5270,.T.);
#11253=EDGE_CURVE('',#8596,#8594,#4274,.T.);
#11254=EDGE_CURVE('',#8596,#8595,#5271,.T.);
#11255=EDGE_CURVE('',#8430,#8596,#5272,.T.);
#11256=EDGE_CURVE('',#8314,#8597,#5273,.T.);
#11257=EDGE_CURVE('',#8313,#8428,#5981,.T.);
#11258=EDGE_CURVE('',#8598,#8427,#5274,.T.);
#11259=EDGE_CURVE('',#8597,#8598,#5275,.T.);
#11260=EDGE_CURVE('',#8312,#8429,#5982,.T.);
#11261=EDGE_CURVE('',#8599,#8597,#4275,.T.);
#11262=EDGE_CURVE('',#8599,#8315,#5276,.T.);
#11263=EDGE_CURVE('',#8600,#8598,#4276,.T.);
#11264=EDGE_CURVE('',#8600,#8599,#5277,.T.);
#11265=EDGE_CURVE('',#8426,#8600,#5278,.T.);
#11266=EDGE_CURVE('',#8318,#8601,#5279,.T.);
#11267=EDGE_CURVE('',#8317,#8424,#5983,.T.);
#11268=EDGE_CURVE('',#8602,#8423,#5280,.T.);
#11269=EDGE_CURVE('',#8601,#8602,#5281,.T.);
#11270=EDGE_CURVE('',#8316,#8425,#5984,.T.);
#11271=EDGE_CURVE('',#8603,#8601,#4277,.T.);
#11272=EDGE_CURVE('',#8603,#8319,#5282,.T.);
#11273=EDGE_CURVE('',#8604,#8602,#4278,.T.);
#11274=EDGE_CURVE('',#8604,#8603,#5283,.T.);
#11275=EDGE_CURVE('',#8422,#8604,#5284,.T.);
#11276=EDGE_CURVE('',#8322,#8605,#5285,.T.);
#11277=EDGE_CURVE('',#8321,#8420,#5985,.T.);
#11278=EDGE_CURVE('',#8606,#8419,#5286,.T.);
#11279=EDGE_CURVE('',#8605,#8606,#5287,.T.);
#11280=EDGE_CURVE('',#8320,#8421,#5986,.T.);
#11281=EDGE_CURVE('',#8607,#8605,#4279,.T.);
#11282=EDGE_CURVE('',#8607,#8323,#5288,.T.);
#11283=EDGE_CURVE('',#8608,#8606,#4280,.T.);
#11284=EDGE_CURVE('',#8608,#8607,#5289,.T.);
#11285=EDGE_CURVE('',#8418,#8608,#5290,.T.);
#11286=EDGE_CURVE('',#8326,#8609,#5291,.T.);
#11287=EDGE_CURVE('',#8325,#8416,#5987,.T.);
#11288=EDGE_CURVE('',#8610,#8415,#5292,.T.);
#11289=EDGE_CURVE('',#8609,#8610,#5293,.T.);
#11290=EDGE_CURVE('',#8324,#8417,#5988,.T.);
#11291=EDGE_CURVE('',#8611,#8609,#4281,.T.);
#11292=EDGE_CURVE('',#8611,#8327,#5294,.T.);
#11293=EDGE_CURVE('',#8612,#8610,#4282,.T.);
#11294=EDGE_CURVE('',#8612,#8611,#5295,.T.);
#11295=EDGE_CURVE('',#8414,#8612,#5296,.T.);
#11296=EDGE_CURVE('',#8330,#8613,#5297,.T.);
#11297=EDGE_CURVE('',#8329,#8412,#5989,.T.);
#11298=EDGE_CURVE('',#8614,#8411,#5298,.T.);
#11299=EDGE_CURVE('',#8613,#8614,#5299,.T.);
#11300=EDGE_CURVE('',#8328,#8413,#5990,.T.);
#11301=EDGE_CURVE('',#8615,#8613,#4283,.T.);
#11302=EDGE_CURVE('',#8615,#8331,#5300,.T.);
#11303=EDGE_CURVE('',#8616,#8614,#4284,.T.);
#11304=EDGE_CURVE('',#8616,#8615,#5301,.T.);
#11305=EDGE_CURVE('',#8410,#8616,#5302,.T.);
#11306=EDGE_CURVE('',#8334,#8617,#5303,.T.);
#11307=EDGE_CURVE('',#8333,#8408,#5991,.T.);
#11308=EDGE_CURVE('',#8618,#8407,#5304,.T.);
#11309=EDGE_CURVE('',#8617,#8618,#5305,.T.);
#11310=EDGE_CURVE('',#8332,#8409,#5992,.T.);
#11311=EDGE_CURVE('',#8619,#8617,#4285,.T.);
#11312=EDGE_CURVE('',#8619,#8335,#5306,.T.);
#11313=EDGE_CURVE('',#8620,#8618,#4286,.T.);
#11314=EDGE_CURVE('',#8620,#8619,#5307,.T.);
#11315=EDGE_CURVE('',#8406,#8620,#5308,.T.);
#11316=EDGE_CURVE('',#8338,#8621,#5309,.T.);
#11317=EDGE_CURVE('',#8337,#8404,#5993,.T.);
#11318=EDGE_CURVE('',#8622,#8403,#5310,.T.);
#11319=EDGE_CURVE('',#8621,#8622,#5311,.T.);
#11320=EDGE_CURVE('',#8336,#8405,#5994,.T.);
#11321=EDGE_CURVE('',#8623,#8621,#4287,.T.);
#11322=EDGE_CURVE('',#8623,#8339,#5312,.T.);
#11323=EDGE_CURVE('',#8624,#8622,#4288,.T.);
#11324=EDGE_CURVE('',#8624,#8623,#5313,.T.);
#11325=EDGE_CURVE('',#8402,#8624,#5314,.T.);
#11326=EDGE_CURVE('',#8342,#8625,#5315,.T.);
#11327=EDGE_CURVE('',#8341,#8400,#5995,.T.);
#11328=EDGE_CURVE('',#8626,#8399,#5316,.T.);
#11329=EDGE_CURVE('',#8625,#8626,#5317,.T.);
#11330=EDGE_CURVE('',#8340,#8401,#5996,.T.);
#11331=EDGE_CURVE('',#8627,#8625,#4289,.T.);
#11332=EDGE_CURVE('',#8627,#8343,#5318,.T.);
#11333=EDGE_CURVE('',#8628,#8626,#4290,.T.);
#11334=EDGE_CURVE('',#8628,#8627,#5319,.T.);
#11335=EDGE_CURVE('',#8398,#8628,#5320,.T.);
#11336=EDGE_CURVE('',#8346,#8629,#5321,.T.);
#11337=EDGE_CURVE('',#8345,#8396,#5997,.T.);
#11338=EDGE_CURVE('',#8630,#8395,#5322,.T.);
#11339=EDGE_CURVE('',#8629,#8630,#5323,.T.);
#11340=EDGE_CURVE('',#8344,#8397,#5998,.T.);
#11341=EDGE_CURVE('',#8631,#8629,#4291,.T.);
#11342=EDGE_CURVE('',#8631,#8347,#5324,.T.);
#11343=EDGE_CURVE('',#8632,#8630,#4292,.T.);
#11344=EDGE_CURVE('',#8632,#8631,#5325,.T.);
#11345=EDGE_CURVE('',#8394,#8632,#5326,.T.);
#11346=EDGE_CURVE('',#8350,#8633,#5327,.T.);
#11347=EDGE_CURVE('',#8349,#8392,#5999,.T.);
#11348=EDGE_CURVE('',#8634,#8391,#5328,.T.);
#11349=EDGE_CURVE('',#8633,#8634,#5329,.T.);
#11350=EDGE_CURVE('',#8348,#8393,#6000,.T.);
#11351=EDGE_CURVE('',#8635,#8633,#4293,.T.);
#11352=EDGE_CURVE('',#8635,#8351,#5330,.T.);
#11353=EDGE_CURVE('',#8636,#8634,#4294,.T.);
#11354=EDGE_CURVE('',#8636,#8635,#5331,.T.);
#11355=EDGE_CURVE('',#8390,#8636,#5332,.T.);
#11356=EDGE_CURVE('',#8354,#8637,#5333,.T.);
#11357=EDGE_CURVE('',#8353,#8388,#6001,.T.);
#11358=EDGE_CURVE('',#8638,#8387,#5334,.T.);
#11359=EDGE_CURVE('',#8637,#8638,#5335,.T.);
#11360=EDGE_CURVE('',#8352,#8389,#6002,.T.);
#11361=EDGE_CURVE('',#8639,#8637,#4295,.T.);
#11362=EDGE_CURVE('',#8639,#8355,#5336,.T.);
#11363=EDGE_CURVE('',#8640,#8638,#4296,.T.);
#11364=EDGE_CURVE('',#8640,#8639,#5337,.T.);
#11365=EDGE_CURVE('',#8386,#8640,#5338,.T.);
#11366=EDGE_CURVE('',#8358,#8641,#5339,.T.);
#11367=EDGE_CURVE('',#8357,#8384,#6003,.T.);
#11368=EDGE_CURVE('',#8642,#8383,#5340,.T.);
#11369=EDGE_CURVE('',#8641,#8642,#5341,.T.);
#11370=EDGE_CURVE('',#8356,#8385,#6004,.T.);
#11371=EDGE_CURVE('',#8643,#8641,#4297,.T.);
#11372=EDGE_CURVE('',#8643,#8359,#5342,.T.);
#11373=EDGE_CURVE('',#8644,#8642,#4298,.T.);
#11374=EDGE_CURVE('',#8644,#8643,#5343,.T.);
#11375=EDGE_CURVE('',#8382,#8644,#5344,.T.);
#11376=EDGE_CURVE('',#8362,#8645,#5345,.T.);
#11377=EDGE_CURVE('',#8361,#8380,#6005,.T.);
#11378=EDGE_CURVE('',#8646,#8379,#5346,.T.);
#11379=EDGE_CURVE('',#8645,#8646,#5347,.T.);
#11380=EDGE_CURVE('',#8360,#8381,#6006,.T.);
#11381=EDGE_CURVE('',#8549,#8645,#4299,.T.);
#11382=EDGE_CURVE('',#8550,#8646,#4300,.T.);
#11383=EDGE_CURVE('',#8546,#8545,#4301,.T.);
#11384=EDGE_CURVE('',#8647,#8647,#4302,.T.);
#11385=EDGE_CURVE('',#8647,#8648,#4303,.T.);
#11386=EDGE_CURVE('',#8648,#8649,#4304,.T.);
#11387=EDGE_CURVE('',#8649,#8648,#4305,.T.);
#11388=EDGE_CURVE('',#8649,#8650,#6007,.T.);
#11389=EDGE_CURVE('',#8651,#8650,#4306,.T.);
#11390=EDGE_CURVE('',#8650,#8651,#4307,.T.);
#11391=EDGE_CURVE('',#8651,#8652,#4308,.T.);
#11392=EDGE_CURVE('',#8652,#8653,#4309,.T.);
#11393=EDGE_CURVE('',#8653,#8652,#4310,.T.);
#11394=EDGE_CURVE('',#8653,#8654,#6008,.T.);
#11395=EDGE_CURVE('',#8655,#8654,#4311,.T.);
#11396=EDGE_CURVE('',#8654,#8655,#4312,.T.);
#11397=EDGE_CURVE('',#8655,#8656,#4313,.T.);
#11398=EDGE_CURVE('',#8656,#8657,#4314,.T.);
#11399=EDGE_CURVE('',#8657,#8656,#4315,.T.);
#11400=EDGE_CURVE('',#8657,#8658,#6009,.T.);
#11401=EDGE_CURVE('',#8659,#8658,#4316,.T.);
#11402=EDGE_CURVE('',#8658,#8659,#4317,.T.);
#11403=EDGE_CURVE('',#8659,#8660,#4318,.T.);
#11404=EDGE_CURVE('',#8660,#8660,#4319,.T.);
#11405=EDGE_CURVE('',#8661,#8662,#4320,.T.);
#11406=EDGE_CURVE('',#8662,#8663,#6010,.T.);
#11407=EDGE_CURVE('',#8663,#8664,#4321,.T.);
#11408=EDGE_CURVE('',#8664,#8661,#6011,.T.);
#11409=EDGE_CURVE('',#8665,#8666,#4322,.T.);
#11410=EDGE_CURVE('',#8666,#8664,#4323,.T.);
#11411=EDGE_CURVE('',#8663,#8665,#4324,.T.);
#11412=EDGE_CURVE('',#8667,#8668,#4325,.T.);
#11413=EDGE_CURVE('',#8668,#8666,#6012,.T.);
#11414=EDGE_CURVE('',#8665,#8667,#6013,.T.);
#11415=EDGE_CURVE('',#8661,#8668,#4326,.T.);
#11416=EDGE_CURVE('',#8667,#8662,#4327,.T.);
#11417=EDGE_CURVE('',#8669,#8663,#6014,.T.);
#11418=EDGE_CURVE('',#8670,#8669,#4328,.T.);
#11419=EDGE_CURVE('',#8670,#8665,#6015,.T.);
#11420=EDGE_CURVE('',#8671,#8662,#6016,.T.);
#11421=EDGE_CURVE('',#8669,#8671,#6017,.T.);
#11422=EDGE_CURVE('',#8672,#8672,#4329,.T.);
#11423=EDGE_CURVE('',#8673,#8669,#4330,.T.);
#11424=EDGE_CURVE('',#8671,#8674,#4331,.T.);
#11425=EDGE_CURVE('',#8674,#8673,#6018,.T.);
#11426=EDGE_CURVE('',#8675,#8676,#4332,.T.);
#11427=EDGE_CURVE('',#8676,#8674,#4333,.T.);
#11428=EDGE_CURVE('',#8671,#8675,#4334,.T.);
#11429=EDGE_CURVE('',#8670,#8677,#4335,.T.);
#11430=EDGE_CURVE('',#8677,#8676,#6019,.T.);
#11431=EDGE_CURVE('',#8675,#8670,#6020,.T.);
#11432=EDGE_CURVE('',#8673,#8677,#4336,.T.);
#11433=EDGE_CURVE('',#8675,#8667,#6021,.T.);
#11434=EDGE_CURVE('',#8678,#8678,#4337,.T.);
#11435=EDGE_CURVE('',#8678,#8679,#4338,.T.);
#11436=EDGE_CURVE('',#8679,#8679,#4339,.T.);
#11437=EDGE_CURVE('',#8679,#8680,#6022,.T.);
#11438=EDGE_CURVE('',#8681,#8680,#4340,.T.);
#11439=EDGE_CURVE('',#8680,#8681,#4341,.T.);
#11440=EDGE_CURVE('',#8672,#8681,#4342,.T.);
#11441=EDGE_CURVE('',#8682,#8682,#4343,.T.);
#11442=EDGE_CURVE('',#8682,#8683,#4344,.T.);
#11443=EDGE_CURVE('',#8683,#8684,#4345,.T.);
#11444=EDGE_CURVE('',#8684,#8683,#4346,.T.);
#11445=EDGE_CURVE('',#8684,#8685,#6023,.T.);
#11446=EDGE_CURVE('',#8686,#8685,#4347,.T.);
#11447=EDGE_CURVE('',#8685,#8686,#4348,.T.);
#11448=EDGE_CURVE('',#8686,#8687,#4349,.T.);
#11449=EDGE_CURVE('',#8687,#8688,#4350,.T.);
#11450=EDGE_CURVE('',#8688,#8687,#4351,.T.);
#11451=EDGE_CURVE('',#8688,#8689,#6024,.T.);
#11452=EDGE_CURVE('',#8690,#8689,#4352,.T.);
#11453=EDGE_CURVE('',#8689,#8690,#4353,.T.);
#11454=EDGE_CURVE('',#8690,#8691,#4354,.T.);
#11455=EDGE_CURVE('',#8691,#8692,#4355,.T.);
#11456=EDGE_CURVE('',#8692,#8691,#4356,.T.);
#11457=EDGE_CURVE('',#8692,#8693,#6025,.T.);
#11458=EDGE_CURVE('',#8694,#8693,#4357,.T.);
#11459=EDGE_CURVE('',#8693,#8694,#4358,.T.);
#11460=EDGE_CURVE('',#8694,#8695,#4359,.T.);
#11461=EDGE_CURVE('',#8695,#8695,#4360,.T.);
#11462=EDGE_CURVE('',#8696,#8696,#4361,.T.);
#11463=EDGE_CURVE('',#8696,#8697,#4362,.T.);
#11464=EDGE_CURVE('',#8697,#8697,#4363,.T.);
#11465=EDGE_CURVE('',#8698,#8699,#5348,.T.);
#11466=EDGE_CURVE('',#8698,#8700,#6026,.T.);
#11467=EDGE_CURVE('',#8700,#8701,#4364,.T.);
#11468=EDGE_CURVE('',#8701,#8702,#6027,.T.);
#11469=EDGE_CURVE('',#8702,#8703,#233,.T.);
#11470=EDGE_CURVE('',#8699,#8703,#6028,.T.);
#11471=EDGE_CURVE('',#8704,#8705,#6029,.T.);
#11472=EDGE_CURVE('',#8705,#8700,#4365,.T.);
#11473=EDGE_CURVE('',#8700,#8706,#6030,.T.);
#11474=EDGE_CURVE('',#8706,#8704,#234,.T.);
#11475=EDGE_CURVE('',#8707,#8708,#4366,.F.);
#11476=EDGE_CURVE('',#8709,#8707,#4367,.F.);
#11477=EDGE_CURVE('',#8708,#8709,#4368,.F.);
#11478=EDGE_CURVE('',#8706,#8709,#6031,.T.);
#11479=EDGE_CURVE('',#8707,#8704,#6032,.T.);
#11480=EDGE_CURVE('',#8710,#8711,#4369,.T.);
#11481=EDGE_CURVE('',#8711,#8708,#6033,.T.);
#11482=EDGE_CURVE('',#8709,#8710,#6034,.T.);
#11483=EDGE_CURVE('',#8710,#8712,#4370,.T.);
#11484=EDGE_CURVE('',#8712,#8711,#4371,.T.);
#11485=EDGE_CURVE('',#8713,#8714,#4372,.T.);
#11486=EDGE_CURVE('',#8714,#8715,#4373,.T.);
#11487=EDGE_CURVE('',#8715,#8713,#4374,.T.);
#11488=EDGE_CURVE('',#8713,#8707,#6035,.T.);
#11489=EDGE_CURVE('',#8708,#8714,#6036,.T.);
#11490=EDGE_CURVE('',#8705,#8701,#4375,.T.);
#11491=EDGE_CURVE('',#8702,#8716,#6037,.T.);
#11492=EDGE_CURVE('',#8716,#8717,#4376,.F.);
#11493=EDGE_CURVE('',#8717,#8718,#6038,.T.);
#11494=EDGE_CURVE('',#8718,#8703,#4377,.F.);
#11495=EDGE_CURVE('',#8715,#8701,#6039,.T.);
#11496=EDGE_CURVE('',#8716,#8715,#6040,.T.);
#11497=EDGE_CURVE('',#8705,#8713,#6041,.T.);
#11498=EDGE_CURVE('',#8710,#8719,#6042,.T.);
#11499=EDGE_CURVE('',#8719,#8720,#4378,.F.);
#11500=EDGE_CURVE('',#8720,#8712,#6043,.T.);
#11501=EDGE_CURVE('',#8717,#8721,#4379,.F.);
#11502=EDGE_CURVE('',#8721,#8716,#4380,.F.);
#11503=EDGE_CURVE('',#8714,#8721,#6044,.T.);
#11504=EDGE_CURVE('',#8712,#8717,#6045,.T.);
#11505=EDGE_CURVE('',#8721,#8711,#6046,.T.);
#11506=EDGE_CURVE('',#8698,#8722,#4381,.T.);
#11507=EDGE_CURVE('',#8722,#8706,#6047,.F.);
#11508=EDGE_CURVE('',#8723,#8724,#5349,.T.);
#11509=EDGE_CURVE('',#8723,#8725,#6048,.T.);
#11510=EDGE_CURVE('',#8725,#8726,#4382,.T.);
#11511=EDGE_CURVE('',#8726,#8727,#6049,.T.);
#11512=EDGE_CURVE('',#8727,#8728,#235,.T.);
#11513=EDGE_CURVE('',#8724,#8728,#6050,.T.);
#11514=EDGE_CURVE('',#8729,#8730,#4383,.T.);
#11515=EDGE_CURVE('',#8730,#8731,#6051,.T.);
#11516=EDGE_CURVE('',#8731,#8732,#4384,.T.);
#11517=EDGE_CURVE('',#8732,#8729,#6052,.T.);
#11518=EDGE_CURVE('',#8731,#8733,#4385,.T.);
#11519=EDGE_CURVE('',#8733,#8732,#4386,.T.);
#11520=EDGE_CURVE('',#8734,#8735,#6053,.T.);
#11521=EDGE_CURVE('',#8735,#8725,#4387,.T.);
#11522=EDGE_CURVE('',#8725,#8736,#6054,.T.);
#11523=EDGE_CURVE('',#8736,#8734,#236,.T.);
#11524=EDGE_CURVE('',#8736,#8737,#6055,.T.);
#11525=EDGE_CURVE('',#8737,#8729,#4388,.T.);
#11526=EDGE_CURVE('',#8729,#8734,#6056,.T.);
#11527=EDGE_CURVE('',#8737,#8730,#4389,.T.);
#11528=EDGE_CURVE('',#8735,#8726,#4390,.T.);
#11529=EDGE_CURVE('',#8727,#8738,#6057,.T.);
#11530=EDGE_CURVE('',#8738,#8739,#4391,.F.);
#11531=EDGE_CURVE('',#8739,#8740,#6058,.T.);
#11532=EDGE_CURVE('',#8740,#8728,#4392,.F.);
#11533=EDGE_CURVE('',#8733,#8726,#6059,.T.);
#11534=EDGE_CURVE('',#8738,#8733,#6060,.T.);
#11535=EDGE_CURVE('',#8735,#8732,#6061,.T.);
#11536=EDGE_CURVE('',#8741,#8742,#4393,.F.);
#11537=EDGE_CURVE('',#8743,#8741,#4394,.F.);
#11538=EDGE_CURVE('',#8742,#8743,#4395,.F.);
#11539=EDGE_CURVE('',#8744,#8745,#4396,.F.);
#11540=EDGE_CURVE('',#8745,#8743,#6062,.T.);
#11541=EDGE_CURVE('',#8741,#8744,#6063,.T.);
#11542=EDGE_CURVE('',#8739,#8746,#4397,.F.);
#11543=EDGE_CURVE('',#8746,#8738,#4398,.F.);
#11544=EDGE_CURVE('',#8731,#8746,#6064,.T.);
#11545=EDGE_CURVE('',#8746,#8742,#6065,.T.);
#11546=EDGE_CURVE('',#8743,#8739,#6066,.T.);
#11547=EDGE_CURVE('',#8737,#8741,#6067,.T.);
#11548=EDGE_CURVE('',#8742,#8730,#6068,.T.);
#11549=EDGE_CURVE('',#8723,#8747,#4399,.T.);
#11550=EDGE_CURVE('',#8747,#8748,#4400,.T.);
#11551=EDGE_CURVE('',#8748,#8736,#6069,.F.);
#11552=EDGE_CURVE('',#8749,#8750,#4401,.T.);
#11553=EDGE_CURVE('',#8750,#8751,#6070,.T.);
#11554=EDGE_CURVE('',#8751,#8752,#4402,.T.);
#11555=EDGE_CURVE('',#8752,#8749,#6071,.T.);
#11556=EDGE_CURVE('',#8751,#8753,#4403,.T.);
#11557=EDGE_CURVE('',#8753,#8752,#4404,.T.);
#11558=EDGE_CURVE('',#8749,#8754,#4405,.T.);
#11559=EDGE_CURVE('',#8754,#8750,#4406,.T.);
#11560=EDGE_CURVE('',#8754,#8755,#6072,.T.);
#11561=EDGE_CURVE('',#8756,#8755,#4407,.T.);
#11562=EDGE_CURVE('',#8756,#8750,#6073,.T.);
#11563=EDGE_CURVE('',#8749,#8757,#6074,.T.);
#11564=EDGE_CURVE('',#8757,#8758,#4408,.T.);
#11565=EDGE_CURVE('',#8758,#8754,#6075,.T.);
#11566=EDGE_CURVE('',#8759,#8752,#6076,.T.);
#11567=EDGE_CURVE('',#8757,#8759,#6077,.T.);
#11568=EDGE_CURVE('',#8760,#8761,#5350,.T.);
#11569=EDGE_CURVE('',#8760,#8762,#6078,.T.);
#11570=EDGE_CURVE('',#8762,#8755,#4409,.T.);
#11571=EDGE_CURVE('',#8755,#8763,#6079,.T.);
#11572=EDGE_CURVE('',#8763,#8764,#237,.T.);
#11573=EDGE_CURVE('',#8761,#8764,#6080,.T.);
#11574=EDGE_CURVE('',#8756,#8762,#4410,.T.);
#11575=EDGE_CURVE('',#8762,#8765,#6081,.T.);
#11576=EDGE_CURVE('',#8765,#8766,#4411,.T.);
#11577=EDGE_CURVE('',#8766,#8756,#6082,.T.);
#11578=EDGE_CURVE('',#8767,#8768,#238,.T.);
#11579=EDGE_CURVE('',#8768,#8769,#6083,.T.);
#11580=EDGE_CURVE('',#8769,#8765,#4412,.T.);
#11581=EDGE_CURVE('',#8765,#8770,#6084,.T.);
#11582=EDGE_CURVE('',#8770,#8771,#5351,.F.);
#11583=EDGE_CURVE('',#8771,#8767,#6085,.F.);
#11584=EDGE_CURVE('',#8769,#8766,#4413,.T.);
#11585=EDGE_CURVE('',#8763,#8758,#6086,.T.);
#11586=EDGE_CURVE('',#8772,#8758,#4414,.T.);
#11587=EDGE_CURVE('',#8772,#8773,#6087,.T.);
#11588=EDGE_CURVE('',#8773,#8764,#4415,.F.);
#11589=EDGE_CURVE('',#8751,#8766,#6088,.T.);
#11590=EDGE_CURVE('',#8769,#8753,#6089,.T.);
#11591=EDGE_CURVE('',#8774,#8768,#6090,.T.);
#11592=EDGE_CURVE('',#8753,#8774,#6091,.T.);
#11593=EDGE_CURVE('',#8767,#8775,#4416,.F.);
#11594=EDGE_CURVE('',#8775,#8776,#6092,.T.);
#11595=EDGE_CURVE('',#8776,#8774,#4417,.F.);
#11596=EDGE_CURVE('',#8748,#8777,#5352,.T.);
#11597=EDGE_CURVE('',#8747,#8778,#4418,.T.);
#11598=EDGE_CURVE('',#8778,#8779,#4419,.T.);
#11599=EDGE_CURVE('',#8779,#8778,#4420,.T.);
#11600=EDGE_CURVE('',#8771,#8724,#4421,.T.);
#11601=EDGE_CURVE('',#8770,#8760,#4422,.F.);
#11602=EDGE_CURVE('',#8780,#8761,#4423,.T.);
#11603=EDGE_CURVE('',#8780,#8781,#5353,.F.);
#11604=EDGE_CURVE('',#8781,#8782,#4424,.F.);
#11605=EDGE_CURVE('',#8783,#8782,#5354,.T.);
#11606=EDGE_CURVE('',#8783,#8784,#4425,.T.);
#11607=EDGE_CURVE('',#8722,#8784,#5355,.T.);
#11608=EDGE_CURVE('',#8777,#8699,#4426,.T.);
#11609=EDGE_CURVE('',#8783,#8785,#6093,.T.);
#11610=EDGE_CURVE('',#8786,#8785,#4427,.F.);
#11611=EDGE_CURVE('',#8786,#8787,#6094,.T.);
#11612=EDGE_CURVE('',#8788,#8787,#4428,.F.);
#11613=EDGE_CURVE('',#8780,#8788,#6095,.F.);
#11614=EDGE_CURVE('',#8773,#8775,#6096,.T.);
#11615=EDGE_CURVE('',#8740,#8745,#6097,.T.);
#11616=EDGE_CURVE('',#8744,#8777,#6098,.T.);
#11617=EDGE_CURVE('',#8718,#8720,#6099,.T.);
#11618=EDGE_CURVE('',#8719,#8784,#6100,.T.);
#11619=EDGE_CURVE('',#8789,#8789,#4429,.T.);
#11620=EDGE_CURVE('',#8779,#8790,#6101,.T.);
#11621=EDGE_CURVE('',#8791,#8790,#4430,.T.);
#11622=EDGE_CURVE('',#8790,#8791,#4431,.T.);
#11623=EDGE_CURVE('',#8792,#8792,#4432,.T.);
#11624=EDGE_CURVE('',#8792,#8793,#4433,.T.);
#11625=EDGE_CURVE('',#8793,#8794,#4434,.T.);
#11626=EDGE_CURVE('',#8794,#8793,#4435,.T.);
#11627=EDGE_CURVE('',#8794,#8795,#6102,.T.);
#11628=EDGE_CURVE('',#8796,#8795,#4436,.T.);
#11629=EDGE_CURVE('',#8795,#8796,#4437,.T.);
#11630=EDGE_CURVE('',#8797,#8797,#4438,.T.);
#11631=EDGE_CURVE('',#8774,#8759,#4439,.F.);
#11632=EDGE_CURVE('',#8759,#8776,#4440,.F.);
#11633=EDGE_CURVE('',#8772,#8757,#4441,.T.);
#11634=EDGE_CURVE('',#8776,#8772,#6103,.T.);
#11635=EDGE_CURVE('',#8788,#8798,#239,.T.);
#11636=EDGE_CURVE('',#8798,#8799,#6104,.T.);
#11637=EDGE_CURVE('',#8799,#8800,#4442,.T.);
#11638=EDGE_CURVE('',#8800,#8781,#6105,.T.);
#11639=EDGE_CURVE('',#8801,#8799,#4443,.T.);
#11640=EDGE_CURVE('',#8799,#8802,#6106,.T.);
#11641=EDGE_CURVE('',#8802,#8803,#4444,.T.);
#11642=EDGE_CURVE('',#8803,#8801,#6107,.T.);
#11643=EDGE_CURVE('',#8804,#8802,#4445,.T.);
#11644=EDGE_CURVE('',#8802,#8805,#6108,.T.);
#11645=EDGE_CURVE('',#8805,#8806,#4446,.T.);
#11646=EDGE_CURVE('',#8806,#8804,#6109,.T.);
#11647=EDGE_CURVE('',#8805,#8807,#4447,.T.);
#11648=EDGE_CURVE('',#8807,#8806,#4448,.T.);
#11649=EDGE_CURVE('',#8804,#8803,#4449,.T.);
#11650=EDGE_CURVE('',#8801,#8800,#4450,.T.);
#11651=EDGE_CURVE('',#8808,#8800,#6110,.T.);
#11652=EDGE_CURVE('',#8782,#8808,#6111,.T.);
#11653=EDGE_CURVE('',#8801,#8809,#6112,.T.);
#11654=EDGE_CURVE('',#8809,#8808,#4451,.T.);
#11655=EDGE_CURVE('',#8810,#8803,#6113,.T.);
#11656=EDGE_CURVE('',#8809,#8810,#6114,.T.);
#11657=EDGE_CURVE('',#8804,#8811,#6115,.T.);
#11658=EDGE_CURVE('',#8810,#8811,#4452,.T.);
#11659=EDGE_CURVE('',#8812,#8806,#6116,.T.);
#11660=EDGE_CURVE('',#8811,#8812,#6117,.T.);
#11661=EDGE_CURVE('',#8796,#8813,#4453,.T.);
#11662=EDGE_CURVE('',#8813,#8814,#4454,.T.);
#11663=EDGE_CURVE('',#8814,#8813,#4455,.T.);
#11664=EDGE_CURVE('',#8814,#8815,#6118,.T.);
#11665=EDGE_CURVE('',#8816,#8815,#4456,.T.);
#11666=EDGE_CURVE('',#8815,#8816,#4457,.T.);
#11667=EDGE_CURVE('',#8791,#8817,#4458,.T.);
#11668=EDGE_CURVE('',#8817,#8818,#4459,.T.);
#11669=EDGE_CURVE('',#8818,#8817,#4460,.T.);
#11670=EDGE_CURVE('',#8818,#8797,#6119,.T.);
#11671=EDGE_CURVE('',#8819,#8819,#4461,.T.);
#11672=EDGE_CURVE('',#8819,#8789,#4462,.T.);
#11673=EDGE_CURVE('',#8816,#8820,#4463,.T.);
#11674=EDGE_CURVE('',#8820,#8820,#4464,.T.);
#11675=EDGE_CURVE('',#8821,#8821,#4465,.T.);
#11676=EDGE_CURVE('',#8808,#8822,#4466,.T.);
#11677=EDGE_CURVE('',#8822,#8823,#6120,.T.);
#11678=EDGE_CURVE('',#8823,#8785,#240,.T.);
#11679=EDGE_CURVE('',#8809,#8822,#4467,.T.);
#11680=EDGE_CURVE('',#8823,#8824,#6121,.T.);
#11681=EDGE_CURVE('',#8824,#8825,#4468,.F.);
#11682=EDGE_CURVE('',#8825,#8786,#6122,.T.);
#11683=EDGE_CURVE('',#8826,#8822,#6123,.T.);
#11684=EDGE_CURVE('',#8824,#8826,#6124,.T.);
#11685=EDGE_CURVE('',#8826,#8810,#4469,.T.);
#11686=EDGE_CURVE('',#8805,#8798,#6125,.T.);
#11687=EDGE_CURVE('',#8811,#8826,#4470,.T.);
#11688=EDGE_CURVE('',#8787,#8807,#6126,.T.);
#11689=EDGE_CURVE('',#8825,#8812,#4471,.F.);
#11690=EDGE_CURVE('',#8812,#8824,#4472,.F.);
#11691=EDGE_CURVE('',#8807,#8825,#6127,.T.);
#11692=EDGE_CURVE('',#8821,#8827,#4473,.T.);
#11693=EDGE_CURVE('',#8827,#8828,#4474,.T.);
#11694=EDGE_CURVE('',#8828,#8827,#4475,.T.);
#11695=EDGE_CURVE('',#8829,#8830,#4476,.T.);
#11696=EDGE_CURVE('',#8829,#8828,#6128,.T.);
#11697=EDGE_CURVE('',#8830,#8829,#4477,.T.);
#11698=EDGE_CURVE('',#8830,#8831,#4478,.T.);
#11699=EDGE_CURVE('',#8831,#8831,#4479,.T.);
#11700=EDGE_CURVE('',#8832,#8832,#4480,.T.);
#11701=EDGE_CURVE('',#8832,#8819,#6129,.T.);
#11702=EDGE_CURVE('',#8833,#8834,#6130,.T.);
#11703=EDGE_CURVE('',#8835,#8833,#6131,.T.);
#11704=EDGE_CURVE('',#8834,#8835,#6132,.T.);
#11705=EDGE_CURVE('',#8836,#8837,#6133,.T.);
#11706=EDGE_CURVE('',#8838,#8836,#6134,.T.);
#11707=EDGE_CURVE('',#8837,#8838,#6135,.T.);
#11708=EDGE_CURVE('',#8839,#8840,#6136,.T.);
#11709=EDGE_CURVE('',#8841,#8839,#6137,.T.);
#11710=EDGE_CURVE('',#8840,#8841,#6138,.T.);
#11711=EDGE_CURVE('',#8842,#8843,#6139,.T.);
#11712=EDGE_CURVE('',#8844,#8842,#6140,.T.);
#11713=EDGE_CURVE('',#8843,#8844,#6141,.T.);
#11714=EDGE_CURVE('',#8833,#8844,#6142,.T.);
#11715=EDGE_CURVE('',#8842,#8835,#6143,.T.);
#11716=EDGE_CURVE('',#8845,#8846,#6144,.T.);
#11717=EDGE_CURVE('',#8847,#8845,#6145,.T.);
#11718=EDGE_CURVE('',#8846,#8847,#6146,.T.);
#11719=EDGE_CURVE('',#8848,#8849,#6147,.T.);
#11720=EDGE_CURVE('',#8850,#8848,#6148,.T.);
#11721=EDGE_CURVE('',#8849,#8850,#6149,.T.);
#11722=EDGE_CURVE('',#8836,#8850,#6150,.T.);
#11723=EDGE_CURVE('',#8848,#8838,#6151,.T.);
#11724=EDGE_CURVE('',#8851,#8852,#6152,.T.);
#11725=EDGE_CURVE('',#8853,#8851,#6153,.T.);
#11726=EDGE_CURVE('',#8852,#8853,#6154,.T.);
#11727=EDGE_CURVE('',#8851,#8841,#6155,.T.);
#11728=EDGE_CURVE('',#8839,#8853,#6156,.T.);
#11729=EDGE_CURVE('',#8843,#8852,#6157,.T.);
#11730=EDGE_CURVE('',#8853,#8842,#6158,.T.);
#11731=EDGE_CURVE('',#8854,#8855,#6159,.T.);
#11732=EDGE_CURVE('',#8856,#8854,#6160,.T.);
#11733=EDGE_CURVE('',#8855,#8856,#6161,.T.);
#11734=EDGE_CURVE('',#8845,#8856,#6162,.T.);
#11735=EDGE_CURVE('',#8854,#8847,#6163,.T.);
#11736=EDGE_CURVE('',#8852,#8855,#6164,.T.);
#11737=EDGE_CURVE('',#8856,#8851,#6165,.T.);
#11738=EDGE_CURVE('',#8855,#8849,#6166,.T.);
#11739=EDGE_CURVE('',#8850,#8854,#6167,.T.);
#11740=EDGE_CURVE('',#8849,#8843,#6168,.T.);
#11741=EDGE_CURVE('',#8844,#8848,#6169,.T.);
#11742=EDGE_CURVE('',#8837,#8846,#6170,.T.);
#11743=EDGE_CURVE('',#8847,#8836,#6171,.T.);
#11744=EDGE_CURVE('',#8846,#8840,#6172,.T.);
#11745=EDGE_CURVE('',#8841,#8845,#6173,.T.);
#11746=EDGE_CURVE('',#8840,#8834,#6174,.T.);
#11747=EDGE_CURVE('',#8835,#8839,#6175,.T.);
#11748=EDGE_CURVE('',#8834,#8837,#6176,.T.);
#11749=EDGE_CURVE('',#8838,#8833,#6177,.T.);
#11750=EDGE_CURVE('',#8857,#8857,#4481,.T.);
#11751=EDGE_CURVE('',#8857,#8858,#5356,.T.);
#11752=EDGE_CURVE('',#8858,#8858,#4482,.T.);
#11753=EDGE_CURVE('',#8859,#8859,#4483,.T.);
#11754=EDGE_CURVE('',#8859,#8860,#4484,.T.);
#11755=EDGE_CURVE('',#8860,#8861,#4485,.T.);
#11756=EDGE_CURVE('',#8861,#8860,#4486,.T.);
#11757=EDGE_CURVE('',#8862,#8863,#4487,.T.);
#11758=EDGE_CURVE('',#8863,#8862,#4488,.T.);
#11759=EDGE_CURVE('',#8863,#8861,#6178,.T.);
#11760=EDGE_CURVE('',#8864,#8865,#6179,.T.);
#11761=EDGE_CURVE('',#8866,#8865,#4489,.F.);
#11762=EDGE_CURVE('',#8867,#8866,#4490,.T.);
#11763=EDGE_CURVE('',#8868,#8867,#4491,.F.);
#11764=EDGE_CURVE('',#8868,#8869,#6180,.T.);
#11765=EDGE_CURVE('',#8870,#8869,#6181,.T.);
#11766=EDGE_CURVE('',#8870,#8871,#6182,.T.);
#11767=EDGE_CURVE('',#8872,#8871,#4492,.F.);
#11768=EDGE_CURVE('',#8873,#8872,#4493,.T.);
#11769=EDGE_CURVE('',#8874,#8873,#4494,.T.);
#11770=EDGE_CURVE('',#8875,#8874,#4495,.F.);
#11771=EDGE_CURVE('',#8875,#8876,#6183,.T.);
#11772=EDGE_CURVE('',#8877,#8876,#6184,.T.);
#11773=EDGE_CURVE('',#8877,#8878,#6185,.T.);
#11774=EDGE_CURVE('',#8879,#8878,#4496,.F.);
#11775=EDGE_CURVE('',#8880,#8879,#4497,.T.);
#11776=EDGE_CURVE('',#8881,#8880,#4498,.F.);
#11777=EDGE_CURVE('',#8881,#8882,#6186,.T.);
#11778=EDGE_CURVE('',#8883,#8882,#6187,.T.);
#11779=EDGE_CURVE('',#8883,#8884,#6188,.T.);
#11780=EDGE_CURVE('',#8885,#8884,#4499,.F.);
#11781=EDGE_CURVE('',#8886,#8885,#4500,.T.);
#11782=EDGE_CURVE('',#8887,#8886,#4501,.F.);
#11783=EDGE_CURVE('',#8887,#8888,#6189,.T.);
#11784=EDGE_CURVE('',#8864,#8888,#6190,.T.);
#11785=EDGE_CURVE('',#8862,#8889,#4502,.T.);
#11786=EDGE_CURVE('',#8889,#8889,#4503,.T.);
#11787=EDGE_CURVE('',#8890,#8891,#6191,.T.);
#11788=EDGE_CURVE('',#8891,#8892,#4504,.T.);
#11789=EDGE_CURVE('',#8892,#8893,#6192,.T.);
#11790=EDGE_CURVE('',#8894,#8893,#6193,.T.);
#11791=EDGE_CURVE('',#8894,#8895,#6194,.T.);
#11792=EDGE_CURVE('',#8895,#8896,#4505,.T.);
#11793=EDGE_CURVE('',#8896,#8897,#6195,.T.);
#11794=EDGE_CURVE('',#8898,#8897,#6196,.T.);
#11795=EDGE_CURVE('',#8898,#8899,#6197,.T.);
#11796=EDGE_CURVE('',#8899,#8900,#4506,.T.);
#11797=EDGE_CURVE('',#8901,#8900,#4507,.F.);
#11798=EDGE_CURVE('',#8901,#8902,#6198,.T.);
#11799=EDGE_CURVE('',#8903,#8902,#6199,.T.);
#11800=EDGE_CURVE('',#8903,#8904,#6200,.T.);
#11801=EDGE_CURVE('',#8905,#8904,#4508,.F.);
#11802=EDGE_CURVE('',#8905,#8906,#4509,.T.);
#11803=EDGE_CURVE('',#8906,#8907,#6201,.T.);
#11804=EDGE_CURVE('',#8890,#8907,#6202,.T.);
#11805=EDGE_CURVE('',#8888,#8908,#4510,.F.);
#11806=EDGE_CURVE('',#8908,#8909,#6203,.T.);
#11807=EDGE_CURVE('',#8909,#8864,#4511,.F.);
#11808=EDGE_CURVE('',#8908,#8910,#6204,.T.);
#11809=EDGE_CURVE('',#8911,#8910,#6205,.T.);
#11810=EDGE_CURVE('',#8909,#8911,#6206,.T.);
#11811=EDGE_CURVE('',#8907,#8911,#4512,.F.);
#11812=EDGE_CURVE('',#8910,#8890,#4513,.F.);
#11813=EDGE_CURVE('',#8882,#8912,#4514,.F.);
#11814=EDGE_CURVE('',#8912,#8913,#6207,.T.);
#11815=EDGE_CURVE('',#8913,#8883,#4515,.F.);
#11816=EDGE_CURVE('',#8912,#8914,#6208,.T.);
#11817=EDGE_CURVE('',#8915,#8914,#6209,.T.);
#11818=EDGE_CURVE('',#8913,#8915,#6210,.T.);
#11819=EDGE_CURVE('',#8893,#8915,#4516,.F.);
#11820=EDGE_CURVE('',#8914,#8894,#4517,.F.);
#11821=EDGE_CURVE('',#8876,#8916,#4518,.F.);
#11822=EDGE_CURVE('',#8916,#8917,#6211,.T.);
#11823=EDGE_CURVE('',#8917,#8877,#4519,.F.);
#11824=EDGE_CURVE('',#8916,#8918,#6212,.T.);
#11825=EDGE_CURVE('',#8919,#8918,#6213,.T.);
#11826=EDGE_CURVE('',#8917,#8919,#6214,.T.);
#11827=EDGE_CURVE('',#8897,#8919,#4520,.F.);
#11828=EDGE_CURVE('',#8918,#8898,#4521,.F.);
#11829=EDGE_CURVE('',#8920,#8921,#4522,.T.);
#11830=EDGE_CURVE('',#8921,#8922,#4523,.T.);
#11831=EDGE_CURVE('',#8922,#8923,#4524,.T.);
#11832=EDGE_CURVE('',#8923,#8920,#4525,.T.);
#11833=EDGE_CURVE('',#8922,#8924,#4526,.T.);
#11834=EDGE_CURVE('',#8924,#8923,#4527,.T.);
#11835=EDGE_CURVE('',#8925,#8920,#4528,.T.);
#11836=EDGE_CURVE('',#8920,#8926,#6215,.T.);
#11837=EDGE_CURVE('',#8926,#8927,#4529,.T.);
#11838=EDGE_CURVE('',#8927,#8925,#6216,.T.);
#11839=EDGE_CURVE('',#8926,#8928,#4530,.T.);
#11840=EDGE_CURVE('',#8928,#8927,#4531,.T.);
#11841=EDGE_CURVE('',#8925,#8921,#4532,.T.);
#11842=EDGE_CURVE('',#8924,#8929,#6217,.T.);
#11843=EDGE_CURVE('',#8929,#8930,#4533,.T.);
#11844=EDGE_CURVE('',#8930,#8923,#6218,.T.);
#11845=EDGE_CURVE('',#8922,#8931,#5357,.T.);
#11846=EDGE_CURVE('',#8932,#8931,#4534,.T.);
#11847=EDGE_CURVE('',#8932,#8924,#5358,.T.);
#11848=EDGE_CURVE('',#8933,#8921,#5359,.T.);
#11849=EDGE_CURVE('',#8931,#8933,#4535,.T.);
#11850=EDGE_CURVE('',#8925,#8934,#5360,.T.);
#11851=EDGE_CURVE('',#8934,#8933,#4536,.T.);
#11852=EDGE_CURVE('',#8935,#8927,#6219,.T.);
#11853=EDGE_CURVE('',#8936,#8935,#5361,.T.);
#11854=EDGE_CURVE('',#8936,#8937,#6220,.T.);
#11855=EDGE_CURVE('',#8934,#8937,#6221,.T.);
#11856=EDGE_CURVE('',#8938,#8939,#5362,.T.);
#11857=EDGE_CURVE('',#8938,#8940,#6222,.T.);
#11858=EDGE_CURVE('',#8940,#8934,#4537,.T.);
#11859=EDGE_CURVE('',#8939,#8937,#4538,.T.);
#11860=EDGE_CURVE('',#8940,#8933,#4539,.T.);
#11861=EDGE_CURVE('',#8926,#8930,#4540,.T.);
#11862=EDGE_CURVE('',#8940,#8941,#4541,.T.);
#11863=EDGE_CURVE('',#8931,#8941,#4542,.T.);
#11864=EDGE_CURVE('',#8942,#8943,#4543,.T.);
#11865=EDGE_CURVE('',#8942,#8944,#6223,.T.);
#11866=EDGE_CURVE('',#8944,#8945,#4544,.T.);
#11867=EDGE_CURVE('',#8946,#8945,#6224,.T.);
#11868=EDGE_CURVE('',#8946,#8947,#4545,.T.);
#11869=EDGE_CURVE('',#8948,#8947,#6225,.T.);
#11870=EDGE_CURVE('',#8949,#8948,#4546,.T.);
#11871=EDGE_CURVE('',#8950,#8949,#6226,.T.);
#11872=EDGE_CURVE('',#8951,#8950,#4547,.T.);
#11873=EDGE_CURVE('',#8952,#8951,#6227,.T.);
#11874=EDGE_CURVE('',#8952,#8953,#4548,.T.);
#11875=EDGE_CURVE('',#8954,#8953,#6228,.T.);
#11876=EDGE_CURVE('',#8955,#8954,#4549,.T.);
#11877=EDGE_CURVE('',#8956,#8955,#6229,.T.);
#11878=EDGE_CURVE('',#8957,#8956,#4550,.T.);
#11879=EDGE_CURVE('',#8941,#8957,#6230,.T.);
#11880=EDGE_CURVE('',#8938,#8944,#4551,.T.);
#11881=EDGE_CURVE('',#8943,#8942,#4552,.T.);
#11882=EDGE_CURVE('',#8958,#8959,#4553,.F.);
#11883=EDGE_CURVE('',#8959,#8960,#6231,.T.);
#11884=EDGE_CURVE('',#8960,#8954,#4554,.T.);
#11885=EDGE_CURVE('',#8953,#8958,#5363,.F.);
#11886=EDGE_CURVE('',#8960,#8961,#4555,.T.);
#11887=EDGE_CURVE('',#8961,#8954,#4556,.T.);
#11888=EDGE_CURVE('',#8962,#8963,#4557,.T.);
#11889=EDGE_CURVE('',#8963,#8964,#4558,.T.);
#11890=EDGE_CURVE('',#8964,#8962,#4559,.T.);
#11891=EDGE_CURVE('',#8962,#8961,#5364,.T.);
#11892=EDGE_CURVE('',#8960,#8963,#5365,.T.);
#11893=EDGE_CURVE('',#8961,#8965,#4560,.T.);
#11894=EDGE_CURVE('',#8955,#8965,#4561,.T.);
#11895=EDGE_CURVE('',#8966,#8962,#4562,.T.);
#11896=EDGE_CURVE('',#8965,#8966,#5366,.T.);
#11897=EDGE_CURVE('',#8964,#8967,#4563,.T.);
#11898=EDGE_CURVE('',#8967,#8966,#4564,.T.);
#11899=EDGE_CURVE('',#8952,#8968,#5367,.F.);
#11900=EDGE_CURVE('',#8968,#8958,#4565,.T.);
#11901=EDGE_CURVE('',#8969,#8968,#4566,.F.);
#11902=EDGE_CURVE('',#8970,#8969,#6232,.T.);
#11903=EDGE_CURVE('',#8971,#8970,#4567,.T.);
#11904=EDGE_CURVE('',#8959,#8971,#6233,.T.);
#11905=EDGE_CURVE('',#8972,#8973,#4568,.T.);
#11906=EDGE_CURVE('',#8973,#8974,#4569,.T.);
#11907=EDGE_CURVE('',#8974,#8972,#4570,.T.);
#11908=EDGE_CURVE('',#8950,#8975,#4571,.T.);
#11909=EDGE_CURVE('',#8975,#8976,#4572,.T.);
#11910=EDGE_CURVE('',#8976,#8951,#4573,.T.);
#11911=EDGE_CURVE('',#8977,#8975,#4574,.T.);
#11912=EDGE_CURVE('',#8950,#8977,#4575,.T.);
#11913=EDGE_CURVE('',#8976,#8978,#4576,.T.);
#11914=EDGE_CURVE('',#8978,#8951,#4577,.T.);
#11915=EDGE_CURVE('',#8979,#8980,#4578,.T.);
#11916=EDGE_CURVE('',#8980,#8981,#4579,.T.);
#11917=EDGE_CURVE('',#8981,#8979,#4580,.T.);
#11918=EDGE_CURVE('',#8979,#8978,#5368,.T.);
#11919=EDGE_CURVE('',#8976,#8980,#5369,.T.);
#11920=EDGE_CURVE('',#8977,#8973,#5370,.T.);
#11921=EDGE_CURVE('',#8972,#8975,#5371,.T.);
#11922=EDGE_CURVE('',#8982,#8949,#5372,.F.);
#11923=EDGE_CURVE('',#8982,#8983,#4581,.F.);
#11924=EDGE_CURVE('',#8983,#8977,#6234,.T.);
#11925=EDGE_CURVE('',#8978,#8969,#6235,.T.);
#11926=EDGE_CURVE('',#8984,#8979,#6236,.T.);
#11927=EDGE_CURVE('',#8985,#8984,#6237,.T.);
#11928=EDGE_CURVE('',#8985,#8970,#5373,.T.);
#11929=EDGE_CURVE('',#8981,#8986,#6238,.T.);
#11930=EDGE_CURVE('',#8986,#8984,#4582,.F.);
#11931=EDGE_CURVE('',#8939,#8987,#4583,.T.);
#11932=EDGE_CURVE('',#8987,#8945,#5374,.F.);
#11933=EDGE_CURVE('',#8988,#8936,#4584,.T.);
#11934=EDGE_CURVE('',#8989,#8988,#6239,.T.);
#11935=EDGE_CURVE('',#8987,#8989,#4585,.F.);
#11936=EDGE_CURVE('',#8941,#8932,#4586,.T.);
#11937=EDGE_CURVE('',#8929,#8990,#4587,.T.);
#11938=EDGE_CURVE('',#8990,#8930,#4588,.T.);
#11939=EDGE_CURVE('',#8929,#8991,#6240,.T.);
#11940=EDGE_CURVE('',#8991,#8992,#5375,.T.);
#11941=EDGE_CURVE('',#8992,#8990,#6241,.T.);
#11942=EDGE_CURVE('',#8993,#8932,#6242,.T.);
#11943=EDGE_CURVE('',#8993,#8994,#6243,.T.);
#11944=EDGE_CURVE('',#8991,#8994,#5376,.T.);
#11945=EDGE_CURVE('',#8957,#8995,#5377,.T.);
#11946=EDGE_CURVE('',#8995,#8993,#4589,.T.);
#11947=EDGE_CURVE('',#8996,#8966,#4590,.T.);
#11948=EDGE_CURVE('',#8967,#8996,#4591,.T.);
#11949=EDGE_CURVE('',#8997,#8965,#4592,.T.);
#11950=EDGE_CURVE('',#8996,#8997,#5378,.T.);
#11951=EDGE_CURVE('',#8955,#8997,#4593,.T.);
#11952=EDGE_CURVE('',#8997,#8998,#6244,.T.);
#11953=EDGE_CURVE('',#8998,#8999,#4594,.T.);
#11954=EDGE_CURVE('',#8999,#8956,#5379,.T.);
#11955=EDGE_CURVE('',#8999,#8995,#4595,.T.);
#11956=EDGE_CURVE('',#9000,#8996,#6245,.T.);
#11957=EDGE_CURVE('',#9001,#9000,#6246,.T.);
#11958=EDGE_CURVE('',#9002,#9001,#5380,.T.);
#11959=EDGE_CURVE('',#9002,#8998,#6247,.T.);
#11960=EDGE_CURVE('',#8967,#9003,#6248,.T.);
#11961=EDGE_CURVE('',#9003,#9000,#4596,.T.);
#11962=EDGE_CURVE('',#9004,#8964,#6249,.T.);
#11963=EDGE_CURVE('',#9003,#9004,#4597,.T.);
#11964=EDGE_CURVE('',#8963,#9005,#6250,.T.);
#11965=EDGE_CURVE('',#9005,#9004,#4598,.T.);
#11966=EDGE_CURVE('',#9005,#9006,#4599,.T.);
#11967=EDGE_CURVE('',#9006,#9004,#4600,.T.);
#11968=EDGE_CURVE('',#8948,#9007,#5381,.F.);
#11969=EDGE_CURVE('',#9007,#8982,#4601,.T.);
#11970=EDGE_CURVE('',#9008,#9007,#4602,.F.);
#11971=EDGE_CURVE('',#9009,#9008,#6251,.T.);
#11972=EDGE_CURVE('',#9010,#9009,#4603,.T.);
#11973=EDGE_CURVE('',#8983,#9010,#6252,.T.);
#11974=EDGE_CURVE('',#9011,#9012,#5382,.T.);
#11975=EDGE_CURVE('',#9011,#9013,#4604,.T.);
#11976=EDGE_CURVE('',#9013,#9014,#5383,.F.);
#11977=EDGE_CURVE('',#9014,#9010,#5384,.F.);
#11978=EDGE_CURVE('',#9012,#9009,#5385,.T.);
#11979=EDGE_CURVE('',#9006,#9015,#4605,.T.);
#11980=EDGE_CURVE('',#9015,#9003,#4606,.T.);
#11981=EDGE_CURVE('',#9005,#9016,#6253,.T.);
#11982=EDGE_CURVE('',#9016,#9017,#5386,.T.);
#11983=EDGE_CURVE('',#9017,#9006,#6254,.T.);
#11984=EDGE_CURVE('',#9018,#8985,#5387,.T.);
#11985=EDGE_CURVE('',#9018,#9017,#4607,.T.);
#11986=EDGE_CURVE('',#9016,#8971,#5388,.T.);
#11987=EDGE_CURVE('',#9015,#9000,#4608,.T.);
#11988=EDGE_CURVE('',#9015,#9019,#6255,.T.);
#11989=EDGE_CURVE('',#9019,#9001,#5389,.T.);
#11990=EDGE_CURVE('',#8886,#9020,#6256,.T.);
#11991=EDGE_CURVE('',#8885,#9021,#6257,.T.);
#11992=EDGE_CURVE('',#9022,#9021,#4609,.T.);
#11993=EDGE_CURVE('',#8880,#9022,#6258,.T.);
#11994=EDGE_CURVE('',#8879,#9023,#6259,.T.);
#11995=EDGE_CURVE('',#9024,#9023,#4610,.T.);
#11996=EDGE_CURVE('',#8874,#9024,#6260,.T.);
#11997=EDGE_CURVE('',#8873,#9025,#6261,.T.);
#11998=EDGE_CURVE('',#9026,#9025,#4611,.T.);
#11999=EDGE_CURVE('',#8928,#9026,#6262,.T.);
#12000=EDGE_CURVE('',#8990,#8928,#4612,.T.);
#12001=EDGE_CURVE('',#9019,#8992,#4613,.T.);
#12002=EDGE_CURVE('',#9018,#9027,#6263,.T.);
#12003=EDGE_CURVE('',#9028,#9027,#4614,.T.);
#12004=EDGE_CURVE('',#9028,#9013,#6264,.T.);
#12005=EDGE_CURVE('',#9011,#9029,#6265,.T.);
#12006=EDGE_CURVE('',#9030,#9029,#4615,.T.);
#12007=EDGE_CURVE('',#9031,#9030,#6266,.T.);
#12008=EDGE_CURVE('',#9025,#9031,#4616,.T.);
#12009=EDGE_CURVE('',#9032,#8872,#6267,.T.);
#12010=EDGE_CURVE('',#9033,#9032,#4617,.T.);
#12011=EDGE_CURVE('',#8867,#9033,#6268,.T.);
#12012=EDGE_CURVE('',#8866,#9034,#6269,.T.);
#12013=EDGE_CURVE('',#9020,#9034,#4618,.T.);
#12014=EDGE_CURVE('',#9035,#8887,#6270,.T.);
#12015=EDGE_CURVE('',#9020,#9035,#5390,.T.);
#12016=EDGE_CURVE('',#9034,#9036,#5391,.F.);
#12017=EDGE_CURVE('',#9036,#9037,#5392,.F.);
#12018=EDGE_CURVE('',#9037,#9038,#4619,.T.);
#12019=EDGE_CURVE('',#9038,#9035,#5393,.T.);
#12020=EDGE_CURVE('',#9037,#9039,#6271,.T.);
#12021=EDGE_CURVE('',#9039,#9040,#6272,.T.);
#12022=EDGE_CURVE('',#9040,#9038,#6273,.T.);
#12023=EDGE_CURVE('',#9041,#8875,#6274,.T.);
#12024=EDGE_CURVE('',#9024,#9041,#5394,.T.);
#12025=EDGE_CURVE('',#9023,#9042,#5395,.F.);
#12026=EDGE_CURVE('',#9042,#9043,#5396,.F.);
#12027=EDGE_CURVE('',#9043,#9044,#4620,.T.);
#12028=EDGE_CURVE('',#9044,#9041,#5397,.T.);
#12029=EDGE_CURVE('',#9043,#9045,#6275,.T.);
#12030=EDGE_CURVE('',#9045,#9046,#6276,.T.);
#12031=EDGE_CURVE('',#9046,#9044,#6277,.T.);
#12032=EDGE_CURVE('',#9026,#8935,#5398,.T.);
#12033=EDGE_CURVE('',#9029,#9047,#4621,.T.);
#12034=EDGE_CURVE('',#9047,#9048,#4622,.T.);
#12035=EDGE_CURVE('',#9048,#9049,#5399,.T.);
#12036=EDGE_CURVE('',#9049,#9030,#5400,.T.);
#12037=EDGE_CURVE('',#9029,#9050,#4623,.T.);
#12038=EDGE_CURVE('',#9050,#9047,#4624,.T.);
#12039=EDGE_CURVE('',#9049,#9051,#6278,.T.);
#12040=EDGE_CURVE('',#9051,#9031,#5401,.T.);
#12041=EDGE_CURVE('',#9051,#8988,#5402,.T.);
#12042=EDGE_CURVE('',#8994,#9002,#4625,.T.);
#12043=EDGE_CURVE('',#9012,#9050,#6279,.T.);
#12044=EDGE_CURVE('',#9050,#9052,#6280,.T.);
#12045=EDGE_CURVE('',#9052,#9053,#4626,.T.);
#12046=EDGE_CURVE('',#9053,#9047,#6281,.T.);
#12047=EDGE_CURVE('',#8947,#9053,#5403,.T.);
#12048=EDGE_CURVE('',#9052,#8947,#4627,.T.);
#12049=EDGE_CURVE('',#9052,#9008,#6282,.T.);
#12050=EDGE_CURVE('',#8974,#8981,#4628,.T.);
#12051=EDGE_CURVE('',#8980,#8972,#4629,.T.);
#12052=EDGE_CURVE('',#9054,#8974,#6283,.T.);
#12053=EDGE_CURVE('',#8986,#9054,#4630,.T.);
#12054=EDGE_CURVE('',#8973,#9055,#6284,.T.);
#12055=EDGE_CURVE('',#9055,#9054,#4631,.F.);
#12056=EDGE_CURVE('',#9028,#9055,#4632,.F.);
#12057=EDGE_CURVE('',#9054,#9028,#4633,.F.);
#12058=EDGE_CURVE('',#9027,#8986,#4634,.F.);
#12059=EDGE_CURVE('',#8984,#9027,#4635,.F.);
#12060=EDGE_CURVE('',#9055,#9014,#6285,.T.);
#12061=EDGE_CURVE('',#9056,#9053,#4636,.T.);
#12062=EDGE_CURVE('',#9057,#9056,#4637,.T.);
#12063=EDGE_CURVE('',#9057,#9048,#6286,.T.);
#12064=EDGE_CURVE('',#9056,#8946,#5404,.T.);
#12065=EDGE_CURVE('',#8989,#9057,#6287,.T.);
#12066=EDGE_CURVE('',#9022,#9058,#5405,.F.);
#12067=EDGE_CURVE('',#9058,#8881,#6288,.T.);
#12068=EDGE_CURVE('',#9059,#9058,#5406,.F.);
#12069=EDGE_CURVE('',#9060,#9059,#6289,.T.);
#12070=EDGE_CURVE('',#9060,#9061,#6290,.T.);
#12071=EDGE_CURVE('',#9062,#9061,#5407,.F.);
#12072=EDGE_CURVE('',#9062,#9063,#828,.T.);
#12073=EDGE_CURVE('',#9063,#9064,#5408,.T.);
#12074=EDGE_CURVE('',#9065,#9064,#6291,.T.);
#12075=EDGE_CURVE('',#9066,#9065,#5409,.T.);
#12076=EDGE_CURVE('',#8895,#9066,#6292,.T.);
#12077=EDGE_CURVE('',#9067,#9068,#5410,.F.);
#12078=EDGE_CURVE('',#9068,#9059,#4638,.T.);
#12079=EDGE_CURVE('',#9021,#9067,#5411,.F.);
#12080=EDGE_CURVE('',#9068,#9069,#6293,.T.);
#12081=EDGE_CURVE('',#9069,#9060,#6294,.T.);
#12082=EDGE_CURVE('',#9070,#9071,#4639,.T.);
#12083=EDGE_CURVE('',#9071,#9070,#4640,.T.);
#12084=EDGE_CURVE('',#9070,#8943,#4641,.T.);
#12085=EDGE_CURVE('',#9072,#9073,#829,.T.);
#12086=EDGE_CURVE('',#9074,#9072,#4642,.T.);
#12087=EDGE_CURVE('',#9074,#9071,#6295,.T.);
#12088=EDGE_CURVE('',#9075,#9074,#4643,.T.);
#12089=EDGE_CURVE('',#9076,#9075,#830,.T.);
#12090=EDGE_CURVE('',#9077,#9076,#5412,.T.);
#12091=EDGE_CURVE('',#9078,#9077,#831,.T.);
#12092=EDGE_CURVE('',#9063,#9078,#4644,.T.);
#12093=EDGE_CURVE('',#9079,#9062,#5413,.T.);
#12094=EDGE_CURVE('',#9080,#9079,#832,.T.);
#12095=EDGE_CURVE('',#9081,#9080,#4645,.T.);
#12096=EDGE_CURVE('',#9082,#9081,#833,.T.);
#12097=EDGE_CURVE('',#9073,#9082,#5414,.T.);
#12098=EDGE_CURVE('',#8878,#9042,#6296,.T.);
#12099=EDGE_CURVE('',#9083,#8896,#6297,.T.);
#12100=EDGE_CURVE('',#9084,#9083,#5415,.T.);
#12101=EDGE_CURVE('',#9084,#9085,#6298,.T.);
#12102=EDGE_CURVE('',#9085,#9078,#5416,.T.);
#12103=EDGE_CURVE('',#9077,#9086,#5417,.T.);
#12104=EDGE_CURVE('',#9045,#9086,#6299,.T.);
#12105=EDGE_CURVE('',#8884,#9067,#6300,.T.);
#12106=EDGE_CURVE('',#9087,#8892,#6301,.T.);
#12107=EDGE_CURVE('',#9088,#9087,#5418,.T.);
#12108=EDGE_CURVE('',#9088,#9089,#6302,.T.);
#12109=EDGE_CURVE('',#9089,#9080,#5419,.T.);
#12110=EDGE_CURVE('',#9079,#9090,#5420,.T.);
#12111=EDGE_CURVE('',#9069,#9090,#6303,.T.);
#12112=EDGE_CURVE('',#8865,#9036,#6304,.T.);
#12113=EDGE_CURVE('',#9091,#8906,#6305,.T.);
#12114=EDGE_CURVE('',#9092,#9091,#5421,.T.);
#12115=EDGE_CURVE('',#9092,#9093,#6306,.T.);
#12116=EDGE_CURVE('',#9093,#9072,#5422,.T.);
#12117=EDGE_CURVE('',#9073,#9094,#5423,.T.);
#12118=EDGE_CURVE('',#9039,#9094,#6307,.T.);
#12119=EDGE_CURVE('',#9095,#9096,#5424,.T.);
#12120=EDGE_CURVE('',#9096,#9097,#6308,.T.);
#12121=EDGE_CURVE('',#9097,#9098,#4646,.T.);
#12122=EDGE_CURVE('',#9098,#9099,#6309,.T.);
#12123=EDGE_CURVE('',#9099,#9095,#241,.F.);
#12124=EDGE_CURVE('',#9091,#9100,#4647,.T.);
#12125=EDGE_CURVE('',#9100,#9097,#4648,.T.);
#12126=EDGE_CURVE('',#9097,#9092,#4649,.T.);
#12127=EDGE_CURVE('',#9100,#9098,#4650,.T.);
#12128=EDGE_CURVE('',#9100,#8905,#6310,.T.);
#12129=EDGE_CURVE('',#8904,#9098,#6311,.T.);
#12130=EDGE_CURVE('',#9093,#9096,#4651,.T.);
#12131=EDGE_CURVE('',#9082,#9101,#5425,.F.);
#12132=EDGE_CURVE('',#9101,#9094,#5426,.T.);
#12133=EDGE_CURVE('',#9040,#9101,#6312,.T.);
#12134=EDGE_CURVE('',#9081,#9102,#5427,.T.);
#12135=EDGE_CURVE('',#9089,#9102,#4652,.T.);
#12136=EDGE_CURVE('',#9103,#9102,#6313,.T.);
#12137=EDGE_CURVE('',#9103,#9088,#4653,.T.);
#12138=EDGE_CURVE('',#9087,#9104,#4654,.T.);
#12139=EDGE_CURVE('',#9104,#9103,#5428,.T.);
#12140=EDGE_CURVE('',#9061,#9090,#5429,.T.);
#12141=EDGE_CURVE('',#9085,#9064,#4655,.T.);
#12142=EDGE_CURVE('',#9065,#9084,#4656,.T.);
#12143=EDGE_CURVE('',#9083,#9066,#4657,.T.);
#12144=EDGE_CURVE('',#9076,#9105,#5430,.F.);
#12145=EDGE_CURVE('',#9105,#9086,#5431,.T.);
#12146=EDGE_CURVE('',#9046,#9105,#6314,.T.);
#12147=EDGE_CURVE('',#9106,#9107,#6315,.T.);
#12148=EDGE_CURVE('',#9108,#9107,#4658,.T.);
#12149=EDGE_CURVE('',#9109,#9108,#6316,.T.);
#12150=EDGE_CURVE('',#9106,#9109,#4659,.T.);
#12151=EDGE_CURVE('',#9110,#9106,#5432,.T.);
#12152=EDGE_CURVE('',#9109,#9111,#4660,.T.);
#12153=EDGE_CURVE('',#9111,#9110,#4661,.T.);
#12154=EDGE_CURVE('',#9108,#9112,#5433,.T.);
#12155=EDGE_CURVE('',#9113,#9112,#242,.T.);
#12156=EDGE_CURVE('',#9113,#9114,#6317,.T.);
#12157=EDGE_CURVE('',#9114,#9109,#4662,.T.);
#12158=EDGE_CURVE('',#9114,#9111,#4663,.T.);
#12159=EDGE_CURVE('',#8900,#9111,#6318,.T.);
#12160=EDGE_CURVE('',#8899,#9110,#6319,.T.);
#12161=EDGE_CURVE('',#9114,#8901,#6320,.T.);
#12162=EDGE_CURVE('',#9115,#9113,#6321,.T.);
#12163=EDGE_CURVE('',#9116,#9115,#6322,.T.);
#12164=EDGE_CURVE('',#9117,#9116,#5434,.T.);
#12165=EDGE_CURVE('',#8871,#9117,#6323,.T.);
#12166=EDGE_CURVE('',#9118,#8870,#4664,.F.);
#12167=EDGE_CURVE('',#9118,#9119,#6324,.T.);
#12168=EDGE_CURVE('',#8902,#9119,#4665,.F.);
#12169=EDGE_CURVE('',#9120,#9095,#5435,.T.);
#12170=EDGE_CURVE('',#9120,#9121,#5436,.T.);
#12171=EDGE_CURVE('',#9112,#9121,#5437,.T.);
#12172=EDGE_CURVE('',#9075,#9107,#5438,.T.);
#12173=EDGE_CURVE('',#9099,#9113,#6325,.T.);
#12174=EDGE_CURVE('',#9122,#8903,#4666,.F.);
#12175=EDGE_CURVE('',#9123,#9122,#6326,.T.);
#12176=EDGE_CURVE('',#8869,#9123,#4667,.F.);
#12177=EDGE_CURVE('',#9124,#8868,#6327,.T.);
#12178=EDGE_CURVE('',#9125,#9124,#5439,.T.);
#12179=EDGE_CURVE('',#9126,#9125,#6328,.T.);
#12180=EDGE_CURVE('',#9126,#9099,#6329,.T.);
#12181=EDGE_CURVE('',#9115,#9126,#6330,.T.);
#12182=EDGE_CURVE('',#9123,#9118,#6331,.T.);
#12183=EDGE_CURVE('',#9119,#9122,#6332,.T.);
#12184=EDGE_CURVE('',#9117,#9032,#5440,.T.);
#12185=EDGE_CURVE('',#9033,#9124,#5441,.T.);
#12186=EDGE_CURVE('',#9116,#9125,#4668,.T.);
#12187=EDGE_CURVE('',#8891,#9104,#6333,.T.);
#12188=ORIENTED_EDGE('',*,*,#9127,.F.);
#12189=ORIENTED_EDGE('',*,*,#9128,.T.);
#12190=ORIENTED_EDGE('',*,*,#9129,.T.);
#12191=ORIENTED_EDGE('',*,*,#9130,.T.);
#12192=ORIENTED_EDGE('',*,*,#9131,.T.);
#12193=ORIENTED_EDGE('',*,*,#9132,.T.);
#12194=ORIENTED_EDGE('',*,*,#9133,.T.);
#12195=ORIENTED_EDGE('',*,*,#9134,.T.);
#12196=ORIENTED_EDGE('',*,*,#9135,.T.);
#12197=ORIENTED_EDGE('',*,*,#9134,.F.);
#12198=ORIENTED_EDGE('',*,*,#9136,.T.);
#12199=ORIENTED_EDGE('',*,*,#9137,.T.);
#12200=ORIENTED_EDGE('',*,*,#9138,.T.);
#12201=ORIENTED_EDGE('',*,*,#9130,.F.);
#12202=ORIENTED_EDGE('',*,*,#9139,.T.);
#12203=ORIENTED_EDGE('',*,*,#9140,.T.);
#12204=ORIENTED_EDGE('',*,*,#9141,.T.);
#12205=ORIENTED_EDGE('',*,*,#9142,.T.);
#12206=ORIENTED_EDGE('',*,*,#9143,.T.);
#12207=ORIENTED_EDGE('',*,*,#9144,.T.);
#12208=ORIENTED_EDGE('',*,*,#9145,.F.);
#12209=ORIENTED_EDGE('',*,*,#9146,.T.);
#12210=ORIENTED_EDGE('',*,*,#9127,.T.);
#12211=ORIENTED_EDGE('',*,*,#9147,.T.);
#12212=ORIENTED_EDGE('',*,*,#9148,.F.);
#12213=ORIENTED_EDGE('',*,*,#9149,.T.);
#12214=ORIENTED_EDGE('',*,*,#9145,.T.);
#12215=ORIENTED_EDGE('',*,*,#9150,.T.);
#12216=ORIENTED_EDGE('',*,*,#9151,.F.);
#12217=ORIENTED_EDGE('',*,*,#9152,.T.);
#12218=ORIENTED_EDGE('',*,*,#9148,.T.);
#12219=ORIENTED_EDGE('',*,*,#9153,.T.);
#12220=ORIENTED_EDGE('',*,*,#9154,.F.);
#12221=ORIENTED_EDGE('',*,*,#9155,.T.);
#12222=ORIENTED_EDGE('',*,*,#9151,.T.);
#12223=ORIENTED_EDGE('',*,*,#9156,.T.);
#12224=ORIENTED_EDGE('',*,*,#9157,.F.);
#12225=ORIENTED_EDGE('',*,*,#9158,.T.);
#12226=ORIENTED_EDGE('',*,*,#9154,.T.);
#12227=ORIENTED_EDGE('',*,*,#9159,.T.);
#12228=ORIENTED_EDGE('',*,*,#9160,.F.);
#12229=ORIENTED_EDGE('',*,*,#9161,.T.);
#12230=ORIENTED_EDGE('',*,*,#9157,.T.);
#12231=ORIENTED_EDGE('',*,*,#9162,.T.);
#12232=ORIENTED_EDGE('',*,*,#9163,.F.);
#12233=ORIENTED_EDGE('',*,*,#9164,.T.);
#12234=ORIENTED_EDGE('',*,*,#9160,.T.);
#12235=ORIENTED_EDGE('',*,*,#9165,.T.);
#12236=ORIENTED_EDGE('',*,*,#9166,.F.);
#12237=ORIENTED_EDGE('',*,*,#9167,.T.);
#12238=ORIENTED_EDGE('',*,*,#9163,.T.);
#12239=ORIENTED_EDGE('',*,*,#9168,.T.);
#12240=ORIENTED_EDGE('',*,*,#9169,.F.);
#12241=ORIENTED_EDGE('',*,*,#9170,.T.);
#12242=ORIENTED_EDGE('',*,*,#9166,.T.);
#12243=ORIENTED_EDGE('',*,*,#9171,.T.);
#12244=ORIENTED_EDGE('',*,*,#9172,.F.);
#12245=ORIENTED_EDGE('',*,*,#9173,.T.);
#12246=ORIENTED_EDGE('',*,*,#9169,.T.);
#12247=ORIENTED_EDGE('',*,*,#9174,.T.);
#12248=ORIENTED_EDGE('',*,*,#9175,.F.);
#12249=ORIENTED_EDGE('',*,*,#9176,.T.);
#12250=ORIENTED_EDGE('',*,*,#9172,.T.);
#12251=ORIENTED_EDGE('',*,*,#9177,.T.);
#12252=ORIENTED_EDGE('',*,*,#9178,.F.);
#12253=ORIENTED_EDGE('',*,*,#9179,.T.);
#12254=ORIENTED_EDGE('',*,*,#9175,.T.);
#12255=ORIENTED_EDGE('',*,*,#9180,.T.);
#12256=ORIENTED_EDGE('',*,*,#9181,.F.);
#12257=ORIENTED_EDGE('',*,*,#9182,.T.);
#12258=ORIENTED_EDGE('',*,*,#9178,.T.);
#12259=ORIENTED_EDGE('',*,*,#9183,.T.);
#12260=ORIENTED_EDGE('',*,*,#9184,.F.);
#12261=ORIENTED_EDGE('',*,*,#9185,.T.);
#12262=ORIENTED_EDGE('',*,*,#9181,.T.);
#12263=ORIENTED_EDGE('',*,*,#9186,.T.);
#12264=ORIENTED_EDGE('',*,*,#9187,.F.);
#12265=ORIENTED_EDGE('',*,*,#9188,.T.);
#12266=ORIENTED_EDGE('',*,*,#9184,.T.);
#12267=ORIENTED_EDGE('',*,*,#9189,.T.);
#12268=ORIENTED_EDGE('',*,*,#9190,.F.);
#12269=ORIENTED_EDGE('',*,*,#9191,.T.);
#12270=ORIENTED_EDGE('',*,*,#9187,.T.);
#12271=ORIENTED_EDGE('',*,*,#9192,.T.);
#12272=ORIENTED_EDGE('',*,*,#9193,.F.);
#12273=ORIENTED_EDGE('',*,*,#9194,.T.);
#12274=ORIENTED_EDGE('',*,*,#9190,.T.);
#12275=ORIENTED_EDGE('',*,*,#9195,.T.);
#12276=ORIENTED_EDGE('',*,*,#9196,.F.);
#12277=ORIENTED_EDGE('',*,*,#9197,.T.);
#12278=ORIENTED_EDGE('',*,*,#9193,.T.);
#12279=ORIENTED_EDGE('',*,*,#9198,.T.);
#12280=ORIENTED_EDGE('',*,*,#9199,.F.);
#12281=ORIENTED_EDGE('',*,*,#9200,.T.);
#12282=ORIENTED_EDGE('',*,*,#9196,.T.);
#12283=ORIENTED_EDGE('',*,*,#9201,.T.);
#12284=ORIENTED_EDGE('',*,*,#9202,.F.);
#12285=ORIENTED_EDGE('',*,*,#9203,.T.);
#12286=ORIENTED_EDGE('',*,*,#9199,.T.);
#12287=ORIENTED_EDGE('',*,*,#9204,.T.);
#12288=ORIENTED_EDGE('',*,*,#9205,.F.);
#12289=ORIENTED_EDGE('',*,*,#9206,.T.);
#12290=ORIENTED_EDGE('',*,*,#9202,.T.);
#12291=ORIENTED_EDGE('',*,*,#9207,.T.);
#12292=ORIENTED_EDGE('',*,*,#9208,.F.);
#12293=ORIENTED_EDGE('',*,*,#9209,.T.);
#12294=ORIENTED_EDGE('',*,*,#9205,.T.);
#12295=ORIENTED_EDGE('',*,*,#9210,.T.);
#12296=ORIENTED_EDGE('',*,*,#9211,.F.);
#12297=ORIENTED_EDGE('',*,*,#9212,.T.);
#12298=ORIENTED_EDGE('',*,*,#9208,.T.);
#12299=ORIENTED_EDGE('',*,*,#9213,.T.);
#12300=ORIENTED_EDGE('',*,*,#9214,.F.);
#12301=ORIENTED_EDGE('',*,*,#9215,.T.);
#12302=ORIENTED_EDGE('',*,*,#9211,.T.);
#12303=ORIENTED_EDGE('',*,*,#9216,.T.);
#12304=ORIENTED_EDGE('',*,*,#9217,.F.);
#12305=ORIENTED_EDGE('',*,*,#9218,.T.);
#12306=ORIENTED_EDGE('',*,*,#9214,.T.);
#12307=ORIENTED_EDGE('',*,*,#9219,.T.);
#12308=ORIENTED_EDGE('',*,*,#9220,.F.);
#12309=ORIENTED_EDGE('',*,*,#9221,.T.);
#12310=ORIENTED_EDGE('',*,*,#9217,.T.);
#12311=ORIENTED_EDGE('',*,*,#9222,.T.);
#12312=ORIENTED_EDGE('',*,*,#9223,.F.);
#12313=ORIENTED_EDGE('',*,*,#9224,.T.);
#12314=ORIENTED_EDGE('',*,*,#9220,.T.);
#12315=ORIENTED_EDGE('',*,*,#9225,.T.);
#12316=ORIENTED_EDGE('',*,*,#9226,.F.);
#12317=ORIENTED_EDGE('',*,*,#9227,.T.);
#12318=ORIENTED_EDGE('',*,*,#9223,.T.);
#12319=ORIENTED_EDGE('',*,*,#9228,.T.);
#12320=ORIENTED_EDGE('',*,*,#9229,.F.);
#12321=ORIENTED_EDGE('',*,*,#9230,.T.);
#12322=ORIENTED_EDGE('',*,*,#9226,.T.);
#12323=ORIENTED_EDGE('',*,*,#9231,.T.);
#12324=ORIENTED_EDGE('',*,*,#9232,.F.);
#12325=ORIENTED_EDGE('',*,*,#9233,.T.);
#12326=ORIENTED_EDGE('',*,*,#9229,.T.);
#12327=ORIENTED_EDGE('',*,*,#9234,.T.);
#12328=ORIENTED_EDGE('',*,*,#9235,.F.);
#12329=ORIENTED_EDGE('',*,*,#9236,.T.);
#12330=ORIENTED_EDGE('',*,*,#9232,.T.);
#12331=ORIENTED_EDGE('',*,*,#9237,.T.);
#12332=ORIENTED_EDGE('',*,*,#9238,.F.);
#12333=ORIENTED_EDGE('',*,*,#9239,.T.);
#12334=ORIENTED_EDGE('',*,*,#9235,.T.);
#12335=ORIENTED_EDGE('',*,*,#9240,.T.);
#12336=ORIENTED_EDGE('',*,*,#9241,.F.);
#12337=ORIENTED_EDGE('',*,*,#9242,.T.);
#12338=ORIENTED_EDGE('',*,*,#9238,.T.);
#12339=ORIENTED_EDGE('',*,*,#9243,.T.);
#12340=ORIENTED_EDGE('',*,*,#9244,.F.);
#12341=ORIENTED_EDGE('',*,*,#9245,.T.);
#12342=ORIENTED_EDGE('',*,*,#9241,.T.);
#12343=ORIENTED_EDGE('',*,*,#9246,.T.);
#12344=ORIENTED_EDGE('',*,*,#9247,.F.);
#12345=ORIENTED_EDGE('',*,*,#9248,.T.);
#12346=ORIENTED_EDGE('',*,*,#9244,.T.);
#12347=ORIENTED_EDGE('',*,*,#9249,.T.);
#12348=ORIENTED_EDGE('',*,*,#9250,.F.);
#12349=ORIENTED_EDGE('',*,*,#9251,.T.);
#12350=ORIENTED_EDGE('',*,*,#9247,.T.);
#12351=ORIENTED_EDGE('',*,*,#9252,.T.);
#12352=ORIENTED_EDGE('',*,*,#9253,.F.);
#12353=ORIENTED_EDGE('',*,*,#9254,.T.);
#12354=ORIENTED_EDGE('',*,*,#9250,.T.);
#12355=ORIENTED_EDGE('',*,*,#9255,.T.);
#12356=ORIENTED_EDGE('',*,*,#9256,.F.);
#12357=ORIENTED_EDGE('',*,*,#9257,.T.);
#12358=ORIENTED_EDGE('',*,*,#9253,.T.);
#12359=ORIENTED_EDGE('',*,*,#9258,.T.);
#12360=ORIENTED_EDGE('',*,*,#9259,.F.);
#12361=ORIENTED_EDGE('',*,*,#9260,.T.);
#12362=ORIENTED_EDGE('',*,*,#9256,.T.);
#12363=ORIENTED_EDGE('',*,*,#9261,.T.);
#12364=ORIENTED_EDGE('',*,*,#9262,.F.);
#12365=ORIENTED_EDGE('',*,*,#9263,.T.);
#12366=ORIENTED_EDGE('',*,*,#9259,.T.);
#12367=ORIENTED_EDGE('',*,*,#9264,.T.);
#12368=ORIENTED_EDGE('',*,*,#9265,.F.);
#12369=ORIENTED_EDGE('',*,*,#9266,.T.);
#12370=ORIENTED_EDGE('',*,*,#9262,.T.);
#12371=ORIENTED_EDGE('',*,*,#9267,.T.);
#12372=ORIENTED_EDGE('',*,*,#9268,.F.);
#12373=ORIENTED_EDGE('',*,*,#9269,.T.);
#12374=ORIENTED_EDGE('',*,*,#9265,.T.);
#12375=ORIENTED_EDGE('',*,*,#9270,.T.);
#12376=ORIENTED_EDGE('',*,*,#9271,.F.);
#12377=ORIENTED_EDGE('',*,*,#9272,.T.);
#12378=ORIENTED_EDGE('',*,*,#9268,.T.);
#12379=ORIENTED_EDGE('',*,*,#9273,.T.);
#12380=ORIENTED_EDGE('',*,*,#9274,.F.);
#12381=ORIENTED_EDGE('',*,*,#9275,.T.);
#12382=ORIENTED_EDGE('',*,*,#9271,.T.);
#12383=ORIENTED_EDGE('',*,*,#9276,.T.);
#12384=ORIENTED_EDGE('',*,*,#9277,.F.);
#12385=ORIENTED_EDGE('',*,*,#9278,.T.);
#12386=ORIENTED_EDGE('',*,*,#9274,.T.);
#12387=ORIENTED_EDGE('',*,*,#9279,.T.);
#12388=ORIENTED_EDGE('',*,*,#9280,.F.);
#12389=ORIENTED_EDGE('',*,*,#9281,.T.);
#12390=ORIENTED_EDGE('',*,*,#9277,.T.);
#12391=ORIENTED_EDGE('',*,*,#9282,.T.);
#12392=ORIENTED_EDGE('',*,*,#9283,.F.);
#12393=ORIENTED_EDGE('',*,*,#9284,.T.);
#12394=ORIENTED_EDGE('',*,*,#9280,.T.);
#12395=ORIENTED_EDGE('',*,*,#9285,.T.);
#12396=ORIENTED_EDGE('',*,*,#9286,.F.);
#12397=ORIENTED_EDGE('',*,*,#9287,.T.);
#12398=ORIENTED_EDGE('',*,*,#9283,.T.);
#12399=ORIENTED_EDGE('',*,*,#9288,.T.);
#12400=ORIENTED_EDGE('',*,*,#9289,.F.);
#12401=ORIENTED_EDGE('',*,*,#9290,.T.);
#12402=ORIENTED_EDGE('',*,*,#9286,.T.);
#12403=ORIENTED_EDGE('',*,*,#9291,.T.);
#12404=ORIENTED_EDGE('',*,*,#9292,.F.);
#12405=ORIENTED_EDGE('',*,*,#9293,.T.);
#12406=ORIENTED_EDGE('',*,*,#9289,.T.);
#12407=ORIENTED_EDGE('',*,*,#9294,.T.);
#12408=ORIENTED_EDGE('',*,*,#9295,.F.);
#12409=ORIENTED_EDGE('',*,*,#9296,.T.);
#12410=ORIENTED_EDGE('',*,*,#9292,.T.);
#12411=ORIENTED_EDGE('',*,*,#9297,.T.);
#12412=ORIENTED_EDGE('',*,*,#9298,.F.);
#12413=ORIENTED_EDGE('',*,*,#9299,.T.);
#12414=ORIENTED_EDGE('',*,*,#9295,.T.);
#12415=ORIENTED_EDGE('',*,*,#9300,.T.);
#12416=ORIENTED_EDGE('',*,*,#9301,.F.);
#12417=ORIENTED_EDGE('',*,*,#9302,.T.);
#12418=ORIENTED_EDGE('',*,*,#9298,.T.);
#12419=ORIENTED_EDGE('',*,*,#9303,.T.);
#12420=ORIENTED_EDGE('',*,*,#9304,.F.);
#12421=ORIENTED_EDGE('',*,*,#9305,.T.);
#12422=ORIENTED_EDGE('',*,*,#9301,.T.);
#12423=ORIENTED_EDGE('',*,*,#9306,.T.);
#12424=ORIENTED_EDGE('',*,*,#9307,.F.);
#12425=ORIENTED_EDGE('',*,*,#9308,.T.);
#12426=ORIENTED_EDGE('',*,*,#9304,.T.);
#12427=ORIENTED_EDGE('',*,*,#9309,.T.);
#12428=ORIENTED_EDGE('',*,*,#9310,.F.);
#12429=ORIENTED_EDGE('',*,*,#9311,.T.);
#12430=ORIENTED_EDGE('',*,*,#9307,.T.);
#12431=ORIENTED_EDGE('',*,*,#9312,.T.);
#12432=ORIENTED_EDGE('',*,*,#9313,.F.);
#12433=ORIENTED_EDGE('',*,*,#9314,.T.);
#12434=ORIENTED_EDGE('',*,*,#9310,.T.);
#12435=ORIENTED_EDGE('',*,*,#9315,.T.);
#12436=ORIENTED_EDGE('',*,*,#9316,.F.);
#12437=ORIENTED_EDGE('',*,*,#9317,.T.);
#12438=ORIENTED_EDGE('',*,*,#9313,.T.);
#12439=ORIENTED_EDGE('',*,*,#9318,.T.);
#12440=ORIENTED_EDGE('',*,*,#9319,.F.);
#12441=ORIENTED_EDGE('',*,*,#9320,.T.);
#12442=ORIENTED_EDGE('',*,*,#9316,.T.);
#12443=ORIENTED_EDGE('',*,*,#9321,.T.);
#12444=ORIENTED_EDGE('',*,*,#9322,.F.);
#12445=ORIENTED_EDGE('',*,*,#9323,.T.);
#12446=ORIENTED_EDGE('',*,*,#9319,.T.);
#12447=ORIENTED_EDGE('',*,*,#9324,.T.);
#12448=ORIENTED_EDGE('',*,*,#9325,.F.);
#12449=ORIENTED_EDGE('',*,*,#9326,.T.);
#12450=ORIENTED_EDGE('',*,*,#9322,.T.);
#12451=ORIENTED_EDGE('',*,*,#9327,.T.);
#12452=ORIENTED_EDGE('',*,*,#9328,.F.);
#12453=ORIENTED_EDGE('',*,*,#9329,.T.);
#12454=ORIENTED_EDGE('',*,*,#9330,.T.);
#12455=ORIENTED_EDGE('',*,*,#9331,.T.);
#12456=ORIENTED_EDGE('',*,*,#9332,.T.);
#12457=ORIENTED_EDGE('',*,*,#9331,.F.);
#12458=ORIENTED_EDGE('',*,*,#9333,.T.);
#12459=ORIENTED_EDGE('',*,*,#9334,.T.);
#12460=ORIENTED_EDGE('',*,*,#9335,.F.);
#12461=ORIENTED_EDGE('',*,*,#9336,.T.);
#12462=ORIENTED_EDGE('',*,*,#9328,.T.);
#12463=ORIENTED_EDGE('',*,*,#9337,.T.);
#12464=ORIENTED_EDGE('',*,*,#9338,.F.);
#12465=ORIENTED_EDGE('',*,*,#9339,.T.);
#12466=ORIENTED_EDGE('',*,*,#9335,.T.);
#12467=ORIENTED_EDGE('',*,*,#9340,.T.);
#12468=ORIENTED_EDGE('',*,*,#9341,.F.);
#12469=ORIENTED_EDGE('',*,*,#9342,.T.);
#12470=ORIENTED_EDGE('',*,*,#9338,.T.);
#12471=ORIENTED_EDGE('',*,*,#9343,.T.);
#12472=ORIENTED_EDGE('',*,*,#9344,.F.);
#12473=ORIENTED_EDGE('',*,*,#9345,.T.);
#12474=ORIENTED_EDGE('',*,*,#9341,.T.);
#12475=ORIENTED_EDGE('',*,*,#9346,.T.);
#12476=ORIENTED_EDGE('',*,*,#9347,.F.);
#12477=ORIENTED_EDGE('',*,*,#9348,.T.);
#12478=ORIENTED_EDGE('',*,*,#9344,.T.);
#12479=ORIENTED_EDGE('',*,*,#9349,.T.);
#12480=ORIENTED_EDGE('',*,*,#9350,.F.);
#12481=ORIENTED_EDGE('',*,*,#9351,.T.);
#12482=ORIENTED_EDGE('',*,*,#9347,.T.);
#12483=ORIENTED_EDGE('',*,*,#9352,.T.);
#12484=ORIENTED_EDGE('',*,*,#9353,.F.);
#12485=ORIENTED_EDGE('',*,*,#9354,.T.);
#12486=ORIENTED_EDGE('',*,*,#9350,.T.);
#12487=ORIENTED_EDGE('',*,*,#9355,.T.);
#12488=ORIENTED_EDGE('',*,*,#9356,.F.);
#12489=ORIENTED_EDGE('',*,*,#9357,.T.);
#12490=ORIENTED_EDGE('',*,*,#9353,.T.);
#12491=ORIENTED_EDGE('',*,*,#9358,.T.);
#12492=ORIENTED_EDGE('',*,*,#9359,.F.);
#12493=ORIENTED_EDGE('',*,*,#9360,.T.);
#12494=ORIENTED_EDGE('',*,*,#9356,.T.);
#12495=ORIENTED_EDGE('',*,*,#9361,.T.);
#12496=ORIENTED_EDGE('',*,*,#9362,.F.);
#12497=ORIENTED_EDGE('',*,*,#9363,.T.);
#12498=ORIENTED_EDGE('',*,*,#9359,.T.);
#12499=ORIENTED_EDGE('',*,*,#9364,.T.);
#12500=ORIENTED_EDGE('',*,*,#9365,.F.);
#12501=ORIENTED_EDGE('',*,*,#9366,.T.);
#12502=ORIENTED_EDGE('',*,*,#9362,.T.);
#12503=ORIENTED_EDGE('',*,*,#9367,.T.);
#12504=ORIENTED_EDGE('',*,*,#9368,.F.);
#12505=ORIENTED_EDGE('',*,*,#9369,.T.);
#12506=ORIENTED_EDGE('',*,*,#9365,.T.);
#12507=ORIENTED_EDGE('',*,*,#9370,.T.);
#12508=ORIENTED_EDGE('',*,*,#9371,.F.);
#12509=ORIENTED_EDGE('',*,*,#9372,.T.);
#12510=ORIENTED_EDGE('',*,*,#9368,.T.);
#12511=ORIENTED_EDGE('',*,*,#9373,.T.);
#12512=ORIENTED_EDGE('',*,*,#9374,.F.);
#12513=ORIENTED_EDGE('',*,*,#9375,.T.);
#12514=ORIENTED_EDGE('',*,*,#9371,.T.);
#12515=ORIENTED_EDGE('',*,*,#9376,.T.);
#12516=ORIENTED_EDGE('',*,*,#9377,.F.);
#12517=ORIENTED_EDGE('',*,*,#9378,.T.);
#12518=ORIENTED_EDGE('',*,*,#9374,.T.);
#12519=ORIENTED_EDGE('',*,*,#9379,.T.);
#12520=ORIENTED_EDGE('',*,*,#9380,.F.);
#12521=ORIENTED_EDGE('',*,*,#9381,.T.);
#12522=ORIENTED_EDGE('',*,*,#9382,.F.);
#12523=ORIENTED_EDGE('',*,*,#9383,.F.);
#12524=ORIENTED_EDGE('',*,*,#9384,.F.);
#12525=ORIENTED_EDGE('',*,*,#9385,.T.);
#12526=ORIENTED_EDGE('',*,*,#9380,.T.);
#12527=ORIENTED_EDGE('',*,*,#9386,.F.);
#12528=ORIENTED_EDGE('',*,*,#9387,.F.);
#12529=ORIENTED_EDGE('',*,*,#9388,.T.);
#12530=ORIENTED_EDGE('',*,*,#9384,.T.);
#12531=ORIENTED_EDGE('',*,*,#9389,.F.);
#12532=ORIENTED_EDGE('',*,*,#9390,.F.);
#12533=ORIENTED_EDGE('',*,*,#9391,.T.);
#12534=ORIENTED_EDGE('',*,*,#9387,.T.);
#12535=ORIENTED_EDGE('',*,*,#9392,.F.);
#12536=ORIENTED_EDGE('',*,*,#9393,.F.);
#12537=ORIENTED_EDGE('',*,*,#9394,.T.);
#12538=ORIENTED_EDGE('',*,*,#9390,.T.);
#12539=ORIENTED_EDGE('',*,*,#9395,.F.);
#12540=ORIENTED_EDGE('',*,*,#9396,.F.);
#12541=ORIENTED_EDGE('',*,*,#9397,.T.);
#12542=ORIENTED_EDGE('',*,*,#9393,.T.);
#12543=ORIENTED_EDGE('',*,*,#9398,.F.);
#12544=ORIENTED_EDGE('',*,*,#9399,.F.);
#12545=ORIENTED_EDGE('',*,*,#9400,.T.);
#12546=ORIENTED_EDGE('',*,*,#9396,.T.);
#12547=ORIENTED_EDGE('',*,*,#9401,.F.);
#12548=ORIENTED_EDGE('',*,*,#9402,.F.);
#12549=ORIENTED_EDGE('',*,*,#9403,.T.);
#12550=ORIENTED_EDGE('',*,*,#9399,.T.);
#12551=ORIENTED_EDGE('',*,*,#9404,.F.);
#12552=ORIENTED_EDGE('',*,*,#9405,.F.);
#12553=ORIENTED_EDGE('',*,*,#9406,.T.);
#12554=ORIENTED_EDGE('',*,*,#9402,.T.);
#12555=ORIENTED_EDGE('',*,*,#9407,.F.);
#12556=ORIENTED_EDGE('',*,*,#9408,.F.);
#12557=ORIENTED_EDGE('',*,*,#9409,.T.);
#12558=ORIENTED_EDGE('',*,*,#9405,.T.);
#12559=ORIENTED_EDGE('',*,*,#9410,.F.);
#12560=ORIENTED_EDGE('',*,*,#9411,.F.);
#12561=ORIENTED_EDGE('',*,*,#9412,.T.);
#12562=ORIENTED_EDGE('',*,*,#9408,.T.);
#12563=ORIENTED_EDGE('',*,*,#9413,.F.);
#12564=ORIENTED_EDGE('',*,*,#9414,.F.);
#12565=ORIENTED_EDGE('',*,*,#9415,.T.);
#12566=ORIENTED_EDGE('',*,*,#9411,.T.);
#12567=ORIENTED_EDGE('',*,*,#9416,.F.);
#12568=ORIENTED_EDGE('',*,*,#9417,.F.);
#12569=ORIENTED_EDGE('',*,*,#9418,.T.);
#12570=ORIENTED_EDGE('',*,*,#9414,.T.);
#12571=ORIENTED_EDGE('',*,*,#9419,.F.);
#12572=ORIENTED_EDGE('',*,*,#9420,.F.);
#12573=ORIENTED_EDGE('',*,*,#9421,.T.);
#12574=ORIENTED_EDGE('',*,*,#9417,.T.);
#12575=ORIENTED_EDGE('',*,*,#9422,.F.);
#12576=ORIENTED_EDGE('',*,*,#9423,.F.);
#12577=ORIENTED_EDGE('',*,*,#9424,.T.);
#12578=ORIENTED_EDGE('',*,*,#9420,.T.);
#12579=ORIENTED_EDGE('',*,*,#9425,.F.);
#12580=ORIENTED_EDGE('',*,*,#9426,.F.);
#12581=ORIENTED_EDGE('',*,*,#9427,.T.);
#12582=ORIENTED_EDGE('',*,*,#9423,.T.);
#12583=ORIENTED_EDGE('',*,*,#9428,.F.);
#12584=ORIENTED_EDGE('',*,*,#9429,.F.);
#12585=ORIENTED_EDGE('',*,*,#9430,.T.);
#12586=ORIENTED_EDGE('',*,*,#9431,.F.);
#12587=ORIENTED_EDGE('',*,*,#9432,.F.);
#12588=ORIENTED_EDGE('',*,*,#9433,.T.);
#12589=ORIENTED_EDGE('',*,*,#9429,.T.);
#12590=ORIENTED_EDGE('',*,*,#9434,.F.);
#12591=ORIENTED_EDGE('',*,*,#9435,.F.);
#12592=ORIENTED_EDGE('',*,*,#9436,.F.);
#12593=ORIENTED_EDGE('',*,*,#9437,.T.);
#12594=ORIENTED_EDGE('',*,*,#9432,.T.);
#12595=ORIENTED_EDGE('',*,*,#9438,.F.);
#12596=ORIENTED_EDGE('',*,*,#9439,.F.);
#12597=ORIENTED_EDGE('',*,*,#9440,.T.);
#12598=ORIENTED_EDGE('',*,*,#9436,.T.);
#12599=ORIENTED_EDGE('',*,*,#9441,.F.);
#12600=ORIENTED_EDGE('',*,*,#9442,.F.);
#12601=ORIENTED_EDGE('',*,*,#9443,.T.);
#12602=ORIENTED_EDGE('',*,*,#9439,.T.);
#12603=ORIENTED_EDGE('',*,*,#9444,.F.);
#12604=ORIENTED_EDGE('',*,*,#9445,.F.);
#12605=ORIENTED_EDGE('',*,*,#9446,.T.);
#12606=ORIENTED_EDGE('',*,*,#9442,.T.);
#12607=ORIENTED_EDGE('',*,*,#9447,.F.);
#12608=ORIENTED_EDGE('',*,*,#9448,.F.);
#12609=ORIENTED_EDGE('',*,*,#9449,.T.);
#12610=ORIENTED_EDGE('',*,*,#9445,.T.);
#12611=ORIENTED_EDGE('',*,*,#9450,.F.);
#12612=ORIENTED_EDGE('',*,*,#9451,.F.);
#12613=ORIENTED_EDGE('',*,*,#9452,.T.);
#12614=ORIENTED_EDGE('',*,*,#9448,.T.);
#12615=ORIENTED_EDGE('',*,*,#9453,.F.);
#12616=ORIENTED_EDGE('',*,*,#9454,.F.);
#12617=ORIENTED_EDGE('',*,*,#9455,.T.);
#12618=ORIENTED_EDGE('',*,*,#9451,.T.);
#12619=ORIENTED_EDGE('',*,*,#9456,.F.);
#12620=ORIENTED_EDGE('',*,*,#9457,.F.);
#12621=ORIENTED_EDGE('',*,*,#9458,.T.);
#12622=ORIENTED_EDGE('',*,*,#9454,.T.);
#12623=ORIENTED_EDGE('',*,*,#9459,.F.);
#12624=ORIENTED_EDGE('',*,*,#9460,.F.);
#12625=ORIENTED_EDGE('',*,*,#9461,.T.);
#12626=ORIENTED_EDGE('',*,*,#9457,.T.);
#12627=ORIENTED_EDGE('',*,*,#9462,.F.);
#12628=ORIENTED_EDGE('',*,*,#9463,.F.);
#12629=ORIENTED_EDGE('',*,*,#9464,.T.);
#12630=ORIENTED_EDGE('',*,*,#9460,.T.);
#12631=ORIENTED_EDGE('',*,*,#9465,.F.);
#12632=ORIENTED_EDGE('',*,*,#9466,.F.);
#12633=ORIENTED_EDGE('',*,*,#9467,.T.);
#12634=ORIENTED_EDGE('',*,*,#9463,.T.);
#12635=ORIENTED_EDGE('',*,*,#9468,.F.);
#12636=ORIENTED_EDGE('',*,*,#9469,.F.);
#12637=ORIENTED_EDGE('',*,*,#9470,.T.);
#12638=ORIENTED_EDGE('',*,*,#9466,.T.);
#12639=ORIENTED_EDGE('',*,*,#9471,.F.);
#12640=ORIENTED_EDGE('',*,*,#9472,.F.);
#12641=ORIENTED_EDGE('',*,*,#9473,.T.);
#12642=ORIENTED_EDGE('',*,*,#9469,.T.);
#12643=ORIENTED_EDGE('',*,*,#9474,.F.);
#12644=ORIENTED_EDGE('',*,*,#9475,.F.);
#12645=ORIENTED_EDGE('',*,*,#9476,.T.);
#12646=ORIENTED_EDGE('',*,*,#9472,.T.);
#12647=ORIENTED_EDGE('',*,*,#9477,.F.);
#12648=ORIENTED_EDGE('',*,*,#9478,.F.);
#12649=ORIENTED_EDGE('',*,*,#9479,.T.);
#12650=ORIENTED_EDGE('',*,*,#9475,.T.);
#12651=ORIENTED_EDGE('',*,*,#9480,.F.);
#12652=ORIENTED_EDGE('',*,*,#9481,.F.);
#12653=ORIENTED_EDGE('',*,*,#9482,.T.);
#12654=ORIENTED_EDGE('',*,*,#9478,.T.);
#12655=ORIENTED_EDGE('',*,*,#9483,.F.);
#12656=ORIENTED_EDGE('',*,*,#9484,.F.);
#12657=ORIENTED_EDGE('',*,*,#9485,.T.);
#12658=ORIENTED_EDGE('',*,*,#9481,.T.);
#12659=ORIENTED_EDGE('',*,*,#9486,.F.);
#12660=ORIENTED_EDGE('',*,*,#9487,.F.);
#12661=ORIENTED_EDGE('',*,*,#9488,.T.);
#12662=ORIENTED_EDGE('',*,*,#9484,.T.);
#12663=ORIENTED_EDGE('',*,*,#9489,.F.);
#12664=ORIENTED_EDGE('',*,*,#9490,.F.);
#12665=ORIENTED_EDGE('',*,*,#9491,.T.);
#12666=ORIENTED_EDGE('',*,*,#9487,.T.);
#12667=ORIENTED_EDGE('',*,*,#9492,.F.);
#12668=ORIENTED_EDGE('',*,*,#9493,.F.);
#12669=ORIENTED_EDGE('',*,*,#9494,.T.);
#12670=ORIENTED_EDGE('',*,*,#9490,.T.);
#12671=ORIENTED_EDGE('',*,*,#9495,.F.);
#12672=ORIENTED_EDGE('',*,*,#9496,.F.);
#12673=ORIENTED_EDGE('',*,*,#9497,.T.);
#12674=ORIENTED_EDGE('',*,*,#9493,.T.);
#12675=ORIENTED_EDGE('',*,*,#9498,.F.);
#12676=ORIENTED_EDGE('',*,*,#9499,.F.);
#12677=ORIENTED_EDGE('',*,*,#9500,.T.);
#12678=ORIENTED_EDGE('',*,*,#9496,.T.);
#12679=ORIENTED_EDGE('',*,*,#9501,.F.);
#12680=ORIENTED_EDGE('',*,*,#9502,.F.);
#12681=ORIENTED_EDGE('',*,*,#9503,.T.);
#12682=ORIENTED_EDGE('',*,*,#9499,.T.);
#12683=ORIENTED_EDGE('',*,*,#9504,.F.);
#12684=ORIENTED_EDGE('',*,*,#9505,.F.);
#12685=ORIENTED_EDGE('',*,*,#9506,.T.);
#12686=ORIENTED_EDGE('',*,*,#9502,.T.);
#12687=ORIENTED_EDGE('',*,*,#9507,.F.);
#12688=ORIENTED_EDGE('',*,*,#9508,.F.);
#12689=ORIENTED_EDGE('',*,*,#9509,.T.);
#12690=ORIENTED_EDGE('',*,*,#9505,.T.);
#12691=ORIENTED_EDGE('',*,*,#9510,.F.);
#12692=ORIENTED_EDGE('',*,*,#9511,.F.);
#12693=ORIENTED_EDGE('',*,*,#9512,.T.);
#12694=ORIENTED_EDGE('',*,*,#9508,.T.);
#12695=ORIENTED_EDGE('',*,*,#9513,.F.);
#12696=ORIENTED_EDGE('',*,*,#9514,.F.);
#12697=ORIENTED_EDGE('',*,*,#9515,.T.);
#12698=ORIENTED_EDGE('',*,*,#9511,.T.);
#12699=ORIENTED_EDGE('',*,*,#9516,.F.);
#12700=ORIENTED_EDGE('',*,*,#9517,.F.);
#12701=ORIENTED_EDGE('',*,*,#9518,.T.);
#12702=ORIENTED_EDGE('',*,*,#9514,.T.);
#12703=ORIENTED_EDGE('',*,*,#9519,.F.);
#12704=ORIENTED_EDGE('',*,*,#9520,.F.);
#12705=ORIENTED_EDGE('',*,*,#9521,.T.);
#12706=ORIENTED_EDGE('',*,*,#9517,.T.);
#12707=ORIENTED_EDGE('',*,*,#9522,.F.);
#12708=ORIENTED_EDGE('',*,*,#9523,.F.);
#12709=ORIENTED_EDGE('',*,*,#9524,.T.);
#12710=ORIENTED_EDGE('',*,*,#9520,.T.);
#12711=ORIENTED_EDGE('',*,*,#9525,.F.);
#12712=ORIENTED_EDGE('',*,*,#9526,.F.);
#12713=ORIENTED_EDGE('',*,*,#9527,.T.);
#12714=ORIENTED_EDGE('',*,*,#9523,.T.);
#12715=ORIENTED_EDGE('',*,*,#9528,.F.);
#12716=ORIENTED_EDGE('',*,*,#9529,.F.);
#12717=ORIENTED_EDGE('',*,*,#9530,.T.);
#12718=ORIENTED_EDGE('',*,*,#9526,.T.);
#12719=ORIENTED_EDGE('',*,*,#9531,.F.);
#12720=ORIENTED_EDGE('',*,*,#9532,.F.);
#12721=ORIENTED_EDGE('',*,*,#9533,.T.);
#12722=ORIENTED_EDGE('',*,*,#9529,.T.);
#12723=ORIENTED_EDGE('',*,*,#9534,.F.);
#12724=ORIENTED_EDGE('',*,*,#9535,.F.);
#12725=ORIENTED_EDGE('',*,*,#9536,.T.);
#12726=ORIENTED_EDGE('',*,*,#9532,.T.);
#12727=ORIENTED_EDGE('',*,*,#9537,.F.);
#12728=ORIENTED_EDGE('',*,*,#9538,.F.);
#12729=ORIENTED_EDGE('',*,*,#9539,.T.);
#12730=ORIENTED_EDGE('',*,*,#9535,.T.);
#12731=ORIENTED_EDGE('',*,*,#9540,.F.);
#12732=ORIENTED_EDGE('',*,*,#9541,.F.);
#12733=ORIENTED_EDGE('',*,*,#9542,.T.);
#12734=ORIENTED_EDGE('',*,*,#9538,.T.);
#12735=ORIENTED_EDGE('',*,*,#9543,.F.);
#12736=ORIENTED_EDGE('',*,*,#9544,.F.);
#12737=ORIENTED_EDGE('',*,*,#9545,.T.);
#12738=ORIENTED_EDGE('',*,*,#9541,.T.);
#12739=ORIENTED_EDGE('',*,*,#9546,.F.);
#12740=ORIENTED_EDGE('',*,*,#9547,.F.);
#12741=ORIENTED_EDGE('',*,*,#9548,.T.);
#12742=ORIENTED_EDGE('',*,*,#9544,.T.);
#12743=ORIENTED_EDGE('',*,*,#9549,.F.);
#12744=ORIENTED_EDGE('',*,*,#9550,.F.);
#12745=ORIENTED_EDGE('',*,*,#9551,.T.);
#12746=ORIENTED_EDGE('',*,*,#9547,.T.);
#12747=ORIENTED_EDGE('',*,*,#9552,.F.);
#12748=ORIENTED_EDGE('',*,*,#9553,.F.);
#12749=ORIENTED_EDGE('',*,*,#9554,.T.);
#12750=ORIENTED_EDGE('',*,*,#9550,.T.);
#12751=ORIENTED_EDGE('',*,*,#9555,.F.);
#12752=ORIENTED_EDGE('',*,*,#9556,.F.);
#12753=ORIENTED_EDGE('',*,*,#9557,.T.);
#12754=ORIENTED_EDGE('',*,*,#9553,.T.);
#12755=ORIENTED_EDGE('',*,*,#9558,.F.);
#12756=ORIENTED_EDGE('',*,*,#9559,.F.);
#12757=ORIENTED_EDGE('',*,*,#9560,.T.);
#12758=ORIENTED_EDGE('',*,*,#9556,.T.);
#12759=ORIENTED_EDGE('',*,*,#9561,.F.);
#12760=ORIENTED_EDGE('',*,*,#9562,.F.);
#12761=ORIENTED_EDGE('',*,*,#9563,.T.);
#12762=ORIENTED_EDGE('',*,*,#9559,.T.);
#12763=ORIENTED_EDGE('',*,*,#9564,.F.);
#12764=ORIENTED_EDGE('',*,*,#9565,.F.);
#12765=ORIENTED_EDGE('',*,*,#9566,.T.);
#12766=ORIENTED_EDGE('',*,*,#9562,.T.);
#12767=ORIENTED_EDGE('',*,*,#9567,.F.);
#12768=ORIENTED_EDGE('',*,*,#9568,.F.);
#12769=ORIENTED_EDGE('',*,*,#9569,.T.);
#12770=ORIENTED_EDGE('',*,*,#9565,.T.);
#12771=ORIENTED_EDGE('',*,*,#9570,.F.);
#12772=ORIENTED_EDGE('',*,*,#9571,.F.);
#12773=ORIENTED_EDGE('',*,*,#9572,.T.);
#12774=ORIENTED_EDGE('',*,*,#9568,.T.);
#12775=ORIENTED_EDGE('',*,*,#9573,.F.);
#12776=ORIENTED_EDGE('',*,*,#9574,.F.);
#12777=ORIENTED_EDGE('',*,*,#9575,.T.);
#12778=ORIENTED_EDGE('',*,*,#9571,.T.);
#12779=ORIENTED_EDGE('',*,*,#9576,.F.);
#12780=ORIENTED_EDGE('',*,*,#9577,.F.);
#12781=ORIENTED_EDGE('',*,*,#9578,.T.);
#12782=ORIENTED_EDGE('',*,*,#9574,.T.);
#12783=ORIENTED_EDGE('',*,*,#9579,.F.);
#12784=ORIENTED_EDGE('',*,*,#9580,.F.);
#12785=ORIENTED_EDGE('',*,*,#9581,.T.);
#12786=ORIENTED_EDGE('',*,*,#9577,.T.);
#12787=ORIENTED_EDGE('',*,*,#9582,.F.);
#12788=ORIENTED_EDGE('',*,*,#9583,.F.);
#12789=ORIENTED_EDGE('',*,*,#9584,.T.);
#12790=ORIENTED_EDGE('',*,*,#9580,.T.);
#12791=ORIENTED_EDGE('',*,*,#9585,.F.);
#12792=ORIENTED_EDGE('',*,*,#9586,.F.);
#12793=ORIENTED_EDGE('',*,*,#9587,.T.);
#12794=ORIENTED_EDGE('',*,*,#9583,.T.);
#12795=ORIENTED_EDGE('',*,*,#9588,.F.);
#12796=ORIENTED_EDGE('',*,*,#9589,.F.);
#12797=ORIENTED_EDGE('',*,*,#9590,.T.);
#12798=ORIENTED_EDGE('',*,*,#9586,.T.);
#12799=ORIENTED_EDGE('',*,*,#9591,.F.);
#12800=ORIENTED_EDGE('',*,*,#9592,.F.);
#12801=ORIENTED_EDGE('',*,*,#9593,.T.);
#12802=ORIENTED_EDGE('',*,*,#9589,.T.);
#12803=ORIENTED_EDGE('',*,*,#9594,.F.);
#12804=ORIENTED_EDGE('',*,*,#9595,.F.);
#12805=ORIENTED_EDGE('',*,*,#9596,.T.);
#12806=ORIENTED_EDGE('',*,*,#9592,.T.);
#12807=ORIENTED_EDGE('',*,*,#9597,.F.);
#12808=ORIENTED_EDGE('',*,*,#9598,.F.);
#12809=ORIENTED_EDGE('',*,*,#9599,.T.);
#12810=ORIENTED_EDGE('',*,*,#9595,.T.);
#12811=ORIENTED_EDGE('',*,*,#9600,.F.);
#12812=ORIENTED_EDGE('',*,*,#9601,.F.);
#12813=ORIENTED_EDGE('',*,*,#9602,.T.);
#12814=ORIENTED_EDGE('',*,*,#9598,.T.);
#12815=ORIENTED_EDGE('',*,*,#9603,.F.);
#12816=ORIENTED_EDGE('',*,*,#9604,.F.);
#12817=ORIENTED_EDGE('',*,*,#9605,.T.);
#12818=ORIENTED_EDGE('',*,*,#9601,.T.);
#12819=ORIENTED_EDGE('',*,*,#9606,.F.);
#12820=ORIENTED_EDGE('',*,*,#9607,.F.);
#12821=ORIENTED_EDGE('',*,*,#9608,.T.);
#12822=ORIENTED_EDGE('',*,*,#9604,.T.);
#12823=ORIENTED_EDGE('',*,*,#9609,.F.);
#12824=ORIENTED_EDGE('',*,*,#9610,.F.);
#12825=ORIENTED_EDGE('',*,*,#9611,.T.);
#12826=ORIENTED_EDGE('',*,*,#9607,.T.);
#12827=ORIENTED_EDGE('',*,*,#9612,.F.);
#12828=ORIENTED_EDGE('',*,*,#9613,.F.);
#12829=ORIENTED_EDGE('',*,*,#9614,.T.);
#12830=ORIENTED_EDGE('',*,*,#9610,.T.);
#12831=ORIENTED_EDGE('',*,*,#9615,.F.);
#12832=ORIENTED_EDGE('',*,*,#9616,.F.);
#12833=ORIENTED_EDGE('',*,*,#9617,.T.);
#12834=ORIENTED_EDGE('',*,*,#9613,.T.);
#12835=ORIENTED_EDGE('',*,*,#9618,.F.);
#12836=ORIENTED_EDGE('',*,*,#9143,.F.);
#12837=ORIENTED_EDGE('',*,*,#9619,.F.);
#12838=ORIENTED_EDGE('',*,*,#9137,.F.);
#12839=ORIENTED_EDGE('',*,*,#9620,.F.);
#12840=ORIENTED_EDGE('',*,*,#9144,.F.);
#12841=ORIENTED_EDGE('',*,*,#9620,.T.);
#12842=ORIENTED_EDGE('',*,*,#9136,.F.);
#12843=ORIENTED_EDGE('',*,*,#9133,.F.);
#12844=ORIENTED_EDGE('',*,*,#9621,.T.);
#12845=ORIENTED_EDGE('',*,*,#9141,.F.);
#12846=ORIENTED_EDGE('',*,*,#9621,.F.);
#12847=ORIENTED_EDGE('',*,*,#9132,.F.);
#12848=ORIENTED_EDGE('',*,*,#9622,.F.);
#12849=ORIENTED_EDGE('',*,*,#9142,.F.);
#12850=ORIENTED_EDGE('',*,*,#9622,.T.);
#12851=ORIENTED_EDGE('',*,*,#9131,.F.);
#12852=ORIENTED_EDGE('',*,*,#9138,.F.);
#12853=ORIENTED_EDGE('',*,*,#9619,.T.);
#12854=ORIENTED_EDGE('',*,*,#9434,.T.);
#12855=ORIENTED_EDGE('',*,*,#9431,.T.);
#12856=ORIENTED_EDGE('',*,*,#9623,.T.);
#12857=ORIENTED_EDGE('',*,*,#9624,.F.);
#12858=ORIENTED_EDGE('',*,*,#9625,.F.);
#12859=ORIENTED_EDGE('',*,*,#9626,.T.);
#12860=ORIENTED_EDGE('',*,*,#9626,.F.);
#12861=ORIENTED_EDGE('',*,*,#9627,.F.);
#12862=ORIENTED_EDGE('',*,*,#9327,.F.);
#12863=ORIENTED_EDGE('',*,*,#9324,.F.);
#12864=ORIENTED_EDGE('',*,*,#9321,.F.);
#12865=ORIENTED_EDGE('',*,*,#9318,.F.);
#12866=ORIENTED_EDGE('',*,*,#9315,.F.);
#12867=ORIENTED_EDGE('',*,*,#9312,.F.);
#12868=ORIENTED_EDGE('',*,*,#9309,.F.);
#12869=ORIENTED_EDGE('',*,*,#9306,.F.);
#12870=ORIENTED_EDGE('',*,*,#9303,.F.);
#12871=ORIENTED_EDGE('',*,*,#9300,.F.);
#12872=ORIENTED_EDGE('',*,*,#9297,.F.);
#12873=ORIENTED_EDGE('',*,*,#9294,.F.);
#12874=ORIENTED_EDGE('',*,*,#9291,.F.);
#12875=ORIENTED_EDGE('',*,*,#9288,.F.);
#12876=ORIENTED_EDGE('',*,*,#9285,.F.);
#12877=ORIENTED_EDGE('',*,*,#9282,.F.);
#12878=ORIENTED_EDGE('',*,*,#9279,.F.);
#12879=ORIENTED_EDGE('',*,*,#9276,.F.);
#12880=ORIENTED_EDGE('',*,*,#9273,.F.);
#12881=ORIENTED_EDGE('',*,*,#9270,.F.);
#12882=ORIENTED_EDGE('',*,*,#9267,.F.);
#12883=ORIENTED_EDGE('',*,*,#9264,.F.);
#12884=ORIENTED_EDGE('',*,*,#9261,.F.);
#12885=ORIENTED_EDGE('',*,*,#9258,.F.);
#12886=ORIENTED_EDGE('',*,*,#9255,.F.);
#12887=ORIENTED_EDGE('',*,*,#9252,.F.);
#12888=ORIENTED_EDGE('',*,*,#9249,.F.);
#12889=ORIENTED_EDGE('',*,*,#9246,.F.);
#12890=ORIENTED_EDGE('',*,*,#9243,.F.);
#12891=ORIENTED_EDGE('',*,*,#9240,.F.);
#12892=ORIENTED_EDGE('',*,*,#9237,.F.);
#12893=ORIENTED_EDGE('',*,*,#9234,.F.);
#12894=ORIENTED_EDGE('',*,*,#9231,.F.);
#12895=ORIENTED_EDGE('',*,*,#9228,.F.);
#12896=ORIENTED_EDGE('',*,*,#9225,.F.);
#12897=ORIENTED_EDGE('',*,*,#9222,.F.);
#12898=ORIENTED_EDGE('',*,*,#9219,.F.);
#12899=ORIENTED_EDGE('',*,*,#9216,.F.);
#12900=ORIENTED_EDGE('',*,*,#9213,.F.);
#12901=ORIENTED_EDGE('',*,*,#9210,.F.);
#12902=ORIENTED_EDGE('',*,*,#9207,.F.);
#12903=ORIENTED_EDGE('',*,*,#9204,.F.);
#12904=ORIENTED_EDGE('',*,*,#9201,.F.);
#12905=ORIENTED_EDGE('',*,*,#9198,.F.);
#12906=ORIENTED_EDGE('',*,*,#9195,.F.);
#12907=ORIENTED_EDGE('',*,*,#9192,.F.);
#12908=ORIENTED_EDGE('',*,*,#9189,.F.);
#12909=ORIENTED_EDGE('',*,*,#9186,.F.);
#12910=ORIENTED_EDGE('',*,*,#9183,.F.);
#12911=ORIENTED_EDGE('',*,*,#9180,.F.);
#12912=ORIENTED_EDGE('',*,*,#9177,.F.);
#12913=ORIENTED_EDGE('',*,*,#9174,.F.);
#12914=ORIENTED_EDGE('',*,*,#9171,.F.);
#12915=ORIENTED_EDGE('',*,*,#9168,.F.);
#12916=ORIENTED_EDGE('',*,*,#9165,.F.);
#12917=ORIENTED_EDGE('',*,*,#9162,.F.);
#12918=ORIENTED_EDGE('',*,*,#9159,.F.);
#12919=ORIENTED_EDGE('',*,*,#9156,.F.);
#12920=ORIENTED_EDGE('',*,*,#9153,.F.);
#12921=ORIENTED_EDGE('',*,*,#9150,.F.);
#12922=ORIENTED_EDGE('',*,*,#9147,.F.);
#12923=ORIENTED_EDGE('',*,*,#9140,.F.);
#12924=ORIENTED_EDGE('',*,*,#9628,.F.);
#12925=ORIENTED_EDGE('',*,*,#9629,.T.);
#12926=ORIENTED_EDGE('',*,*,#9618,.T.);
#12927=ORIENTED_EDGE('',*,*,#9615,.T.);
#12928=ORIENTED_EDGE('',*,*,#9612,.T.);
#12929=ORIENTED_EDGE('',*,*,#9609,.T.);
#12930=ORIENTED_EDGE('',*,*,#9606,.T.);
#12931=ORIENTED_EDGE('',*,*,#9603,.T.);
#12932=ORIENTED_EDGE('',*,*,#9600,.T.);
#12933=ORIENTED_EDGE('',*,*,#9597,.T.);
#12934=ORIENTED_EDGE('',*,*,#9594,.T.);
#12935=ORIENTED_EDGE('',*,*,#9591,.T.);
#12936=ORIENTED_EDGE('',*,*,#9588,.T.);
#12937=ORIENTED_EDGE('',*,*,#9585,.T.);
#12938=ORIENTED_EDGE('',*,*,#9582,.T.);
#12939=ORIENTED_EDGE('',*,*,#9579,.T.);
#12940=ORIENTED_EDGE('',*,*,#9576,.T.);
#12941=ORIENTED_EDGE('',*,*,#9573,.T.);
#12942=ORIENTED_EDGE('',*,*,#9570,.T.);
#12943=ORIENTED_EDGE('',*,*,#9567,.T.);
#12944=ORIENTED_EDGE('',*,*,#9564,.T.);
#12945=ORIENTED_EDGE('',*,*,#9561,.T.);
#12946=ORIENTED_EDGE('',*,*,#9558,.T.);
#12947=ORIENTED_EDGE('',*,*,#9555,.T.);
#12948=ORIENTED_EDGE('',*,*,#9552,.T.);
#12949=ORIENTED_EDGE('',*,*,#9549,.T.);
#12950=ORIENTED_EDGE('',*,*,#9546,.T.);
#12951=ORIENTED_EDGE('',*,*,#9543,.T.);
#12952=ORIENTED_EDGE('',*,*,#9540,.T.);
#12953=ORIENTED_EDGE('',*,*,#9537,.T.);
#12954=ORIENTED_EDGE('',*,*,#9534,.T.);
#12955=ORIENTED_EDGE('',*,*,#9531,.T.);
#12956=ORIENTED_EDGE('',*,*,#9528,.T.);
#12957=ORIENTED_EDGE('',*,*,#9525,.T.);
#12958=ORIENTED_EDGE('',*,*,#9522,.T.);
#12959=ORIENTED_EDGE('',*,*,#9519,.T.);
#12960=ORIENTED_EDGE('',*,*,#9516,.T.);
#12961=ORIENTED_EDGE('',*,*,#9513,.T.);
#12962=ORIENTED_EDGE('',*,*,#9510,.T.);
#12963=ORIENTED_EDGE('',*,*,#9507,.T.);
#12964=ORIENTED_EDGE('',*,*,#9504,.T.);
#12965=ORIENTED_EDGE('',*,*,#9501,.T.);
#12966=ORIENTED_EDGE('',*,*,#9498,.T.);
#12967=ORIENTED_EDGE('',*,*,#9495,.T.);
#12968=ORIENTED_EDGE('',*,*,#9492,.T.);
#12969=ORIENTED_EDGE('',*,*,#9489,.T.);
#12970=ORIENTED_EDGE('',*,*,#9486,.T.);
#12971=ORIENTED_EDGE('',*,*,#9483,.T.);
#12972=ORIENTED_EDGE('',*,*,#9480,.T.);
#12973=ORIENTED_EDGE('',*,*,#9477,.T.);
#12974=ORIENTED_EDGE('',*,*,#9474,.T.);
#12975=ORIENTED_EDGE('',*,*,#9471,.T.);
#12976=ORIENTED_EDGE('',*,*,#9468,.T.);
#12977=ORIENTED_EDGE('',*,*,#9465,.T.);
#12978=ORIENTED_EDGE('',*,*,#9462,.T.);
#12979=ORIENTED_EDGE('',*,*,#9459,.T.);
#12980=ORIENTED_EDGE('',*,*,#9456,.T.);
#12981=ORIENTED_EDGE('',*,*,#9453,.T.);
#12982=ORIENTED_EDGE('',*,*,#9450,.T.);
#12983=ORIENTED_EDGE('',*,*,#9447,.T.);
#12984=ORIENTED_EDGE('',*,*,#9444,.T.);
#12985=ORIENTED_EDGE('',*,*,#9441,.T.);
#12986=ORIENTED_EDGE('',*,*,#9438,.T.);
#12987=ORIENTED_EDGE('',*,*,#9435,.T.);
#12988=ORIENTED_EDGE('',*,*,#9129,.F.);
#12989=ORIENTED_EDGE('',*,*,#9630,.T.);
#12990=ORIENTED_EDGE('',*,*,#9631,.T.);
#12991=ORIENTED_EDGE('',*,*,#9628,.T.);
#12992=ORIENTED_EDGE('',*,*,#9139,.F.);
#12993=ORIENTED_EDGE('',*,*,#9616,.T.);
#12994=ORIENTED_EDGE('',*,*,#9629,.F.);
#12995=ORIENTED_EDGE('',*,*,#9631,.F.);
#12996=ORIENTED_EDGE('',*,*,#9632,.T.);
#12997=ORIENTED_EDGE('',*,*,#9623,.F.);
#12998=ORIENTED_EDGE('',*,*,#9430,.F.);
#12999=ORIENTED_EDGE('',*,*,#9433,.F.);
#13000=ORIENTED_EDGE('',*,*,#9437,.F.);
#13001=ORIENTED_EDGE('',*,*,#9440,.F.);
#13002=ORIENTED_EDGE('',*,*,#9443,.F.);
#13003=ORIENTED_EDGE('',*,*,#9446,.F.);
#13004=ORIENTED_EDGE('',*,*,#9449,.F.);
#13005=ORIENTED_EDGE('',*,*,#9452,.F.);
#13006=ORIENTED_EDGE('',*,*,#9455,.F.);
#13007=ORIENTED_EDGE('',*,*,#9458,.F.);
#13008=ORIENTED_EDGE('',*,*,#9461,.F.);
#13009=ORIENTED_EDGE('',*,*,#9464,.F.);
#13010=ORIENTED_EDGE('',*,*,#9467,.F.);
#13011=ORIENTED_EDGE('',*,*,#9470,.F.);
#13012=ORIENTED_EDGE('',*,*,#9473,.F.);
#13013=ORIENTED_EDGE('',*,*,#9476,.F.);
#13014=ORIENTED_EDGE('',*,*,#9479,.F.);
#13015=ORIENTED_EDGE('',*,*,#9482,.F.);
#13016=ORIENTED_EDGE('',*,*,#9485,.F.);
#13017=ORIENTED_EDGE('',*,*,#9488,.F.);
#13018=ORIENTED_EDGE('',*,*,#9491,.F.);
#13019=ORIENTED_EDGE('',*,*,#9494,.F.);
#13020=ORIENTED_EDGE('',*,*,#9497,.F.);
#13021=ORIENTED_EDGE('',*,*,#9500,.F.);
#13022=ORIENTED_EDGE('',*,*,#9503,.F.);
#13023=ORIENTED_EDGE('',*,*,#9506,.F.);
#13024=ORIENTED_EDGE('',*,*,#9509,.F.);
#13025=ORIENTED_EDGE('',*,*,#9512,.F.);
#13026=ORIENTED_EDGE('',*,*,#9515,.F.);
#13027=ORIENTED_EDGE('',*,*,#9518,.F.);
#13028=ORIENTED_EDGE('',*,*,#9521,.F.);
#13029=ORIENTED_EDGE('',*,*,#9524,.F.);
#13030=ORIENTED_EDGE('',*,*,#9527,.F.);
#13031=ORIENTED_EDGE('',*,*,#9530,.F.);
#13032=ORIENTED_EDGE('',*,*,#9533,.F.);
#13033=ORIENTED_EDGE('',*,*,#9536,.F.);
#13034=ORIENTED_EDGE('',*,*,#9539,.F.);
#13035=ORIENTED_EDGE('',*,*,#9542,.F.);
#13036=ORIENTED_EDGE('',*,*,#9545,.F.);
#13037=ORIENTED_EDGE('',*,*,#9548,.F.);
#13038=ORIENTED_EDGE('',*,*,#9551,.F.);
#13039=ORIENTED_EDGE('',*,*,#9554,.F.);
#13040=ORIENTED_EDGE('',*,*,#9557,.F.);
#13041=ORIENTED_EDGE('',*,*,#9560,.F.);
#13042=ORIENTED_EDGE('',*,*,#9563,.F.);
#13043=ORIENTED_EDGE('',*,*,#9566,.F.);
#13044=ORIENTED_EDGE('',*,*,#9569,.F.);
#13045=ORIENTED_EDGE('',*,*,#9572,.F.);
#13046=ORIENTED_EDGE('',*,*,#9575,.F.);
#13047=ORIENTED_EDGE('',*,*,#9578,.F.);
#13048=ORIENTED_EDGE('',*,*,#9581,.F.);
#13049=ORIENTED_EDGE('',*,*,#9584,.F.);
#13050=ORIENTED_EDGE('',*,*,#9587,.F.);
#13051=ORIENTED_EDGE('',*,*,#9590,.F.);
#13052=ORIENTED_EDGE('',*,*,#9593,.F.);
#13053=ORIENTED_EDGE('',*,*,#9596,.F.);
#13054=ORIENTED_EDGE('',*,*,#9599,.F.);
#13055=ORIENTED_EDGE('',*,*,#9602,.F.);
#13056=ORIENTED_EDGE('',*,*,#9605,.F.);
#13057=ORIENTED_EDGE('',*,*,#9608,.F.);
#13058=ORIENTED_EDGE('',*,*,#9611,.F.);
#13059=ORIENTED_EDGE('',*,*,#9614,.F.);
#13060=ORIENTED_EDGE('',*,*,#9617,.F.);
#13061=ORIENTED_EDGE('',*,*,#9632,.F.);
#13062=ORIENTED_EDGE('',*,*,#9630,.F.);
#13063=ORIENTED_EDGE('',*,*,#9128,.F.);
#13064=ORIENTED_EDGE('',*,*,#9146,.F.);
#13065=ORIENTED_EDGE('',*,*,#9149,.F.);
#13066=ORIENTED_EDGE('',*,*,#9152,.F.);
#13067=ORIENTED_EDGE('',*,*,#9155,.F.);
#13068=ORIENTED_EDGE('',*,*,#9158,.F.);
#13069=ORIENTED_EDGE('',*,*,#9161,.F.);
#13070=ORIENTED_EDGE('',*,*,#9164,.F.);
#13071=ORIENTED_EDGE('',*,*,#9167,.F.);
#13072=ORIENTED_EDGE('',*,*,#9170,.F.);
#13073=ORIENTED_EDGE('',*,*,#9173,.F.);
#13074=ORIENTED_EDGE('',*,*,#9176,.F.);
#13075=ORIENTED_EDGE('',*,*,#9179,.F.);
#13076=ORIENTED_EDGE('',*,*,#9182,.F.);
#13077=ORIENTED_EDGE('',*,*,#9185,.F.);
#13078=ORIENTED_EDGE('',*,*,#9188,.F.);
#13079=ORIENTED_EDGE('',*,*,#9191,.F.);
#13080=ORIENTED_EDGE('',*,*,#9194,.F.);
#13081=ORIENTED_EDGE('',*,*,#9197,.F.);
#13082=ORIENTED_EDGE('',*,*,#9200,.F.);
#13083=ORIENTED_EDGE('',*,*,#9203,.F.);
#13084=ORIENTED_EDGE('',*,*,#9206,.F.);
#13085=ORIENTED_EDGE('',*,*,#9209,.F.);
#13086=ORIENTED_EDGE('',*,*,#9212,.F.);
#13087=ORIENTED_EDGE('',*,*,#9215,.F.);
#13088=ORIENTED_EDGE('',*,*,#9218,.F.);
#13089=ORIENTED_EDGE('',*,*,#9221,.F.);
#13090=ORIENTED_EDGE('',*,*,#9224,.F.);
#13091=ORIENTED_EDGE('',*,*,#9227,.F.);
#13092=ORIENTED_EDGE('',*,*,#9230,.F.);
#13093=ORIENTED_EDGE('',*,*,#9233,.F.);
#13094=ORIENTED_EDGE('',*,*,#9236,.F.);
#13095=ORIENTED_EDGE('',*,*,#9239,.F.);
#13096=ORIENTED_EDGE('',*,*,#9242,.F.);
#13097=ORIENTED_EDGE('',*,*,#9245,.F.);
#13098=ORIENTED_EDGE('',*,*,#9248,.F.);
#13099=ORIENTED_EDGE('',*,*,#9251,.F.);
#13100=ORIENTED_EDGE('',*,*,#9254,.F.);
#13101=ORIENTED_EDGE('',*,*,#9257,.F.);
#13102=ORIENTED_EDGE('',*,*,#9260,.F.);
#13103=ORIENTED_EDGE('',*,*,#9263,.F.);
#13104=ORIENTED_EDGE('',*,*,#9266,.F.);
#13105=ORIENTED_EDGE('',*,*,#9269,.F.);
#13106=ORIENTED_EDGE('',*,*,#9272,.F.);
#13107=ORIENTED_EDGE('',*,*,#9275,.F.);
#13108=ORIENTED_EDGE('',*,*,#9278,.F.);
#13109=ORIENTED_EDGE('',*,*,#9281,.F.);
#13110=ORIENTED_EDGE('',*,*,#9284,.F.);
#13111=ORIENTED_EDGE('',*,*,#9287,.F.);
#13112=ORIENTED_EDGE('',*,*,#9290,.F.);
#13113=ORIENTED_EDGE('',*,*,#9293,.F.);
#13114=ORIENTED_EDGE('',*,*,#9296,.F.);
#13115=ORIENTED_EDGE('',*,*,#9299,.F.);
#13116=ORIENTED_EDGE('',*,*,#9302,.F.);
#13117=ORIENTED_EDGE('',*,*,#9305,.F.);
#13118=ORIENTED_EDGE('',*,*,#9308,.F.);
#13119=ORIENTED_EDGE('',*,*,#9311,.F.);
#13120=ORIENTED_EDGE('',*,*,#9314,.F.);
#13121=ORIENTED_EDGE('',*,*,#9317,.F.);
#13122=ORIENTED_EDGE('',*,*,#9320,.F.);
#13123=ORIENTED_EDGE('',*,*,#9323,.F.);
#13124=ORIENTED_EDGE('',*,*,#9326,.F.);
#13125=ORIENTED_EDGE('',*,*,#9633,.F.);
#13126=ORIENTED_EDGE('',*,*,#9382,.T.);
#13127=ORIENTED_EDGE('',*,*,#9634,.T.);
#13128=ORIENTED_EDGE('',*,*,#9635,.F.);
#13129=ORIENTED_EDGE('',*,*,#9636,.F.);
#13130=ORIENTED_EDGE('',*,*,#9637,.T.);
#13131=ORIENTED_EDGE('',*,*,#9637,.F.);
#13132=ORIENTED_EDGE('',*,*,#9638,.F.);
#13133=ORIENTED_EDGE('',*,*,#9379,.F.);
#13134=ORIENTED_EDGE('',*,*,#9376,.F.);
#13135=ORIENTED_EDGE('',*,*,#9373,.F.);
#13136=ORIENTED_EDGE('',*,*,#9370,.F.);
#13137=ORIENTED_EDGE('',*,*,#9367,.F.);
#13138=ORIENTED_EDGE('',*,*,#9364,.F.);
#13139=ORIENTED_EDGE('',*,*,#9361,.F.);
#13140=ORIENTED_EDGE('',*,*,#9358,.F.);
#13141=ORIENTED_EDGE('',*,*,#9355,.F.);
#13142=ORIENTED_EDGE('',*,*,#9352,.F.);
#13143=ORIENTED_EDGE('',*,*,#9349,.F.);
#13144=ORIENTED_EDGE('',*,*,#9346,.F.);
#13145=ORIENTED_EDGE('',*,*,#9343,.F.);
#13146=ORIENTED_EDGE('',*,*,#9340,.F.);
#13147=ORIENTED_EDGE('',*,*,#9337,.F.);
#13148=ORIENTED_EDGE('',*,*,#9334,.F.);
#13149=ORIENTED_EDGE('',*,*,#9639,.F.);
#13150=ORIENTED_EDGE('',*,*,#9640,.T.);
#13151=ORIENTED_EDGE('',*,*,#9428,.T.);
#13152=ORIENTED_EDGE('',*,*,#9425,.T.);
#13153=ORIENTED_EDGE('',*,*,#9422,.T.);
#13154=ORIENTED_EDGE('',*,*,#9419,.T.);
#13155=ORIENTED_EDGE('',*,*,#9416,.T.);
#13156=ORIENTED_EDGE('',*,*,#9413,.T.);
#13157=ORIENTED_EDGE('',*,*,#9410,.T.);
#13158=ORIENTED_EDGE('',*,*,#9407,.T.);
#13159=ORIENTED_EDGE('',*,*,#9404,.T.);
#13160=ORIENTED_EDGE('',*,*,#9401,.T.);
#13161=ORIENTED_EDGE('',*,*,#9398,.T.);
#13162=ORIENTED_EDGE('',*,*,#9395,.T.);
#13163=ORIENTED_EDGE('',*,*,#9392,.T.);
#13164=ORIENTED_EDGE('',*,*,#9389,.T.);
#13165=ORIENTED_EDGE('',*,*,#9386,.T.);
#13166=ORIENTED_EDGE('',*,*,#9383,.T.);
#13167=ORIENTED_EDGE('',*,*,#9330,.F.);
#13168=ORIENTED_EDGE('',*,*,#9641,.T.);
#13169=ORIENTED_EDGE('',*,*,#9642,.T.);
#13170=ORIENTED_EDGE('',*,*,#9639,.T.);
#13171=ORIENTED_EDGE('',*,*,#9333,.F.);
#13172=ORIENTED_EDGE('',*,*,#9426,.T.);
#13173=ORIENTED_EDGE('',*,*,#9640,.F.);
#13174=ORIENTED_EDGE('',*,*,#9642,.F.);
#13175=ORIENTED_EDGE('',*,*,#9643,.T.);
#13176=ORIENTED_EDGE('',*,*,#9634,.F.);
#13177=ORIENTED_EDGE('',*,*,#9381,.F.);
#13178=ORIENTED_EDGE('',*,*,#9385,.F.);
#13179=ORIENTED_EDGE('',*,*,#9388,.F.);
#13180=ORIENTED_EDGE('',*,*,#9391,.F.);
#13181=ORIENTED_EDGE('',*,*,#9394,.F.);
#13182=ORIENTED_EDGE('',*,*,#9397,.F.);
#13183=ORIENTED_EDGE('',*,*,#9400,.F.);
#13184=ORIENTED_EDGE('',*,*,#9403,.F.);
#13185=ORIENTED_EDGE('',*,*,#9406,.F.);
#13186=ORIENTED_EDGE('',*,*,#9409,.F.);
#13187=ORIENTED_EDGE('',*,*,#9412,.F.);
#13188=ORIENTED_EDGE('',*,*,#9415,.F.);
#13189=ORIENTED_EDGE('',*,*,#9418,.F.);
#13190=ORIENTED_EDGE('',*,*,#9421,.F.);
#13191=ORIENTED_EDGE('',*,*,#9424,.F.);
#13192=ORIENTED_EDGE('',*,*,#9427,.F.);
#13193=ORIENTED_EDGE('',*,*,#9643,.F.);
#13194=ORIENTED_EDGE('',*,*,#9641,.F.);
#13195=ORIENTED_EDGE('',*,*,#9329,.F.);
#13196=ORIENTED_EDGE('',*,*,#9336,.F.);
#13197=ORIENTED_EDGE('',*,*,#9339,.F.);
#13198=ORIENTED_EDGE('',*,*,#9342,.F.);
#13199=ORIENTED_EDGE('',*,*,#9345,.F.);
#13200=ORIENTED_EDGE('',*,*,#9348,.F.);
#13201=ORIENTED_EDGE('',*,*,#9351,.F.);
#13202=ORIENTED_EDGE('',*,*,#9354,.F.);
#13203=ORIENTED_EDGE('',*,*,#9357,.F.);
#13204=ORIENTED_EDGE('',*,*,#9360,.F.);
#13205=ORIENTED_EDGE('',*,*,#9363,.F.);
#13206=ORIENTED_EDGE('',*,*,#9366,.F.);
#13207=ORIENTED_EDGE('',*,*,#9369,.F.);
#13208=ORIENTED_EDGE('',*,*,#9372,.F.);
#13209=ORIENTED_EDGE('',*,*,#9375,.F.);
#13210=ORIENTED_EDGE('',*,*,#9378,.F.);
#13211=ORIENTED_EDGE('',*,*,#9644,.F.);
#13212=ORIENTED_EDGE('',*,*,#9377,.T.);
#13213=ORIENTED_EDGE('',*,*,#9638,.T.);
#13214=ORIENTED_EDGE('',*,*,#9645,.F.);
#13215=ORIENTED_EDGE('',*,*,#9644,.T.);
#13216=ORIENTED_EDGE('',*,*,#9646,.T.);
#13217=ORIENTED_EDGE('',*,*,#9647,.F.);
#13218=ORIENTED_EDGE('',*,*,#9648,.F.);
#13219=ORIENTED_EDGE('',*,*,#9649,.F.);
#13220=ORIENTED_EDGE('',*,*,#9650,.F.);
#13221=ORIENTED_EDGE('',*,*,#9649,.T.);
#13222=ORIENTED_EDGE('',*,*,#9651,.T.);
#13223=ORIENTED_EDGE('',*,*,#9652,.T.);
#13224=ORIENTED_EDGE('',*,*,#9653,.F.);
#13225=ORIENTED_EDGE('',*,*,#9654,.F.);
#13226=ORIENTED_EDGE('',*,*,#9648,.T.);
#13227=ORIENTED_EDGE('',*,*,#9655,.T.);
#13228=ORIENTED_EDGE('',*,*,#9656,.T.);
#13229=ORIENTED_EDGE('',*,*,#9651,.F.);
#13230=ORIENTED_EDGE('',*,*,#9657,.F.);
#13231=ORIENTED_EDGE('',*,*,#9658,.F.);
#13232=ORIENTED_EDGE('',*,*,#9659,.F.);
#13233=ORIENTED_EDGE('',*,*,#9660,.T.);
#13234=ORIENTED_EDGE('',*,*,#9655,.F.);
#13235=ORIENTED_EDGE('',*,*,#9647,.T.);
#13236=ORIENTED_EDGE('',*,*,#9661,.F.);
#13237=ORIENTED_EDGE('',*,*,#9652,.F.);
#13238=ORIENTED_EDGE('',*,*,#9656,.F.);
#13239=ORIENTED_EDGE('',*,*,#9660,.F.);
#13240=ORIENTED_EDGE('',*,*,#9650,.T.);
#13241=ORIENTED_EDGE('',*,*,#9662,.F.);
#13242=ORIENTED_EDGE('',*,*,#9663,.T.);
#13243=ORIENTED_EDGE('',*,*,#9664,.T.);
#13244=ORIENTED_EDGE('',*,*,#9657,.T.);
#13245=ORIENTED_EDGE('',*,*,#9665,.T.);
#13246=ORIENTED_EDGE('',*,*,#9666,.T.);
#13247=ORIENTED_EDGE('',*,*,#9667,.F.);
#13248=ORIENTED_EDGE('',*,*,#9654,.T.);
#13249=ORIENTED_EDGE('',*,*,#9668,.F.);
#13250=ORIENTED_EDGE('',*,*,#9669,.T.);
#13251=ORIENTED_EDGE('',*,*,#9662,.T.);
#13252=ORIENTED_EDGE('',*,*,#9653,.T.);
#13253=ORIENTED_EDGE('',*,*,#9670,.F.);
#13254=ORIENTED_EDGE('',*,*,#9671,.T.);
#13255=ORIENTED_EDGE('',*,*,#9668,.T.);
#13256=ORIENTED_EDGE('',*,*,#9672,.T.);
#13257=ORIENTED_EDGE('',*,*,#9673,.F.);
#13258=ORIENTED_EDGE('',*,*,#9674,.F.);
#13259=ORIENTED_EDGE('',*,*,#9675,.F.);
#13260=ORIENTED_EDGE('',*,*,#9676,.F.);
#13261=ORIENTED_EDGE('',*,*,#9675,.T.);
#13262=ORIENTED_EDGE('',*,*,#9677,.T.);
#13263=ORIENTED_EDGE('',*,*,#9678,.T.);
#13264=ORIENTED_EDGE('',*,*,#9679,.F.);
#13265=ORIENTED_EDGE('',*,*,#9680,.F.);
#13266=ORIENTED_EDGE('',*,*,#9674,.T.);
#13267=ORIENTED_EDGE('',*,*,#9681,.T.);
#13268=ORIENTED_EDGE('',*,*,#9682,.T.);
#13269=ORIENTED_EDGE('',*,*,#9677,.F.);
#13270=ORIENTED_EDGE('',*,*,#9663,.F.);
#13271=ORIENTED_EDGE('',*,*,#9669,.F.);
#13272=ORIENTED_EDGE('',*,*,#9671,.F.);
#13273=ORIENTED_EDGE('',*,*,#9683,.T.);
#13274=ORIENTED_EDGE('',*,*,#9681,.F.);
#13275=ORIENTED_EDGE('',*,*,#9673,.T.);
#13276=ORIENTED_EDGE('',*,*,#9684,.F.);
#13277=ORIENTED_EDGE('',*,*,#9678,.F.);
#13278=ORIENTED_EDGE('',*,*,#9682,.F.);
#13279=ORIENTED_EDGE('',*,*,#9683,.F.);
#13280=ORIENTED_EDGE('',*,*,#9676,.T.);
#13281=ORIENTED_EDGE('',*,*,#9685,.F.);
#13282=ORIENTED_EDGE('',*,*,#9686,.T.);
#13283=ORIENTED_EDGE('',*,*,#9687,.T.);
#13284=ORIENTED_EDGE('',*,*,#9680,.T.);
#13285=ORIENTED_EDGE('',*,*,#9688,.F.);
#13286=ORIENTED_EDGE('',*,*,#9689,.T.);
#13287=ORIENTED_EDGE('',*,*,#9685,.T.);
#13288=ORIENTED_EDGE('',*,*,#9679,.T.);
#13289=ORIENTED_EDGE('',*,*,#9690,.F.);
#13290=ORIENTED_EDGE('',*,*,#9691,.T.);
#13291=ORIENTED_EDGE('',*,*,#9688,.T.);
#13292=ORIENTED_EDGE('',*,*,#9692,.T.);
#13293=ORIENTED_EDGE('',*,*,#9693,.F.);
#13294=ORIENTED_EDGE('',*,*,#9694,.F.);
#13295=ORIENTED_EDGE('',*,*,#9695,.F.);
#13296=ORIENTED_EDGE('',*,*,#9696,.F.);
#13297=ORIENTED_EDGE('',*,*,#9695,.T.);
#13298=ORIENTED_EDGE('',*,*,#9697,.T.);
#13299=ORIENTED_EDGE('',*,*,#9698,.T.);
#13300=ORIENTED_EDGE('',*,*,#9699,.F.);
#13301=ORIENTED_EDGE('',*,*,#9700,.F.);
#13302=ORIENTED_EDGE('',*,*,#9694,.T.);
#13303=ORIENTED_EDGE('',*,*,#9701,.T.);
#13304=ORIENTED_EDGE('',*,*,#9702,.T.);
#13305=ORIENTED_EDGE('',*,*,#9697,.F.);
#13306=ORIENTED_EDGE('',*,*,#9686,.F.);
#13307=ORIENTED_EDGE('',*,*,#9689,.F.);
#13308=ORIENTED_EDGE('',*,*,#9691,.F.);
#13309=ORIENTED_EDGE('',*,*,#9703,.T.);
#13310=ORIENTED_EDGE('',*,*,#9701,.F.);
#13311=ORIENTED_EDGE('',*,*,#9693,.T.);
#13312=ORIENTED_EDGE('',*,*,#9704,.F.);
#13313=ORIENTED_EDGE('',*,*,#9698,.F.);
#13314=ORIENTED_EDGE('',*,*,#9702,.F.);
#13315=ORIENTED_EDGE('',*,*,#9703,.F.);
#13316=ORIENTED_EDGE('',*,*,#9696,.T.);
#13317=ORIENTED_EDGE('',*,*,#9705,.F.);
#13318=ORIENTED_EDGE('',*,*,#9706,.T.);
#13319=ORIENTED_EDGE('',*,*,#9707,.T.);
#13320=ORIENTED_EDGE('',*,*,#9700,.T.);
#13321=ORIENTED_EDGE('',*,*,#9708,.F.);
#13322=ORIENTED_EDGE('',*,*,#9709,.T.);
#13323=ORIENTED_EDGE('',*,*,#9705,.T.);
#13324=ORIENTED_EDGE('',*,*,#9699,.T.);
#13325=ORIENTED_EDGE('',*,*,#9710,.F.);
#13326=ORIENTED_EDGE('',*,*,#9711,.T.);
#13327=ORIENTED_EDGE('',*,*,#9708,.T.);
#13328=ORIENTED_EDGE('',*,*,#9712,.T.);
#13329=ORIENTED_EDGE('',*,*,#9713,.F.);
#13330=ORIENTED_EDGE('',*,*,#9714,.F.);
#13331=ORIENTED_EDGE('',*,*,#9715,.F.);
#13332=ORIENTED_EDGE('',*,*,#9716,.F.);
#13333=ORIENTED_EDGE('',*,*,#9715,.T.);
#13334=ORIENTED_EDGE('',*,*,#9717,.T.);
#13335=ORIENTED_EDGE('',*,*,#9718,.T.);
#13336=ORIENTED_EDGE('',*,*,#9719,.F.);
#13337=ORIENTED_EDGE('',*,*,#9720,.F.);
#13338=ORIENTED_EDGE('',*,*,#9714,.T.);
#13339=ORIENTED_EDGE('',*,*,#9721,.T.);
#13340=ORIENTED_EDGE('',*,*,#9722,.T.);
#13341=ORIENTED_EDGE('',*,*,#9717,.F.);
#13342=ORIENTED_EDGE('',*,*,#9706,.F.);
#13343=ORIENTED_EDGE('',*,*,#9709,.F.);
#13344=ORIENTED_EDGE('',*,*,#9711,.F.);
#13345=ORIENTED_EDGE('',*,*,#9723,.T.);
#13346=ORIENTED_EDGE('',*,*,#9721,.F.);
#13347=ORIENTED_EDGE('',*,*,#9713,.T.);
#13348=ORIENTED_EDGE('',*,*,#9724,.F.);
#13349=ORIENTED_EDGE('',*,*,#9718,.F.);
#13350=ORIENTED_EDGE('',*,*,#9722,.F.);
#13351=ORIENTED_EDGE('',*,*,#9723,.F.);
#13352=ORIENTED_EDGE('',*,*,#9716,.T.);
#13353=ORIENTED_EDGE('',*,*,#9725,.F.);
#13354=ORIENTED_EDGE('',*,*,#9726,.T.);
#13355=ORIENTED_EDGE('',*,*,#9727,.T.);
#13356=ORIENTED_EDGE('',*,*,#9720,.T.);
#13357=ORIENTED_EDGE('',*,*,#9728,.F.);
#13358=ORIENTED_EDGE('',*,*,#9729,.T.);
#13359=ORIENTED_EDGE('',*,*,#9725,.T.);
#13360=ORIENTED_EDGE('',*,*,#9719,.T.);
#13361=ORIENTED_EDGE('',*,*,#9730,.F.);
#13362=ORIENTED_EDGE('',*,*,#9731,.T.);
#13363=ORIENTED_EDGE('',*,*,#9728,.T.);
#13364=ORIENTED_EDGE('',*,*,#9732,.T.);
#13365=ORIENTED_EDGE('',*,*,#9733,.F.);
#13366=ORIENTED_EDGE('',*,*,#9734,.F.);
#13367=ORIENTED_EDGE('',*,*,#9735,.F.);
#13368=ORIENTED_EDGE('',*,*,#9736,.F.);
#13369=ORIENTED_EDGE('',*,*,#9735,.T.);
#13370=ORIENTED_EDGE('',*,*,#9737,.T.);
#13371=ORIENTED_EDGE('',*,*,#9738,.T.);
#13372=ORIENTED_EDGE('',*,*,#9739,.F.);
#13373=ORIENTED_EDGE('',*,*,#9740,.F.);
#13374=ORIENTED_EDGE('',*,*,#9734,.T.);
#13375=ORIENTED_EDGE('',*,*,#9741,.T.);
#13376=ORIENTED_EDGE('',*,*,#9742,.T.);
#13377=ORIENTED_EDGE('',*,*,#9737,.F.);
#13378=ORIENTED_EDGE('',*,*,#9726,.F.);
#13379=ORIENTED_EDGE('',*,*,#9729,.F.);
#13380=ORIENTED_EDGE('',*,*,#9731,.F.);
#13381=ORIENTED_EDGE('',*,*,#9743,.T.);
#13382=ORIENTED_EDGE('',*,*,#9741,.F.);
#13383=ORIENTED_EDGE('',*,*,#9733,.T.);
#13384=ORIENTED_EDGE('',*,*,#9744,.F.);
#13385=ORIENTED_EDGE('',*,*,#9738,.F.);
#13386=ORIENTED_EDGE('',*,*,#9742,.F.);
#13387=ORIENTED_EDGE('',*,*,#9743,.F.);
#13388=ORIENTED_EDGE('',*,*,#9736,.T.);
#13389=ORIENTED_EDGE('',*,*,#9745,.F.);
#13390=ORIENTED_EDGE('',*,*,#9746,.T.);
#13391=ORIENTED_EDGE('',*,*,#9747,.T.);
#13392=ORIENTED_EDGE('',*,*,#9740,.T.);
#13393=ORIENTED_EDGE('',*,*,#9748,.F.);
#13394=ORIENTED_EDGE('',*,*,#9749,.T.);
#13395=ORIENTED_EDGE('',*,*,#9745,.T.);
#13396=ORIENTED_EDGE('',*,*,#9739,.T.);
#13397=ORIENTED_EDGE('',*,*,#9750,.F.);
#13398=ORIENTED_EDGE('',*,*,#9751,.T.);
#13399=ORIENTED_EDGE('',*,*,#9748,.T.);
#13400=ORIENTED_EDGE('',*,*,#9752,.T.);
#13401=ORIENTED_EDGE('',*,*,#9753,.F.);
#13402=ORIENTED_EDGE('',*,*,#9754,.F.);
#13403=ORIENTED_EDGE('',*,*,#9755,.F.);
#13404=ORIENTED_EDGE('',*,*,#9756,.F.);
#13405=ORIENTED_EDGE('',*,*,#9755,.T.);
#13406=ORIENTED_EDGE('',*,*,#9757,.T.);
#13407=ORIENTED_EDGE('',*,*,#9758,.T.);
#13408=ORIENTED_EDGE('',*,*,#9759,.F.);
#13409=ORIENTED_EDGE('',*,*,#9760,.F.);
#13410=ORIENTED_EDGE('',*,*,#9754,.T.);
#13411=ORIENTED_EDGE('',*,*,#9761,.T.);
#13412=ORIENTED_EDGE('',*,*,#9762,.T.);
#13413=ORIENTED_EDGE('',*,*,#9757,.F.);
#13414=ORIENTED_EDGE('',*,*,#9746,.F.);
#13415=ORIENTED_EDGE('',*,*,#9749,.F.);
#13416=ORIENTED_EDGE('',*,*,#9751,.F.);
#13417=ORIENTED_EDGE('',*,*,#9763,.T.);
#13418=ORIENTED_EDGE('',*,*,#9761,.F.);
#13419=ORIENTED_EDGE('',*,*,#9753,.T.);
#13420=ORIENTED_EDGE('',*,*,#9764,.F.);
#13421=ORIENTED_EDGE('',*,*,#9758,.F.);
#13422=ORIENTED_EDGE('',*,*,#9762,.F.);
#13423=ORIENTED_EDGE('',*,*,#9763,.F.);
#13424=ORIENTED_EDGE('',*,*,#9756,.T.);
#13425=ORIENTED_EDGE('',*,*,#9765,.F.);
#13426=ORIENTED_EDGE('',*,*,#9766,.T.);
#13427=ORIENTED_EDGE('',*,*,#9767,.T.);
#13428=ORIENTED_EDGE('',*,*,#9760,.T.);
#13429=ORIENTED_EDGE('',*,*,#9768,.F.);
#13430=ORIENTED_EDGE('',*,*,#9769,.T.);
#13431=ORIENTED_EDGE('',*,*,#9765,.T.);
#13432=ORIENTED_EDGE('',*,*,#9759,.T.);
#13433=ORIENTED_EDGE('',*,*,#9770,.F.);
#13434=ORIENTED_EDGE('',*,*,#9771,.T.);
#13435=ORIENTED_EDGE('',*,*,#9768,.T.);
#13436=ORIENTED_EDGE('',*,*,#9772,.T.);
#13437=ORIENTED_EDGE('',*,*,#9773,.F.);
#13438=ORIENTED_EDGE('',*,*,#9774,.F.);
#13439=ORIENTED_EDGE('',*,*,#9775,.F.);
#13440=ORIENTED_EDGE('',*,*,#9776,.F.);
#13441=ORIENTED_EDGE('',*,*,#9775,.T.);
#13442=ORIENTED_EDGE('',*,*,#9777,.T.);
#13443=ORIENTED_EDGE('',*,*,#9778,.T.);
#13444=ORIENTED_EDGE('',*,*,#9779,.F.);
#13445=ORIENTED_EDGE('',*,*,#9780,.F.);
#13446=ORIENTED_EDGE('',*,*,#9774,.T.);
#13447=ORIENTED_EDGE('',*,*,#9781,.T.);
#13448=ORIENTED_EDGE('',*,*,#9782,.T.);
#13449=ORIENTED_EDGE('',*,*,#9777,.F.);
#13450=ORIENTED_EDGE('',*,*,#9766,.F.);
#13451=ORIENTED_EDGE('',*,*,#9769,.F.);
#13452=ORIENTED_EDGE('',*,*,#9771,.F.);
#13453=ORIENTED_EDGE('',*,*,#9783,.T.);
#13454=ORIENTED_EDGE('',*,*,#9781,.F.);
#13455=ORIENTED_EDGE('',*,*,#9773,.T.);
#13456=ORIENTED_EDGE('',*,*,#9784,.F.);
#13457=ORIENTED_EDGE('',*,*,#9778,.F.);
#13458=ORIENTED_EDGE('',*,*,#9782,.F.);
#13459=ORIENTED_EDGE('',*,*,#9783,.F.);
#13460=ORIENTED_EDGE('',*,*,#9776,.T.);
#13461=ORIENTED_EDGE('',*,*,#9785,.F.);
#13462=ORIENTED_EDGE('',*,*,#9786,.T.);
#13463=ORIENTED_EDGE('',*,*,#9787,.T.);
#13464=ORIENTED_EDGE('',*,*,#9780,.T.);
#13465=ORIENTED_EDGE('',*,*,#9788,.F.);
#13466=ORIENTED_EDGE('',*,*,#9789,.T.);
#13467=ORIENTED_EDGE('',*,*,#9785,.T.);
#13468=ORIENTED_EDGE('',*,*,#9779,.T.);
#13469=ORIENTED_EDGE('',*,*,#9790,.F.);
#13470=ORIENTED_EDGE('',*,*,#9791,.T.);
#13471=ORIENTED_EDGE('',*,*,#9788,.T.);
#13472=ORIENTED_EDGE('',*,*,#9792,.T.);
#13473=ORIENTED_EDGE('',*,*,#9793,.T.);
#13474=ORIENTED_EDGE('',*,*,#9794,.F.);
#13475=ORIENTED_EDGE('',*,*,#9795,.F.);
#13476=ORIENTED_EDGE('',*,*,#9796,.F.);
#13477=ORIENTED_EDGE('',*,*,#9797,.F.);
#13478=ORIENTED_EDGE('',*,*,#9796,.T.);
#13479=ORIENTED_EDGE('',*,*,#9798,.T.);
#13480=ORIENTED_EDGE('',*,*,#9799,.T.);
#13481=ORIENTED_EDGE('',*,*,#9800,.F.);
#13482=ORIENTED_EDGE('',*,*,#9801,.F.);
#13483=ORIENTED_EDGE('',*,*,#9795,.T.);
#13484=ORIENTED_EDGE('',*,*,#9802,.T.);
#13485=ORIENTED_EDGE('',*,*,#9803,.T.);
#13486=ORIENTED_EDGE('',*,*,#9798,.F.);
#13487=ORIENTED_EDGE('',*,*,#9786,.F.);
#13488=ORIENTED_EDGE('',*,*,#9789,.F.);
#13489=ORIENTED_EDGE('',*,*,#9791,.F.);
#13490=ORIENTED_EDGE('',*,*,#9804,.T.);
#13491=ORIENTED_EDGE('',*,*,#9802,.F.);
#13492=ORIENTED_EDGE('',*,*,#9794,.T.);
#13493=ORIENTED_EDGE('',*,*,#9805,.F.);
#13494=ORIENTED_EDGE('',*,*,#9799,.F.);
#13495=ORIENTED_EDGE('',*,*,#9803,.F.);
#13496=ORIENTED_EDGE('',*,*,#9804,.F.);
#13497=ORIENTED_EDGE('',*,*,#9806,.F.);
#13498=ORIENTED_EDGE('',*,*,#9797,.T.);
#13499=ORIENTED_EDGE('',*,*,#9807,.F.);
#13500=ORIENTED_EDGE('',*,*,#9808,.T.);
#13501=ORIENTED_EDGE('',*,*,#9809,.T.);
#13502=ORIENTED_EDGE('',*,*,#9801,.T.);
#13503=ORIENTED_EDGE('',*,*,#9810,.F.);
#13504=ORIENTED_EDGE('',*,*,#9811,.T.);
#13505=ORIENTED_EDGE('',*,*,#9807,.T.);
#13506=ORIENTED_EDGE('',*,*,#9800,.T.);
#13507=ORIENTED_EDGE('',*,*,#9812,.F.);
#13508=ORIENTED_EDGE('',*,*,#9813,.T.);
#13509=ORIENTED_EDGE('',*,*,#9810,.T.);
#13510=ORIENTED_EDGE('',*,*,#9814,.T.);
#13511=ORIENTED_EDGE('',*,*,#9815,.F.);
#13512=ORIENTED_EDGE('',*,*,#9816,.F.);
#13513=ORIENTED_EDGE('',*,*,#9817,.F.);
#13514=ORIENTED_EDGE('',*,*,#9818,.F.);
#13515=ORIENTED_EDGE('',*,*,#9817,.T.);
#13516=ORIENTED_EDGE('',*,*,#9819,.T.);
#13517=ORIENTED_EDGE('',*,*,#9820,.T.);
#13518=ORIENTED_EDGE('',*,*,#9821,.F.);
#13519=ORIENTED_EDGE('',*,*,#9822,.F.);
#13520=ORIENTED_EDGE('',*,*,#9816,.T.);
#13521=ORIENTED_EDGE('',*,*,#9823,.T.);
#13522=ORIENTED_EDGE('',*,*,#9824,.T.);
#13523=ORIENTED_EDGE('',*,*,#9819,.F.);
#13524=ORIENTED_EDGE('',*,*,#9808,.F.);
#13525=ORIENTED_EDGE('',*,*,#9811,.F.);
#13526=ORIENTED_EDGE('',*,*,#9813,.F.);
#13527=ORIENTED_EDGE('',*,*,#9825,.T.);
#13528=ORIENTED_EDGE('',*,*,#9823,.F.);
#13529=ORIENTED_EDGE('',*,*,#9815,.T.);
#13530=ORIENTED_EDGE('',*,*,#9826,.F.);
#13531=ORIENTED_EDGE('',*,*,#9820,.F.);
#13532=ORIENTED_EDGE('',*,*,#9824,.F.);
#13533=ORIENTED_EDGE('',*,*,#9825,.F.);
#13534=ORIENTED_EDGE('',*,*,#9818,.T.);
#13535=ORIENTED_EDGE('',*,*,#9827,.F.);
#13536=ORIENTED_EDGE('',*,*,#9828,.T.);
#13537=ORIENTED_EDGE('',*,*,#9829,.T.);
#13538=ORIENTED_EDGE('',*,*,#9822,.T.);
#13539=ORIENTED_EDGE('',*,*,#9830,.F.);
#13540=ORIENTED_EDGE('',*,*,#9831,.T.);
#13541=ORIENTED_EDGE('',*,*,#9827,.T.);
#13542=ORIENTED_EDGE('',*,*,#9821,.T.);
#13543=ORIENTED_EDGE('',*,*,#9832,.F.);
#13544=ORIENTED_EDGE('',*,*,#9833,.T.);
#13545=ORIENTED_EDGE('',*,*,#9830,.T.);
#13546=ORIENTED_EDGE('',*,*,#9834,.T.);
#13547=ORIENTED_EDGE('',*,*,#9835,.F.);
#13548=ORIENTED_EDGE('',*,*,#9836,.F.);
#13549=ORIENTED_EDGE('',*,*,#9837,.F.);
#13550=ORIENTED_EDGE('',*,*,#9838,.F.);
#13551=ORIENTED_EDGE('',*,*,#9837,.T.);
#13552=ORIENTED_EDGE('',*,*,#9839,.T.);
#13553=ORIENTED_EDGE('',*,*,#9840,.T.);
#13554=ORIENTED_EDGE('',*,*,#9841,.F.);
#13555=ORIENTED_EDGE('',*,*,#9842,.F.);
#13556=ORIENTED_EDGE('',*,*,#9836,.T.);
#13557=ORIENTED_EDGE('',*,*,#9843,.T.);
#13558=ORIENTED_EDGE('',*,*,#9844,.T.);
#13559=ORIENTED_EDGE('',*,*,#9839,.F.);
#13560=ORIENTED_EDGE('',*,*,#9828,.F.);
#13561=ORIENTED_EDGE('',*,*,#9831,.F.);
#13562=ORIENTED_EDGE('',*,*,#9833,.F.);
#13563=ORIENTED_EDGE('',*,*,#9845,.T.);
#13564=ORIENTED_EDGE('',*,*,#9843,.F.);
#13565=ORIENTED_EDGE('',*,*,#9835,.T.);
#13566=ORIENTED_EDGE('',*,*,#9846,.F.);
#13567=ORIENTED_EDGE('',*,*,#9840,.F.);
#13568=ORIENTED_EDGE('',*,*,#9844,.F.);
#13569=ORIENTED_EDGE('',*,*,#9845,.F.);
#13570=ORIENTED_EDGE('',*,*,#9838,.T.);
#13571=ORIENTED_EDGE('',*,*,#9847,.F.);
#13572=ORIENTED_EDGE('',*,*,#9848,.T.);
#13573=ORIENTED_EDGE('',*,*,#9849,.T.);
#13574=ORIENTED_EDGE('',*,*,#9842,.T.);
#13575=ORIENTED_EDGE('',*,*,#9850,.F.);
#13576=ORIENTED_EDGE('',*,*,#9851,.T.);
#13577=ORIENTED_EDGE('',*,*,#9847,.T.);
#13578=ORIENTED_EDGE('',*,*,#9841,.T.);
#13579=ORIENTED_EDGE('',*,*,#9852,.F.);
#13580=ORIENTED_EDGE('',*,*,#9853,.T.);
#13581=ORIENTED_EDGE('',*,*,#9850,.T.);
#13582=ORIENTED_EDGE('',*,*,#9854,.T.);
#13583=ORIENTED_EDGE('',*,*,#9855,.F.);
#13584=ORIENTED_EDGE('',*,*,#9856,.F.);
#13585=ORIENTED_EDGE('',*,*,#9857,.F.);
#13586=ORIENTED_EDGE('',*,*,#9858,.F.);
#13587=ORIENTED_EDGE('',*,*,#9857,.T.);
#13588=ORIENTED_EDGE('',*,*,#9859,.T.);
#13589=ORIENTED_EDGE('',*,*,#9860,.T.);
#13590=ORIENTED_EDGE('',*,*,#9861,.F.);
#13591=ORIENTED_EDGE('',*,*,#9862,.F.);
#13592=ORIENTED_EDGE('',*,*,#9856,.T.);
#13593=ORIENTED_EDGE('',*,*,#9863,.T.);
#13594=ORIENTED_EDGE('',*,*,#9864,.T.);
#13595=ORIENTED_EDGE('',*,*,#9859,.F.);
#13596=ORIENTED_EDGE('',*,*,#9848,.F.);
#13597=ORIENTED_EDGE('',*,*,#9851,.F.);
#13598=ORIENTED_EDGE('',*,*,#9853,.F.);
#13599=ORIENTED_EDGE('',*,*,#9865,.T.);
#13600=ORIENTED_EDGE('',*,*,#9863,.F.);
#13601=ORIENTED_EDGE('',*,*,#9855,.T.);
#13602=ORIENTED_EDGE('',*,*,#9866,.F.);
#13603=ORIENTED_EDGE('',*,*,#9860,.F.);
#13604=ORIENTED_EDGE('',*,*,#9864,.F.);
#13605=ORIENTED_EDGE('',*,*,#9865,.F.);
#13606=ORIENTED_EDGE('',*,*,#9858,.T.);
#13607=ORIENTED_EDGE('',*,*,#9867,.F.);
#13608=ORIENTED_EDGE('',*,*,#9868,.T.);
#13609=ORIENTED_EDGE('',*,*,#9869,.T.);
#13610=ORIENTED_EDGE('',*,*,#9862,.T.);
#13611=ORIENTED_EDGE('',*,*,#9870,.F.);
#13612=ORIENTED_EDGE('',*,*,#9871,.T.);
#13613=ORIENTED_EDGE('',*,*,#9867,.T.);
#13614=ORIENTED_EDGE('',*,*,#9861,.T.);
#13615=ORIENTED_EDGE('',*,*,#9872,.F.);
#13616=ORIENTED_EDGE('',*,*,#9873,.T.);
#13617=ORIENTED_EDGE('',*,*,#9870,.T.);
#13618=ORIENTED_EDGE('',*,*,#9874,.T.);
#13619=ORIENTED_EDGE('',*,*,#9875,.F.);
#13620=ORIENTED_EDGE('',*,*,#9876,.F.);
#13621=ORIENTED_EDGE('',*,*,#9877,.F.);
#13622=ORIENTED_EDGE('',*,*,#9878,.F.);
#13623=ORIENTED_EDGE('',*,*,#9877,.T.);
#13624=ORIENTED_EDGE('',*,*,#9879,.T.);
#13625=ORIENTED_EDGE('',*,*,#9880,.T.);
#13626=ORIENTED_EDGE('',*,*,#9881,.F.);
#13627=ORIENTED_EDGE('',*,*,#9882,.F.);
#13628=ORIENTED_EDGE('',*,*,#9876,.T.);
#13629=ORIENTED_EDGE('',*,*,#9883,.T.);
#13630=ORIENTED_EDGE('',*,*,#9884,.T.);
#13631=ORIENTED_EDGE('',*,*,#9879,.F.);
#13632=ORIENTED_EDGE('',*,*,#9868,.F.);
#13633=ORIENTED_EDGE('',*,*,#9871,.F.);
#13634=ORIENTED_EDGE('',*,*,#9873,.F.);
#13635=ORIENTED_EDGE('',*,*,#9885,.T.);
#13636=ORIENTED_EDGE('',*,*,#9883,.F.);
#13637=ORIENTED_EDGE('',*,*,#9875,.T.);
#13638=ORIENTED_EDGE('',*,*,#9886,.F.);
#13639=ORIENTED_EDGE('',*,*,#9880,.F.);
#13640=ORIENTED_EDGE('',*,*,#9884,.F.);
#13641=ORIENTED_EDGE('',*,*,#9885,.F.);
#13642=ORIENTED_EDGE('',*,*,#9878,.T.);
#13643=ORIENTED_EDGE('',*,*,#9887,.F.);
#13644=ORIENTED_EDGE('',*,*,#9888,.T.);
#13645=ORIENTED_EDGE('',*,*,#9889,.T.);
#13646=ORIENTED_EDGE('',*,*,#9882,.T.);
#13647=ORIENTED_EDGE('',*,*,#9890,.F.);
#13648=ORIENTED_EDGE('',*,*,#9891,.T.);
#13649=ORIENTED_EDGE('',*,*,#9887,.T.);
#13650=ORIENTED_EDGE('',*,*,#9881,.T.);
#13651=ORIENTED_EDGE('',*,*,#9892,.F.);
#13652=ORIENTED_EDGE('',*,*,#9893,.T.);
#13653=ORIENTED_EDGE('',*,*,#9890,.T.);
#13654=ORIENTED_EDGE('',*,*,#9894,.T.);
#13655=ORIENTED_EDGE('',*,*,#9895,.F.);
#13656=ORIENTED_EDGE('',*,*,#9896,.F.);
#13657=ORIENTED_EDGE('',*,*,#9897,.F.);
#13658=ORIENTED_EDGE('',*,*,#9898,.F.);
#13659=ORIENTED_EDGE('',*,*,#9897,.T.);
#13660=ORIENTED_EDGE('',*,*,#9899,.T.);
#13661=ORIENTED_EDGE('',*,*,#9900,.T.);
#13662=ORIENTED_EDGE('',*,*,#9901,.F.);
#13663=ORIENTED_EDGE('',*,*,#9902,.F.);
#13664=ORIENTED_EDGE('',*,*,#9896,.T.);
#13665=ORIENTED_EDGE('',*,*,#9903,.T.);
#13666=ORIENTED_EDGE('',*,*,#9904,.T.);
#13667=ORIENTED_EDGE('',*,*,#9899,.F.);
#13668=ORIENTED_EDGE('',*,*,#9888,.F.);
#13669=ORIENTED_EDGE('',*,*,#9891,.F.);
#13670=ORIENTED_EDGE('',*,*,#9893,.F.);
#13671=ORIENTED_EDGE('',*,*,#9905,.T.);
#13672=ORIENTED_EDGE('',*,*,#9903,.F.);
#13673=ORIENTED_EDGE('',*,*,#9895,.T.);
#13674=ORIENTED_EDGE('',*,*,#9906,.F.);
#13675=ORIENTED_EDGE('',*,*,#9900,.F.);
#13676=ORIENTED_EDGE('',*,*,#9904,.F.);
#13677=ORIENTED_EDGE('',*,*,#9905,.F.);
#13678=ORIENTED_EDGE('',*,*,#9898,.T.);
#13679=ORIENTED_EDGE('',*,*,#9907,.F.);
#13680=ORIENTED_EDGE('',*,*,#9908,.T.);
#13681=ORIENTED_EDGE('',*,*,#9909,.T.);
#13682=ORIENTED_EDGE('',*,*,#9902,.T.);
#13683=ORIENTED_EDGE('',*,*,#9910,.F.);
#13684=ORIENTED_EDGE('',*,*,#9911,.T.);
#13685=ORIENTED_EDGE('',*,*,#9907,.T.);
#13686=ORIENTED_EDGE('',*,*,#9901,.T.);
#13687=ORIENTED_EDGE('',*,*,#9912,.F.);
#13688=ORIENTED_EDGE('',*,*,#9913,.T.);
#13689=ORIENTED_EDGE('',*,*,#9910,.T.);
#13690=ORIENTED_EDGE('',*,*,#9914,.T.);
#13691=ORIENTED_EDGE('',*,*,#9915,.F.);
#13692=ORIENTED_EDGE('',*,*,#9916,.F.);
#13693=ORIENTED_EDGE('',*,*,#9917,.F.);
#13694=ORIENTED_EDGE('',*,*,#9918,.F.);
#13695=ORIENTED_EDGE('',*,*,#9917,.T.);
#13696=ORIENTED_EDGE('',*,*,#9919,.T.);
#13697=ORIENTED_EDGE('',*,*,#9920,.T.);
#13698=ORIENTED_EDGE('',*,*,#9921,.F.);
#13699=ORIENTED_EDGE('',*,*,#9922,.F.);
#13700=ORIENTED_EDGE('',*,*,#9916,.T.);
#13701=ORIENTED_EDGE('',*,*,#9923,.T.);
#13702=ORIENTED_EDGE('',*,*,#9924,.T.);
#13703=ORIENTED_EDGE('',*,*,#9919,.F.);
#13704=ORIENTED_EDGE('',*,*,#9908,.F.);
#13705=ORIENTED_EDGE('',*,*,#9911,.F.);
#13706=ORIENTED_EDGE('',*,*,#9913,.F.);
#13707=ORIENTED_EDGE('',*,*,#9925,.T.);
#13708=ORIENTED_EDGE('',*,*,#9923,.F.);
#13709=ORIENTED_EDGE('',*,*,#9915,.T.);
#13710=ORIENTED_EDGE('',*,*,#9926,.F.);
#13711=ORIENTED_EDGE('',*,*,#9920,.F.);
#13712=ORIENTED_EDGE('',*,*,#9924,.F.);
#13713=ORIENTED_EDGE('',*,*,#9925,.F.);
#13714=ORIENTED_EDGE('',*,*,#9918,.T.);
#13715=ORIENTED_EDGE('',*,*,#9927,.F.);
#13716=ORIENTED_EDGE('',*,*,#9928,.T.);
#13717=ORIENTED_EDGE('',*,*,#9929,.T.);
#13718=ORIENTED_EDGE('',*,*,#9922,.T.);
#13719=ORIENTED_EDGE('',*,*,#9930,.F.);
#13720=ORIENTED_EDGE('',*,*,#9931,.T.);
#13721=ORIENTED_EDGE('',*,*,#9927,.T.);
#13722=ORIENTED_EDGE('',*,*,#9921,.T.);
#13723=ORIENTED_EDGE('',*,*,#9932,.F.);
#13724=ORIENTED_EDGE('',*,*,#9933,.T.);
#13725=ORIENTED_EDGE('',*,*,#9930,.T.);
#13726=ORIENTED_EDGE('',*,*,#9933,.F.);
#13727=ORIENTED_EDGE('',*,*,#9934,.T.);
#13728=ORIENTED_EDGE('',*,*,#9935,.F.);
#13729=ORIENTED_EDGE('',*,*,#9936,.T.);
#13730=ORIENTED_EDGE('',*,*,#9928,.F.);
#13731=ORIENTED_EDGE('',*,*,#9931,.F.);
#13732=ORIENTED_EDGE('',*,*,#9937,.T.);
#13733=ORIENTED_EDGE('',*,*,#9936,.F.);
#13734=ORIENTED_EDGE('',*,*,#9938,.F.);
#13735=ORIENTED_EDGE('',*,*,#9939,.F.);
#13736=ORIENTED_EDGE('',*,*,#9938,.T.);
#13737=ORIENTED_EDGE('',*,*,#9935,.T.);
#13738=ORIENTED_EDGE('',*,*,#9940,.T.);
#13739=ORIENTED_EDGE('',*,*,#9941,.F.);
#13740=ORIENTED_EDGE('',*,*,#9942,.F.);
#13741=ORIENTED_EDGE('',*,*,#9943,.F.);
#13742=ORIENTED_EDGE('',*,*,#9666,.F.);
#13743=ORIENTED_EDGE('',*,*,#9939,.T.);
#13744=ORIENTED_EDGE('',*,*,#9941,.T.);
#13745=ORIENTED_EDGE('',*,*,#9944,.T.);
#13746=ORIENTED_EDGE('',*,*,#9945,.F.);
#13747=ORIENTED_EDGE('',*,*,#9944,.F.);
#13748=ORIENTED_EDGE('',*,*,#9940,.F.);
#13749=ORIENTED_EDGE('',*,*,#9934,.F.);
#13750=ORIENTED_EDGE('',*,*,#9659,.T.);
#13751=ORIENTED_EDGE('',*,*,#9946,.T.);
#13752=ORIENTED_EDGE('',*,*,#9942,.T.);
#13753=ORIENTED_EDGE('',*,*,#9947,.F.);
#13754=ORIENTED_EDGE('',*,*,#9658,.T.);
#13755=ORIENTED_EDGE('',*,*,#9667,.T.);
#13756=ORIENTED_EDGE('',*,*,#9943,.T.);
#13757=ORIENTED_EDGE('',*,*,#9946,.F.);
#13758=ORIENTED_EDGE('',*,*,#9948,.F.);
#13759=ORIENTED_EDGE('',*,*,#9332,.F.);
#13760=ORIENTED_EDGE('',*,*,#9949,.T.);
#13761=ORIENTED_EDGE('',*,*,#9948,.T.);
#13762=ORIENTED_EDGE('',*,*,#9949,.F.);
#13763=ORIENTED_EDGE('',*,*,#9929,.F.);
#13764=ORIENTED_EDGE('',*,*,#9937,.F.);
#13765=ORIENTED_EDGE('',*,*,#9665,.F.);
#13766=ORIENTED_EDGE('',*,*,#9646,.F.);
#13767=ORIENTED_EDGE('',*,*,#9664,.F.);
#13768=ORIENTED_EDGE('',*,*,#9672,.F.);
#13769=ORIENTED_EDGE('',*,*,#9687,.F.);
#13770=ORIENTED_EDGE('',*,*,#9692,.F.);
#13771=ORIENTED_EDGE('',*,*,#9707,.F.);
#13772=ORIENTED_EDGE('',*,*,#9712,.F.);
#13773=ORIENTED_EDGE('',*,*,#9727,.F.);
#13774=ORIENTED_EDGE('',*,*,#9732,.F.);
#13775=ORIENTED_EDGE('',*,*,#9747,.F.);
#13776=ORIENTED_EDGE('',*,*,#9752,.F.);
#13777=ORIENTED_EDGE('',*,*,#9767,.F.);
#13778=ORIENTED_EDGE('',*,*,#9772,.F.);
#13779=ORIENTED_EDGE('',*,*,#9787,.F.);
#13780=ORIENTED_EDGE('',*,*,#9793,.F.);
#13781=ORIENTED_EDGE('',*,*,#9950,.T.);
#13782=ORIENTED_EDGE('',*,*,#9635,.T.);
#13783=ORIENTED_EDGE('',*,*,#9645,.T.);
#13784=ORIENTED_EDGE('',*,*,#9636,.T.);
#13785=ORIENTED_EDGE('',*,*,#9950,.F.);
#13786=ORIENTED_EDGE('',*,*,#9792,.F.);
#13787=ORIENTED_EDGE('',*,*,#9809,.F.);
#13788=ORIENTED_EDGE('',*,*,#9814,.F.);
#13789=ORIENTED_EDGE('',*,*,#9829,.F.);
#13790=ORIENTED_EDGE('',*,*,#9834,.F.);
#13791=ORIENTED_EDGE('',*,*,#9849,.F.);
#13792=ORIENTED_EDGE('',*,*,#9854,.F.);
#13793=ORIENTED_EDGE('',*,*,#9869,.F.);
#13794=ORIENTED_EDGE('',*,*,#9874,.F.);
#13795=ORIENTED_EDGE('',*,*,#9889,.F.);
#13796=ORIENTED_EDGE('',*,*,#9894,.F.);
#13797=ORIENTED_EDGE('',*,*,#9909,.F.);
#13798=ORIENTED_EDGE('',*,*,#9914,.F.);
#13799=ORIENTED_EDGE('',*,*,#9135,.F.);
#13800=ORIENTED_EDGE('',*,*,#9951,.T.);
#13801=ORIENTED_EDGE('',*,*,#9806,.T.);
#13802=ORIENTED_EDGE('',*,*,#9790,.T.);
#13803=ORIENTED_EDGE('',*,*,#9784,.T.);
#13804=ORIENTED_EDGE('',*,*,#9770,.T.);
#13805=ORIENTED_EDGE('',*,*,#9764,.T.);
#13806=ORIENTED_EDGE('',*,*,#9750,.T.);
#13807=ORIENTED_EDGE('',*,*,#9744,.T.);
#13808=ORIENTED_EDGE('',*,*,#9730,.T.);
#13809=ORIENTED_EDGE('',*,*,#9724,.T.);
#13810=ORIENTED_EDGE('',*,*,#9710,.T.);
#13811=ORIENTED_EDGE('',*,*,#9704,.T.);
#13812=ORIENTED_EDGE('',*,*,#9690,.T.);
#13813=ORIENTED_EDGE('',*,*,#9684,.T.);
#13814=ORIENTED_EDGE('',*,*,#9670,.T.);
#13815=ORIENTED_EDGE('',*,*,#9661,.T.);
#13816=ORIENTED_EDGE('',*,*,#9947,.T.);
#13817=ORIENTED_EDGE('',*,*,#9945,.T.);
#13818=ORIENTED_EDGE('',*,*,#9932,.T.);
#13819=ORIENTED_EDGE('',*,*,#9926,.T.);
#13820=ORIENTED_EDGE('',*,*,#9912,.T.);
#13821=ORIENTED_EDGE('',*,*,#9906,.T.);
#13822=ORIENTED_EDGE('',*,*,#9892,.T.);
#13823=ORIENTED_EDGE('',*,*,#9886,.T.);
#13824=ORIENTED_EDGE('',*,*,#9872,.T.);
#13825=ORIENTED_EDGE('',*,*,#9866,.T.);
#13826=ORIENTED_EDGE('',*,*,#9852,.T.);
#13827=ORIENTED_EDGE('',*,*,#9846,.T.);
#13828=ORIENTED_EDGE('',*,*,#9832,.T.);
#13829=ORIENTED_EDGE('',*,*,#9826,.T.);
#13830=ORIENTED_EDGE('',*,*,#9812,.T.);
#13831=ORIENTED_EDGE('',*,*,#9805,.T.);
#13832=ORIENTED_EDGE('',*,*,#9951,.F.);
#13833=ORIENTED_EDGE('',*,*,#9325,.T.);
#13834=ORIENTED_EDGE('',*,*,#9627,.T.);
#13835=ORIENTED_EDGE('',*,*,#9952,.F.);
#13836=ORIENTED_EDGE('',*,*,#9633,.T.);
#13837=ORIENTED_EDGE('',*,*,#9953,.F.);
#13838=ORIENTED_EDGE('',*,*,#9954,.T.);
#13839=ORIENTED_EDGE('',*,*,#9624,.T.);
#13840=ORIENTED_EDGE('',*,*,#9952,.T.);
#13841=ORIENTED_EDGE('',*,*,#9625,.T.);
#13842=ORIENTED_EDGE('',*,*,#9954,.F.);
#13843=ORIENTED_EDGE('',*,*,#9953,.T.);
#13844=ORIENTED_EDGE('',*,*,#9955,.T.);
#13845=ORIENTED_EDGE('',*,*,#9956,.T.);
#13846=ORIENTED_EDGE('',*,*,#9957,.T.);
#13847=ORIENTED_EDGE('',*,*,#9958,.T.);
#13848=ORIENTED_EDGE('',*,*,#9959,.T.);
#13849=ORIENTED_EDGE('',*,*,#9960,.T.);
#13850=ORIENTED_EDGE('',*,*,#9957,.F.);
#13851=ORIENTED_EDGE('',*,*,#9961,.T.);
#13852=ORIENTED_EDGE('',*,*,#9962,.T.);
#13853=ORIENTED_EDGE('',*,*,#9963,.T.);
#13854=ORIENTED_EDGE('',*,*,#9964,.F.);
#13855=ORIENTED_EDGE('',*,*,#9965,.T.);
#13856=ORIENTED_EDGE('',*,*,#9966,.T.);
#13857=ORIENTED_EDGE('',*,*,#9967,.T.);
#13858=ORIENTED_EDGE('',*,*,#9968,.T.);
#13859=ORIENTED_EDGE('',*,*,#9969,.T.);
#13860=ORIENTED_EDGE('',*,*,#9968,.F.);
#13861=ORIENTED_EDGE('',*,*,#9970,.T.);
#13862=ORIENTED_EDGE('',*,*,#9962,.F.);
#13863=ORIENTED_EDGE('',*,*,#9971,.F.);
#13864=ORIENTED_EDGE('',*,*,#9972,.T.);
#13865=ORIENTED_EDGE('',*,*,#9973,.T.);
#13866=ORIENTED_EDGE('',*,*,#9974,.T.);
#13867=ORIENTED_EDGE('',*,*,#9975,.T.);
#13868=ORIENTED_EDGE('',*,*,#9976,.T.);
#13869=ORIENTED_EDGE('',*,*,#9973,.F.);
#13870=ORIENTED_EDGE('',*,*,#9977,.T.);
#13871=ORIENTED_EDGE('',*,*,#9978,.T.);
#13872=ORIENTED_EDGE('',*,*,#9979,.T.);
#13873=ORIENTED_EDGE('',*,*,#9980,.F.);
#13874=ORIENTED_EDGE('',*,*,#9981,.T.);
#13875=ORIENTED_EDGE('',*,*,#9978,.F.);
#13876=ORIENTED_EDGE('',*,*,#9982,.T.);
#13877=ORIENTED_EDGE('',*,*,#9966,.F.);
#13878=ORIENTED_EDGE('',*,*,#9961,.F.);
#13879=ORIENTED_EDGE('',*,*,#9983,.T.);
#13880=ORIENTED_EDGE('',*,*,#9984,.T.);
#13881=ORIENTED_EDGE('',*,*,#9985,.T.);
#13882=ORIENTED_EDGE('',*,*,#9956,.F.);
#13883=ORIENTED_EDGE('',*,*,#9963,.F.);
#13884=ORIENTED_EDGE('',*,*,#9986,.F.);
#13885=ORIENTED_EDGE('',*,*,#9983,.F.);
#13886=ORIENTED_EDGE('',*,*,#9970,.F.);
#13887=ORIENTED_EDGE('',*,*,#9987,.T.);
#13888=ORIENTED_EDGE('',*,*,#9988,.T.);
#13889=ORIENTED_EDGE('',*,*,#9986,.T.);
#13890=ORIENTED_EDGE('',*,*,#9967,.F.);
#13891=ORIENTED_EDGE('',*,*,#9989,.F.);
#13892=ORIENTED_EDGE('',*,*,#9990,.F.);
#13893=ORIENTED_EDGE('',*,*,#9987,.F.);
#13894=ORIENTED_EDGE('',*,*,#9982,.F.);
#13895=ORIENTED_EDGE('',*,*,#9991,.T.);
#13896=ORIENTED_EDGE('',*,*,#9992,.F.);
#13897=ORIENTED_EDGE('',*,*,#9989,.T.);
#13898=ORIENTED_EDGE('',*,*,#9981,.F.);
#13899=ORIENTED_EDGE('',*,*,#9977,.F.);
#13900=ORIENTED_EDGE('',*,*,#9993,.F.);
#13901=ORIENTED_EDGE('',*,*,#9991,.F.);
#13902=ORIENTED_EDGE('',*,*,#9959,.F.);
#13903=ORIENTED_EDGE('',*,*,#9994,.T.);
#13904=ORIENTED_EDGE('',*,*,#9971,.T.);
#13905=ORIENTED_EDGE('',*,*,#9995,.T.);
#13906=ORIENTED_EDGE('',*,*,#9972,.F.);
#13907=ORIENTED_EDGE('',*,*,#9996,.T.);
#13908=ORIENTED_EDGE('',*,*,#9997,.T.);
#13909=ORIENTED_EDGE('',*,*,#9993,.T.);
#13910=ORIENTED_EDGE('',*,*,#9988,.F.);
#13911=ORIENTED_EDGE('',*,*,#9998,.T.);
#13912=ORIENTED_EDGE('',*,*,#9984,.F.);
#13913=ORIENTED_EDGE('',*,*,#9985,.F.);
#13914=ORIENTED_EDGE('',*,*,#9999,.F.);
#13915=ORIENTED_EDGE('',*,*,#9996,.F.);
#13916=ORIENTED_EDGE('',*,*,#9994,.F.);
#13917=ORIENTED_EDGE('',*,*,#9998,.F.);
#13918=ORIENTED_EDGE('',*,*,#9990,.T.);
#13919=ORIENTED_EDGE('',*,*,#10000,.T.);
#13920=ORIENTED_EDGE('',*,*,#9999,.T.);
#13921=ORIENTED_EDGE('',*,*,#9965,.F.);
#13922=ORIENTED_EDGE('',*,*,#10001,.F.);
#13923=ORIENTED_EDGE('',*,*,#9979,.F.);
#13924=ORIENTED_EDGE('',*,*,#9969,.F.);
#13925=ORIENTED_EDGE('',*,*,#10002,.T.);
#13926=ORIENTED_EDGE('',*,*,#10003,.F.);
#13927=ORIENTED_EDGE('',*,*,#10004,.F.);
#13928=ORIENTED_EDGE('',*,*,#10005,.T.);
#13929=ORIENTED_EDGE('',*,*,#10006,.T.);
#13930=ORIENTED_EDGE('',*,*,#10007,.T.);
#13931=ORIENTED_EDGE('',*,*,#10006,.F.);
#13932=ORIENTED_EDGE('',*,*,#10008,.T.);
#13933=ORIENTED_EDGE('',*,*,#9964,.T.);
#13934=ORIENTED_EDGE('',*,*,#9955,.F.);
#13935=ORIENTED_EDGE('',*,*,#9958,.F.);
#13936=ORIENTED_EDGE('',*,*,#10009,.F.);
#13937=ORIENTED_EDGE('',*,*,#10010,.F.);
#13938=ORIENTED_EDGE('',*,*,#10011,.T.);
#13939=ORIENTED_EDGE('',*,*,#10012,.F.);
#13940=ORIENTED_EDGE('',*,*,#10007,.F.);
#13941=ORIENTED_EDGE('',*,*,#10008,.F.);
#13942=ORIENTED_EDGE('',*,*,#10013,.T.);
#13943=ORIENTED_EDGE('',*,*,#10014,.T.);
#13944=ORIENTED_EDGE('',*,*,#10001,.T.);
#13945=ORIENTED_EDGE('',*,*,#10014,.F.);
#13946=ORIENTED_EDGE('',*,*,#10015,.T.);
#13947=ORIENTED_EDGE('',*,*,#9975,.F.);
#13948=ORIENTED_EDGE('',*,*,#9980,.T.);
#13949=ORIENTED_EDGE('',*,*,#10015,.F.);
#13950=ORIENTED_EDGE('',*,*,#10016,.T.);
#13951=ORIENTED_EDGE('',*,*,#10017,.T.);
#13952=ORIENTED_EDGE('',*,*,#10018,.T.);
#13953=ORIENTED_EDGE('',*,*,#10019,.F.);
#13954=ORIENTED_EDGE('',*,*,#10020,.F.);
#13955=ORIENTED_EDGE('',*,*,#10021,.F.);
#13956=ORIENTED_EDGE('',*,*,#10016,.F.);
#13957=ORIENTED_EDGE('',*,*,#10013,.F.);
#13958=ORIENTED_EDGE('',*,*,#10005,.F.);
#13959=ORIENTED_EDGE('',*,*,#10022,.T.);
#13960=ORIENTED_EDGE('',*,*,#10023,.T.);
#13961=ORIENTED_EDGE('',*,*,#10024,.T.);
#13962=ORIENTED_EDGE('',*,*,#10025,.T.);
#13963=ORIENTED_EDGE('',*,*,#10026,.T.);
#13964=ORIENTED_EDGE('',*,*,#10024,.F.);
#13965=ORIENTED_EDGE('',*,*,#10019,.T.);
#13966=ORIENTED_EDGE('',*,*,#10004,.T.);
#13967=ORIENTED_EDGE('',*,*,#10023,.F.);
#13968=ORIENTED_EDGE('',*,*,#10027,.T.);
#13969=ORIENTED_EDGE('',*,*,#10028,.T.);
#13970=ORIENTED_EDGE('',*,*,#10029,.T.);
#13971=ORIENTED_EDGE('',*,*,#10020,.T.);
#13972=ORIENTED_EDGE('',*,*,#10022,.F.);
#13973=ORIENTED_EDGE('',*,*,#10030,.T.);
#13974=ORIENTED_EDGE('',*,*,#10031,.T.);
#13975=ORIENTED_EDGE('',*,*,#10032,.T.);
#13976=ORIENTED_EDGE('',*,*,#10025,.F.);
#13977=ORIENTED_EDGE('',*,*,#10033,.T.);
#13978=ORIENTED_EDGE('',*,*,#10034,.T.);
#13979=ORIENTED_EDGE('',*,*,#10035,.T.);
#13980=ORIENTED_EDGE('',*,*,#10036,.T.);
#13981=ORIENTED_EDGE('',*,*,#10037,.T.);
#13982=ORIENTED_EDGE('',*,*,#10002,.F.);
#13983=ORIENTED_EDGE('',*,*,#10012,.T.);
#13984=ORIENTED_EDGE('',*,*,#10038,.T.);
#13985=ORIENTED_EDGE('',*,*,#10036,.F.);
#13986=ORIENTED_EDGE('',*,*,#10039,.T.);
#13987=ORIENTED_EDGE('',*,*,#10034,.F.);
#13988=ORIENTED_EDGE('',*,*,#10035,.F.);
#13989=ORIENTED_EDGE('',*,*,#10040,.F.);
#13990=ORIENTED_EDGE('',*,*,#10041,.F.);
#13991=ORIENTED_EDGE('',*,*,#10030,.F.);
#13992=ORIENTED_EDGE('',*,*,#10039,.F.);
#13993=ORIENTED_EDGE('',*,*,#10042,.T.);
#13994=ORIENTED_EDGE('',*,*,#10043,.F.);
#13995=ORIENTED_EDGE('',*,*,#10040,.T.);
#13996=ORIENTED_EDGE('',*,*,#10038,.F.);
#13997=ORIENTED_EDGE('',*,*,#10011,.F.);
#13998=ORIENTED_EDGE('',*,*,#10044,.F.);
#13999=ORIENTED_EDGE('',*,*,#10042,.F.);
#14000=ORIENTED_EDGE('',*,*,#10000,.F.);
#14001=ORIENTED_EDGE('',*,*,#9992,.T.);
#14002=ORIENTED_EDGE('',*,*,#9997,.F.);
#14003=ORIENTED_EDGE('',*,*,#9974,.F.);
#14004=ORIENTED_EDGE('',*,*,#10045,.T.);
#14005=ORIENTED_EDGE('',*,*,#10046,.T.);
#14006=ORIENTED_EDGE('',*,*,#10047,.T.);
#14007=ORIENTED_EDGE('',*,*,#9995,.F.);
#14008=ORIENTED_EDGE('',*,*,#10047,.F.);
#14009=ORIENTED_EDGE('',*,*,#10048,.F.);
#14010=ORIENTED_EDGE('',*,*,#10049,.F.);
#14011=ORIENTED_EDGE('',*,*,#10050,.F.);
#14012=ORIENTED_EDGE('',*,*,#10051,.F.);
#14013=ORIENTED_EDGE('',*,*,#9960,.F.);
#14014=ORIENTED_EDGE('',*,*,#10051,.T.);
#14015=ORIENTED_EDGE('',*,*,#10052,.T.);
#14016=ORIENTED_EDGE('',*,*,#10053,.T.);
#14017=ORIENTED_EDGE('',*,*,#10054,.F.);
#14018=ORIENTED_EDGE('',*,*,#10009,.T.);
#14019=ORIENTED_EDGE('',*,*,#10055,.T.);
#14020=ORIENTED_EDGE('',*,*,#10044,.T.);
#14021=ORIENTED_EDGE('',*,*,#10010,.T.);
#14022=ORIENTED_EDGE('',*,*,#10054,.T.);
#14023=ORIENTED_EDGE('',*,*,#10056,.T.);
#14024=ORIENTED_EDGE('',*,*,#10057,.T.);
#14025=ORIENTED_EDGE('',*,*,#10043,.T.);
#14026=ORIENTED_EDGE('',*,*,#10055,.F.);
#14027=ORIENTED_EDGE('',*,*,#10058,.F.);
#14028=ORIENTED_EDGE('',*,*,#10041,.T.);
#14029=ORIENTED_EDGE('',*,*,#10057,.F.);
#14030=ORIENTED_EDGE('',*,*,#10059,.T.);
#14031=ORIENTED_EDGE('',*,*,#10032,.F.);
#14032=ORIENTED_EDGE('',*,*,#10060,.F.);
#14033=ORIENTED_EDGE('',*,*,#10061,.F.);
#14034=ORIENTED_EDGE('',*,*,#10062,.F.);
#14035=ORIENTED_EDGE('',*,*,#10063,.T.);
#14036=ORIENTED_EDGE('',*,*,#10027,.F.);
#14037=ORIENTED_EDGE('',*,*,#10026,.F.);
#14038=ORIENTED_EDGE('',*,*,#10003,.T.);
#14039=ORIENTED_EDGE('',*,*,#10037,.F.);
#14040=ORIENTED_EDGE('',*,*,#10033,.F.);
#14041=ORIENTED_EDGE('',*,*,#10064,.T.);
#14042=ORIENTED_EDGE('',*,*,#10065,.T.);
#14043=ORIENTED_EDGE('',*,*,#10052,.F.);
#14044=ORIENTED_EDGE('',*,*,#10050,.T.);
#14045=ORIENTED_EDGE('',*,*,#10064,.F.);
#14046=ORIENTED_EDGE('',*,*,#10066,.T.);
#14047=ORIENTED_EDGE('',*,*,#10031,.F.);
#14048=ORIENTED_EDGE('',*,*,#10058,.T.);
#14049=ORIENTED_EDGE('',*,*,#10066,.F.);
#14050=ORIENTED_EDGE('',*,*,#10049,.T.);
#14051=ORIENTED_EDGE('',*,*,#10067,.F.);
#14052=ORIENTED_EDGE('',*,*,#10068,.F.);
#14053=ORIENTED_EDGE('',*,*,#10060,.T.);
#14054=ORIENTED_EDGE('',*,*,#10056,.F.);
#14055=ORIENTED_EDGE('',*,*,#10053,.F.);
#14056=ORIENTED_EDGE('',*,*,#10065,.F.);
#14057=ORIENTED_EDGE('',*,*,#10059,.F.);
#14058=ORIENTED_EDGE('',*,*,#10069,.T.);
#14059=ORIENTED_EDGE('',*,*,#10070,.T.);
#14060=ORIENTED_EDGE('',*,*,#10071,.T.);
#14061=ORIENTED_EDGE('',*,*,#10072,.T.);
#14062=ORIENTED_EDGE('',*,*,#10073,.T.);
#14063=ORIENTED_EDGE('',*,*,#10074,.T.);
#14064=ORIENTED_EDGE('',*,*,#10075,.T.);
#14065=ORIENTED_EDGE('',*,*,#10076,.T.);
#14066=ORIENTED_EDGE('',*,*,#10077,.F.);
#14067=ORIENTED_EDGE('',*,*,#10078,.T.);
#14068=ORIENTED_EDGE('',*,*,#10075,.F.);
#14069=ORIENTED_EDGE('',*,*,#10079,.T.);
#14070=ORIENTED_EDGE('',*,*,#10070,.F.);
#14071=ORIENTED_EDGE('',*,*,#10080,.F.);
#14072=ORIENTED_EDGE('',*,*,#10081,.F.);
#14073=ORIENTED_EDGE('',*,*,#10082,.F.);
#14074=ORIENTED_EDGE('',*,*,#10076,.F.);
#14075=ORIENTED_EDGE('',*,*,#10083,.F.);
#14076=ORIENTED_EDGE('',*,*,#10084,.F.);
#14077=ORIENTED_EDGE('',*,*,#10085,.F.);
#14078=ORIENTED_EDGE('',*,*,#10086,.T.);
#14079=ORIENTED_EDGE('',*,*,#10085,.T.);
#14080=ORIENTED_EDGE('',*,*,#10087,.T.);
#14081=ORIENTED_EDGE('',*,*,#10088,.T.);
#14082=ORIENTED_EDGE('',*,*,#10086,.F.);
#14083=ORIENTED_EDGE('',*,*,#10089,.T.);
#14084=ORIENTED_EDGE('',*,*,#10069,.F.);
#14085=ORIENTED_EDGE('',*,*,#10073,.F.);
#14086=ORIENTED_EDGE('',*,*,#10090,.T.);
#14087=ORIENTED_EDGE('',*,*,#10091,.T.);
#14088=ORIENTED_EDGE('',*,*,#10092,.T.);
#14089=ORIENTED_EDGE('',*,*,#10084,.T.);
#14090=ORIENTED_EDGE('',*,*,#10092,.F.);
#14091=ORIENTED_EDGE('',*,*,#10093,.T.);
#14092=ORIENTED_EDGE('',*,*,#10087,.F.);
#14093=ORIENTED_EDGE('',*,*,#10078,.F.);
#14094=ORIENTED_EDGE('',*,*,#10094,.T.);
#14095=ORIENTED_EDGE('',*,*,#10095,.T.);
#14096=ORIENTED_EDGE('',*,*,#10083,.T.);
#14097=ORIENTED_EDGE('',*,*,#10095,.F.);
#14098=ORIENTED_EDGE('',*,*,#10096,.T.);
#14099=ORIENTED_EDGE('',*,*,#10090,.F.);
#14100=ORIENTED_EDGE('',*,*,#10089,.F.);
#14101=ORIENTED_EDGE('',*,*,#10097,.T.);
#14102=ORIENTED_EDGE('',*,*,#10098,.T.);
#14103=ORIENTED_EDGE('',*,*,#10080,.T.);
#14104=ORIENTED_EDGE('',*,*,#10088,.F.);
#14105=ORIENTED_EDGE('',*,*,#10099,.F.);
#14106=ORIENTED_EDGE('',*,*,#10100,.F.);
#14107=ORIENTED_EDGE('',*,*,#10097,.F.);
#14108=ORIENTED_EDGE('',*,*,#10093,.F.);
#14109=ORIENTED_EDGE('',*,*,#10101,.T.);
#14110=ORIENTED_EDGE('',*,*,#10102,.F.);
#14111=ORIENTED_EDGE('',*,*,#10099,.T.);
#14112=ORIENTED_EDGE('',*,*,#10091,.F.);
#14113=ORIENTED_EDGE('',*,*,#10103,.F.);
#14114=ORIENTED_EDGE('',*,*,#10104,.F.);
#14115=ORIENTED_EDGE('',*,*,#10101,.F.);
#14116=ORIENTED_EDGE('',*,*,#10096,.F.);
#14117=ORIENTED_EDGE('',*,*,#10105,.T.);
#14118=ORIENTED_EDGE('',*,*,#10106,.F.);
#14119=ORIENTED_EDGE('',*,*,#10103,.T.);
#14120=ORIENTED_EDGE('',*,*,#10094,.F.);
#14121=ORIENTED_EDGE('',*,*,#10107,.F.);
#14122=ORIENTED_EDGE('',*,*,#10108,.F.);
#14123=ORIENTED_EDGE('',*,*,#10105,.F.);
#14124=ORIENTED_EDGE('',*,*,#10077,.T.);
#14125=ORIENTED_EDGE('',*,*,#10109,.T.);
#14126=ORIENTED_EDGE('',*,*,#10110,.T.);
#14127=ORIENTED_EDGE('',*,*,#10107,.T.);
#14128=ORIENTED_EDGE('',*,*,#10111,.T.);
#14129=ORIENTED_EDGE('',*,*,#10112,.T.);
#14130=ORIENTED_EDGE('',*,*,#10113,.T.);
#14131=ORIENTED_EDGE('',*,*,#10114,.T.);
#14132=ORIENTED_EDGE('',*,*,#10115,.F.);
#14133=ORIENTED_EDGE('',*,*,#10116,.T.);
#14134=ORIENTED_EDGE('',*,*,#10117,.T.);
#14135=ORIENTED_EDGE('',*,*,#10118,.T.);
#14136=ORIENTED_EDGE('',*,*,#10119,.F.);
#14137=ORIENTED_EDGE('',*,*,#10117,.F.);
#14138=ORIENTED_EDGE('',*,*,#10120,.T.);
#14139=ORIENTED_EDGE('',*,*,#10111,.F.);
#14140=ORIENTED_EDGE('',*,*,#10112,.F.);
#14141=ORIENTED_EDGE('',*,*,#10121,.F.);
#14142=ORIENTED_EDGE('',*,*,#10122,.F.);
#14143=ORIENTED_EDGE('',*,*,#10123,.F.);
#14144=ORIENTED_EDGE('',*,*,#10120,.F.);
#14145=ORIENTED_EDGE('',*,*,#10124,.T.);
#14146=ORIENTED_EDGE('',*,*,#10125,.T.);
#14147=ORIENTED_EDGE('',*,*,#10121,.T.);
#14148=ORIENTED_EDGE('',*,*,#10116,.F.);
#14149=ORIENTED_EDGE('',*,*,#10126,.F.);
#14150=ORIENTED_EDGE('',*,*,#10127,.F.);
#14151=ORIENTED_EDGE('',*,*,#10128,.T.);
#14152=ORIENTED_EDGE('',*,*,#10129,.F.);
#14153=ORIENTED_EDGE('',*,*,#10124,.F.);
#14154=ORIENTED_EDGE('',*,*,#10125,.F.);
#14155=ORIENTED_EDGE('',*,*,#10130,.T.);
#14156=ORIENTED_EDGE('',*,*,#10131,.T.);
#14157=ORIENTED_EDGE('',*,*,#10072,.F.);
#14158=ORIENTED_EDGE('',*,*,#10132,.F.);
#14159=ORIENTED_EDGE('',*,*,#10118,.F.);
#14160=ORIENTED_EDGE('',*,*,#10114,.F.);
#14161=ORIENTED_EDGE('',*,*,#10133,.F.);
#14162=ORIENTED_EDGE('',*,*,#10074,.F.);
#14163=ORIENTED_EDGE('',*,*,#10130,.F.);
#14164=ORIENTED_EDGE('',*,*,#10129,.T.);
#14165=ORIENTED_EDGE('',*,*,#10134,.T.);
#14166=ORIENTED_EDGE('',*,*,#10135,.T.);
#14167=ORIENTED_EDGE('',*,*,#10136,.T.);
#14168=ORIENTED_EDGE('',*,*,#10131,.F.);
#14169=ORIENTED_EDGE('',*,*,#10137,.T.);
#14170=ORIENTED_EDGE('',*,*,#10138,.T.);
#14171=ORIENTED_EDGE('',*,*,#10122,.T.);
#14172=ORIENTED_EDGE('',*,*,#10139,.T.);
#14173=ORIENTED_EDGE('',*,*,#10108,.T.);
#14174=ORIENTED_EDGE('',*,*,#10140,.F.);
#14175=ORIENTED_EDGE('',*,*,#10141,.T.);
#14176=ORIENTED_EDGE('',*,*,#10142,.T.);
#14177=ORIENTED_EDGE('',*,*,#10104,.T.);
#14178=ORIENTED_EDGE('',*,*,#10143,.T.);
#14179=ORIENTED_EDGE('',*,*,#10144,.T.);
#14180=ORIENTED_EDGE('',*,*,#10145,.T.);
#14181=ORIENTED_EDGE('',*,*,#10102,.T.);
#14182=ORIENTED_EDGE('',*,*,#10142,.F.);
#14183=ORIENTED_EDGE('',*,*,#10146,.T.);
#14184=ORIENTED_EDGE('',*,*,#10100,.T.);
#14185=ORIENTED_EDGE('',*,*,#10145,.F.);
#14186=ORIENTED_EDGE('',*,*,#10147,.T.);
#14187=ORIENTED_EDGE('',*,*,#10143,.F.);
#14188=ORIENTED_EDGE('',*,*,#10106,.T.);
#14189=ORIENTED_EDGE('',*,*,#10139,.F.);
#14190=ORIENTED_EDGE('',*,*,#10147,.F.);
#14191=ORIENTED_EDGE('',*,*,#10144,.F.);
#14192=ORIENTED_EDGE('',*,*,#10141,.F.);
#14193=ORIENTED_EDGE('',*,*,#10148,.F.);
#14194=ORIENTED_EDGE('',*,*,#10109,.F.);
#14195=ORIENTED_EDGE('',*,*,#10149,.F.);
#14196=ORIENTED_EDGE('',*,*,#10123,.T.);
#14197=ORIENTED_EDGE('',*,*,#10150,.F.);
#14198=ORIENTED_EDGE('',*,*,#10079,.F.);
#14199=ORIENTED_EDGE('',*,*,#10133,.T.);
#14200=ORIENTED_EDGE('',*,*,#10113,.F.);
#14201=ORIENTED_EDGE('',*,*,#10149,.T.);
#14202=ORIENTED_EDGE('',*,*,#10151,.T.);
#14203=ORIENTED_EDGE('',*,*,#10150,.T.);
#14204=ORIENTED_EDGE('',*,*,#10138,.F.);
#14205=ORIENTED_EDGE('',*,*,#10152,.T.);
#14206=ORIENTED_EDGE('',*,*,#10151,.F.);
#14207=ORIENTED_EDGE('',*,*,#10153,.T.);
#14208=ORIENTED_EDGE('',*,*,#10140,.T.);
#14209=ORIENTED_EDGE('',*,*,#10110,.F.);
#14210=ORIENTED_EDGE('',*,*,#10153,.F.);
#14211=ORIENTED_EDGE('',*,*,#10154,.T.);
#14212=ORIENTED_EDGE('',*,*,#10155,.T.);
#14213=ORIENTED_EDGE('',*,*,#10148,.T.);
#14214=ORIENTED_EDGE('',*,*,#10136,.F.);
#14215=ORIENTED_EDGE('',*,*,#10156,.F.);
#14216=ORIENTED_EDGE('',*,*,#10157,.F.);
#14217=ORIENTED_EDGE('',*,*,#10154,.F.);
#14218=ORIENTED_EDGE('',*,*,#10152,.F.);
#14219=ORIENTED_EDGE('',*,*,#10137,.F.);
#14220=ORIENTED_EDGE('',*,*,#10155,.F.);
#14221=ORIENTED_EDGE('',*,*,#10158,.T.);
#14222=ORIENTED_EDGE('',*,*,#10098,.F.);
#14223=ORIENTED_EDGE('',*,*,#10146,.F.);
#14224=ORIENTED_EDGE('',*,*,#10158,.F.);
#14225=ORIENTED_EDGE('',*,*,#10157,.T.);
#14226=ORIENTED_EDGE('',*,*,#10159,.T.);
#14227=ORIENTED_EDGE('',*,*,#10081,.T.);
#14228=ORIENTED_EDGE('',*,*,#10160,.F.);
#14229=ORIENTED_EDGE('',*,*,#10161,.T.);
#14230=ORIENTED_EDGE('',*,*,#10162,.T.);
#14231=ORIENTED_EDGE('',*,*,#10163,.T.);
#14232=ORIENTED_EDGE('',*,*,#10164,.F.);
#14233=ORIENTED_EDGE('',*,*,#10165,.T.);
#14234=ORIENTED_EDGE('',*,*,#10166,.T.);
#14235=ORIENTED_EDGE('',*,*,#10167,.T.);
#14236=ORIENTED_EDGE('',*,*,#10168,.T.);
#14237=ORIENTED_EDGE('',*,*,#10169,.T.);
#14238=ORIENTED_EDGE('',*,*,#10167,.F.);
#14239=ORIENTED_EDGE('',*,*,#10170,.T.);
#14240=ORIENTED_EDGE('',*,*,#10162,.F.);
#14241=ORIENTED_EDGE('',*,*,#10163,.F.);
#14242=ORIENTED_EDGE('',*,*,#10171,.F.);
#14243=ORIENTED_EDGE('',*,*,#10172,.F.);
#14244=ORIENTED_EDGE('',*,*,#10173,.F.);
#14245=ORIENTED_EDGE('',*,*,#10170,.F.);
#14246=ORIENTED_EDGE('',*,*,#10174,.T.);
#14247=ORIENTED_EDGE('',*,*,#10175,.F.);
#14248=ORIENTED_EDGE('',*,*,#10176,.F.);
#14249=ORIENTED_EDGE('',*,*,#10171,.T.);
#14250=ORIENTED_EDGE('',*,*,#10166,.F.);
#14251=ORIENTED_EDGE('',*,*,#10177,.F.);
#14252=ORIENTED_EDGE('',*,*,#10178,.F.);
#14253=ORIENTED_EDGE('',*,*,#10174,.F.);
#14254=ORIENTED_EDGE('',*,*,#10165,.F.);
#14255=ORIENTED_EDGE('',*,*,#10179,.F.);
#14256=ORIENTED_EDGE('',*,*,#10180,.T.);
#14257=ORIENTED_EDGE('',*,*,#10181,.T.);
#14258=ORIENTED_EDGE('',*,*,#10177,.T.);
#14259=ORIENTED_EDGE('',*,*,#10169,.F.);
#14260=ORIENTED_EDGE('',*,*,#10182,.T.);
#14261=ORIENTED_EDGE('',*,*,#10183,.T.);
#14262=ORIENTED_EDGE('',*,*,#10184,.F.);
#14263=ORIENTED_EDGE('',*,*,#10185,.T.);
#14264=ORIENTED_EDGE('',*,*,#10179,.T.);
#14265=ORIENTED_EDGE('',*,*,#10186,.T.);
#14266=ORIENTED_EDGE('',*,*,#10187,.T.);
#14267=ORIENTED_EDGE('',*,*,#10188,.T.);
#14268=ORIENTED_EDGE('',*,*,#10189,.T.);
#14269=ORIENTED_EDGE('',*,*,#10190,.F.);
#14270=ORIENTED_EDGE('',*,*,#10191,.T.);
#14271=ORIENTED_EDGE('',*,*,#10188,.F.);
#14272=ORIENTED_EDGE('',*,*,#10192,.T.);
#14273=ORIENTED_EDGE('',*,*,#10193,.T.);
#14274=ORIENTED_EDGE('',*,*,#10194,.T.);
#14275=ORIENTED_EDGE('',*,*,#10186,.F.);
#14276=ORIENTED_EDGE('',*,*,#10195,.T.);
#14277=ORIENTED_EDGE('',*,*,#10194,.F.);
#14278=ORIENTED_EDGE('',*,*,#10196,.T.);
#14279=ORIENTED_EDGE('',*,*,#10197,.T.);
#14280=ORIENTED_EDGE('',*,*,#10198,.T.);
#14281=ORIENTED_EDGE('',*,*,#10193,.F.);
#14282=ORIENTED_EDGE('',*,*,#10199,.T.);
#14283=ORIENTED_EDGE('',*,*,#10200,.F.);
#14284=ORIENTED_EDGE('',*,*,#10201,.T.);
#14285=ORIENTED_EDGE('',*,*,#10195,.F.);
#14286=ORIENTED_EDGE('',*,*,#10202,.T.);
#14287=ORIENTED_EDGE('',*,*,#10203,.T.);
#14288=ORIENTED_EDGE('',*,*,#10204,.T.);
#14289=ORIENTED_EDGE('',*,*,#10189,.F.);
#14290=ORIENTED_EDGE('',*,*,#10205,.F.);
#14291=ORIENTED_EDGE('',*,*,#10206,.F.);
#14292=ORIENTED_EDGE('',*,*,#10202,.F.);
#14293=ORIENTED_EDGE('',*,*,#10191,.F.);
#14294=ORIENTED_EDGE('',*,*,#10207,.T.);
#14295=ORIENTED_EDGE('',*,*,#10208,.T.);
#14296=ORIENTED_EDGE('',*,*,#10205,.T.);
#14297=ORIENTED_EDGE('',*,*,#10209,.T.);
#14298=ORIENTED_EDGE('',*,*,#10210,.T.);
#14299=ORIENTED_EDGE('',*,*,#10211,.T.);
#14300=ORIENTED_EDGE('',*,*,#10212,.T.);
#14301=ORIENTED_EDGE('',*,*,#10213,.T.);
#14302=ORIENTED_EDGE('',*,*,#10214,.T.);
#14303=ORIENTED_EDGE('',*,*,#10209,.F.);
#14304=ORIENTED_EDGE('',*,*,#10211,.F.);
#14305=ORIENTED_EDGE('',*,*,#10215,.T.);
#14306=ORIENTED_EDGE('',*,*,#10208,.F.);
#14307=ORIENTED_EDGE('',*,*,#10216,.T.);
#14308=ORIENTED_EDGE('',*,*,#10217,.T.);
#14309=ORIENTED_EDGE('',*,*,#10213,.F.);
#14310=ORIENTED_EDGE('',*,*,#10218,.T.);
#14311=ORIENTED_EDGE('',*,*,#10219,.T.);
#14312=ORIENTED_EDGE('',*,*,#10215,.F.);
#14313=ORIENTED_EDGE('',*,*,#10220,.T.);
#14314=ORIENTED_EDGE('',*,*,#10221,.T.);
#14315=ORIENTED_EDGE('',*,*,#10206,.T.);
#14316=ORIENTED_EDGE('',*,*,#10210,.F.);
#14317=ORIENTED_EDGE('',*,*,#10222,.F.);
#14318=ORIENTED_EDGE('',*,*,#10223,.F.);
#14319=ORIENTED_EDGE('',*,*,#10220,.F.);
#14320=ORIENTED_EDGE('',*,*,#10214,.F.);
#14321=ORIENTED_EDGE('',*,*,#10224,.T.);
#14322=ORIENTED_EDGE('',*,*,#10225,.F.);
#14323=ORIENTED_EDGE('',*,*,#10222,.T.);
#14324=ORIENTED_EDGE('',*,*,#10217,.F.);
#14325=ORIENTED_EDGE('',*,*,#10226,.F.);
#14326=ORIENTED_EDGE('',*,*,#10227,.F.);
#14327=ORIENTED_EDGE('',*,*,#10224,.F.);
#14328=ORIENTED_EDGE('',*,*,#10216,.F.);
#14329=ORIENTED_EDGE('',*,*,#10228,.F.);
#14330=ORIENTED_EDGE('',*,*,#10229,.F.);
#14331=ORIENTED_EDGE('',*,*,#10190,.T.);
#14332=ORIENTED_EDGE('',*,*,#10230,.T.);
#14333=ORIENTED_EDGE('',*,*,#10228,.T.);
#14334=ORIENTED_EDGE('',*,*,#10219,.F.);
#14335=ORIENTED_EDGE('',*,*,#10231,.T.);
#14336=ORIENTED_EDGE('',*,*,#10207,.F.);
#14337=ORIENTED_EDGE('',*,*,#10231,.F.);
#14338=ORIENTED_EDGE('',*,*,#10218,.F.);
#14339=ORIENTED_EDGE('',*,*,#10212,.F.);
#14340=ORIENTED_EDGE('',*,*,#10192,.F.);
#14341=ORIENTED_EDGE('',*,*,#10232,.T.);
#14342=ORIENTED_EDGE('',*,*,#10233,.T.);
#14343=ORIENTED_EDGE('',*,*,#10234,.T.);
#14344=ORIENTED_EDGE('',*,*,#10187,.F.);
#14345=ORIENTED_EDGE('',*,*,#10198,.F.);
#14346=ORIENTED_EDGE('',*,*,#10235,.F.);
#14347=ORIENTED_EDGE('',*,*,#10232,.F.);
#14348=ORIENTED_EDGE('',*,*,#10236,.T.);
#14349=ORIENTED_EDGE('',*,*,#10237,.T.);
#14350=ORIENTED_EDGE('',*,*,#10238,.T.);
#14351=ORIENTED_EDGE('',*,*,#10160,.T.);
#14352=ORIENTED_EDGE('',*,*,#10239,.T.);
#14353=ORIENTED_EDGE('',*,*,#10229,.T.);
#14354=ORIENTED_EDGE('',*,*,#10236,.F.);
#14355=ORIENTED_EDGE('',*,*,#10240,.T.);
#14356=ORIENTED_EDGE('',*,*,#10240,.F.);
#14357=ORIENTED_EDGE('',*,*,#10241,.T.);
#14358=ORIENTED_EDGE('',*,*,#10242,.F.);
#14359=ORIENTED_EDGE('',*,*,#10226,.T.);
#14360=ORIENTED_EDGE('',*,*,#10239,.F.);
#14361=ORIENTED_EDGE('',*,*,#10164,.T.);
#14362=ORIENTED_EDGE('',*,*,#10173,.T.);
#14363=ORIENTED_EDGE('',*,*,#10243,.F.);
#14364=ORIENTED_EDGE('',*,*,#10244,.F.);
#14365=ORIENTED_EDGE('',*,*,#10241,.F.);
#14366=ORIENTED_EDGE('',*,*,#10230,.F.);
#14367=ORIENTED_EDGE('',*,*,#10234,.F.);
#14368=ORIENTED_EDGE('',*,*,#10245,.F.);
#14369=ORIENTED_EDGE('',*,*,#10183,.F.);
#14370=ORIENTED_EDGE('',*,*,#10246,.F.);
#14371=ORIENTED_EDGE('',*,*,#10237,.F.);
#14372=ORIENTED_EDGE('',*,*,#10161,.F.);
#14373=ORIENTED_EDGE('',*,*,#10238,.F.);
#14374=ORIENTED_EDGE('',*,*,#10246,.T.);
#14375=ORIENTED_EDGE('',*,*,#10182,.F.);
#14376=ORIENTED_EDGE('',*,*,#10168,.F.);
#14377=ORIENTED_EDGE('',*,*,#10247,.T.);
#14378=ORIENTED_EDGE('',*,*,#10248,.T.);
#14379=ORIENTED_EDGE('',*,*,#10249,.T.);
#14380=ORIENTED_EDGE('',*,*,#10250,.T.);
#14381=ORIENTED_EDGE('',*,*,#10251,.F.);
#14382=ORIENTED_EDGE('',*,*,#10248,.F.);
#14383=ORIENTED_EDGE('',*,*,#10252,.F.);
#14384=ORIENTED_EDGE('',*,*,#10253,.F.);
#14385=ORIENTED_EDGE('',*,*,#10196,.F.);
#14386=ORIENTED_EDGE('',*,*,#10201,.F.);
#14387=ORIENTED_EDGE('',*,*,#10247,.F.);
#14388=ORIENTED_EDGE('',*,*,#10254,.T.);
#14389=ORIENTED_EDGE('',*,*,#10255,.T.);
#14390=ORIENTED_EDGE('',*,*,#10175,.T.);
#14391=ORIENTED_EDGE('',*,*,#10178,.T.);
#14392=ORIENTED_EDGE('',*,*,#10256,.F.);
#14393=ORIENTED_EDGE('',*,*,#10256,.T.);
#14394=ORIENTED_EDGE('',*,*,#10181,.F.);
#14395=ORIENTED_EDGE('',*,*,#10257,.T.);
#14396=ORIENTED_EDGE('',*,*,#10255,.F.);
#14397=ORIENTED_EDGE('',*,*,#10258,.T.);
#14398=ORIENTED_EDGE('',*,*,#10259,.T.);
#14399=ORIENTED_EDGE('',*,*,#10243,.T.);
#14400=ORIENTED_EDGE('',*,*,#10172,.T.);
#14401=ORIENTED_EDGE('',*,*,#10176,.T.);
#14402=ORIENTED_EDGE('',*,*,#10221,.F.);
#14403=ORIENTED_EDGE('',*,*,#10260,.T.);
#14404=ORIENTED_EDGE('',*,*,#10203,.F.);
#14405=ORIENTED_EDGE('',*,*,#10257,.F.);
#14406=ORIENTED_EDGE('',*,*,#10261,.T.);
#14407=ORIENTED_EDGE('',*,*,#10262,.T.);
#14408=ORIENTED_EDGE('',*,*,#10263,.T.);
#14409=ORIENTED_EDGE('',*,*,#10252,.T.);
#14410=ORIENTED_EDGE('',*,*,#10250,.F.);
#14411=ORIENTED_EDGE('',*,*,#10264,.F.);
#14412=ORIENTED_EDGE('',*,*,#10258,.F.);
#14413=ORIENTED_EDGE('',*,*,#10254,.F.);
#14414=ORIENTED_EDGE('',*,*,#10265,.T.);
#14415=ORIENTED_EDGE('',*,*,#10227,.T.);
#14416=ORIENTED_EDGE('',*,*,#10266,.T.);
#14417=ORIENTED_EDGE('',*,*,#10267,.T.);
#14418=ORIENTED_EDGE('',*,*,#10268,.T.);
#14419=ORIENTED_EDGE('',*,*,#10200,.T.);
#14420=ORIENTED_EDGE('',*,*,#10266,.F.);
#14421=ORIENTED_EDGE('',*,*,#10242,.T.);
#14422=ORIENTED_EDGE('',*,*,#10264,.T.);
#14423=ORIENTED_EDGE('',*,*,#10249,.F.);
#14424=ORIENTED_EDGE('',*,*,#10251,.T.);
#14425=ORIENTED_EDGE('',*,*,#10268,.F.);
#14426=ORIENTED_EDGE('',*,*,#10244,.T.);
#14427=ORIENTED_EDGE('',*,*,#10259,.F.);
#14428=ORIENTED_EDGE('',*,*,#10260,.F.);
#14429=ORIENTED_EDGE('',*,*,#10223,.T.);
#14430=ORIENTED_EDGE('',*,*,#10269,.T.);
#14431=ORIENTED_EDGE('',*,*,#10270,.T.);
#14432=ORIENTED_EDGE('',*,*,#10269,.F.);
#14433=ORIENTED_EDGE('',*,*,#10225,.T.);
#14434=ORIENTED_EDGE('',*,*,#10265,.F.);
#14435=ORIENTED_EDGE('',*,*,#10204,.F.);
#14436=ORIENTED_EDGE('',*,*,#10270,.F.);
#14437=ORIENTED_EDGE('',*,*,#10267,.F.);
#14438=ORIENTED_EDGE('',*,*,#10199,.F.);
#14439=ORIENTED_EDGE('',*,*,#10271,.T.);
#14440=ORIENTED_EDGE('',*,*,#10272,.T.);
#14441=ORIENTED_EDGE('',*,*,#10273,.T.);
#14442=ORIENTED_EDGE('',*,*,#10272,.F.);
#14443=ORIENTED_EDGE('',*,*,#10274,.T.);
#14444=ORIENTED_EDGE('',*,*,#10271,.F.);
#14445=ORIENTED_EDGE('',*,*,#10275,.T.);
#14446=ORIENTED_EDGE('',*,*,#10276,.F.);
#14447=ORIENTED_EDGE('',*,*,#10277,.F.);
#14448=ORIENTED_EDGE('',*,*,#10278,.T.);
#14449=ORIENTED_EDGE('',*,*,#10279,.F.);
#14450=ORIENTED_EDGE('',*,*,#10280,.F.);
#14451=ORIENTED_EDGE('',*,*,#10281,.F.);
#14452=ORIENTED_EDGE('',*,*,#10282,.T.);
#14453=ORIENTED_EDGE('',*,*,#10283,.F.);
#14454=ORIENTED_EDGE('',*,*,#10284,.F.);
#14455=ORIENTED_EDGE('',*,*,#10285,.F.);
#14456=ORIENTED_EDGE('',*,*,#10286,.T.);
#14457=ORIENTED_EDGE('',*,*,#10287,.F.);
#14458=ORIENTED_EDGE('',*,*,#10288,.F.);
#14459=ORIENTED_EDGE('',*,*,#10289,.F.);
#14460=ORIENTED_EDGE('',*,*,#10290,.T.);
#14461=ORIENTED_EDGE('',*,*,#10291,.F.);
#14462=ORIENTED_EDGE('',*,*,#10292,.F.);
#14463=ORIENTED_EDGE('',*,*,#10275,.F.);
#14464=ORIENTED_EDGE('',*,*,#10274,.F.);
#14465=ORIENTED_EDGE('',*,*,#10273,.F.);
#14466=ORIENTED_EDGE('',*,*,#10293,.F.);
#14467=ORIENTED_EDGE('',*,*,#10294,.T.);
#14468=ORIENTED_EDGE('',*,*,#10295,.T.);
#14469=ORIENTED_EDGE('',*,*,#10296,.T.);
#14470=ORIENTED_EDGE('',*,*,#10297,.T.);
#14471=ORIENTED_EDGE('',*,*,#10298,.T.);
#14472=ORIENTED_EDGE('',*,*,#10299,.T.);
#14473=ORIENTED_EDGE('',*,*,#10300,.T.);
#14474=ORIENTED_EDGE('',*,*,#10296,.F.);
#14475=ORIENTED_EDGE('',*,*,#10301,.T.);
#14476=ORIENTED_EDGE('',*,*,#10302,.T.);
#14477=ORIENTED_EDGE('',*,*,#10303,.T.);
#14478=ORIENTED_EDGE('',*,*,#10299,.F.);
#14479=ORIENTED_EDGE('',*,*,#10304,.T.);
#14480=ORIENTED_EDGE('',*,*,#10305,.T.);
#14481=ORIENTED_EDGE('',*,*,#10306,.T.);
#14482=ORIENTED_EDGE('',*,*,#10302,.F.);
#14483=ORIENTED_EDGE('',*,*,#10307,.T.);
#14484=ORIENTED_EDGE('',*,*,#10308,.T.);
#14485=ORIENTED_EDGE('',*,*,#10309,.F.);
#14486=ORIENTED_EDGE('',*,*,#10309,.T.);
#14487=ORIENTED_EDGE('',*,*,#10310,.T.);
#14488=ORIENTED_EDGE('',*,*,#10311,.T.);
#14489=ORIENTED_EDGE('',*,*,#10307,.F.);
#14490=ORIENTED_EDGE('',*,*,#10312,.T.);
#14491=ORIENTED_EDGE('',*,*,#10305,.F.);
#14492=ORIENTED_EDGE('',*,*,#10313,.T.);
#14493=ORIENTED_EDGE('',*,*,#10297,.F.);
#14494=ORIENTED_EDGE('',*,*,#10300,.F.);
#14495=ORIENTED_EDGE('',*,*,#10303,.F.);
#14496=ORIENTED_EDGE('',*,*,#10314,.F.);
#14497=ORIENTED_EDGE('',*,*,#10315,.F.);
#14498=ORIENTED_EDGE('',*,*,#10316,.F.);
#14499=ORIENTED_EDGE('',*,*,#10317,.F.);
#14500=ORIENTED_EDGE('',*,*,#10318,.F.);
#14501=ORIENTED_EDGE('',*,*,#10319,.F.);
#14502=ORIENTED_EDGE('',*,*,#10320,.F.);
#14503=ORIENTED_EDGE('',*,*,#10321,.F.);
#14504=ORIENTED_EDGE('',*,*,#10322,.F.);
#14505=ORIENTED_EDGE('',*,*,#10323,.F.);
#14506=ORIENTED_EDGE('',*,*,#10324,.F.);
#14507=ORIENTED_EDGE('',*,*,#10325,.F.);
#14508=ORIENTED_EDGE('',*,*,#10326,.F.);
#14509=ORIENTED_EDGE('',*,*,#10327,.F.);
#14510=ORIENTED_EDGE('',*,*,#10306,.F.);
#14511=ORIENTED_EDGE('',*,*,#10328,.T.);
#14512=ORIENTED_EDGE('',*,*,#10329,.T.);
#14513=ORIENTED_EDGE('',*,*,#10314,.T.);
#14514=ORIENTED_EDGE('',*,*,#10312,.F.);
#14515=ORIENTED_EDGE('',*,*,#10330,.F.);
#14516=ORIENTED_EDGE('',*,*,#10331,.F.);
#14517=ORIENTED_EDGE('',*,*,#10328,.F.);
#14518=ORIENTED_EDGE('',*,*,#10311,.F.);
#14519=ORIENTED_EDGE('',*,*,#10284,.T.);
#14520=ORIENTED_EDGE('',*,*,#10332,.T.);
#14521=ORIENTED_EDGE('',*,*,#10330,.T.);
#14522=ORIENTED_EDGE('',*,*,#10308,.F.);
#14523=ORIENTED_EDGE('',*,*,#10333,.T.);
#14524=ORIENTED_EDGE('',*,*,#10334,.F.);
#14525=ORIENTED_EDGE('',*,*,#10335,.F.);
#14526=ORIENTED_EDGE('',*,*,#10285,.T.);
#14527=ORIENTED_EDGE('',*,*,#10310,.F.);
#14528=ORIENTED_EDGE('',*,*,#10336,.T.);
#14529=ORIENTED_EDGE('',*,*,#10337,.T.);
#14530=ORIENTED_EDGE('',*,*,#10338,.T.);
#14531=ORIENTED_EDGE('',*,*,#10323,.T.);
#14532=ORIENTED_EDGE('',*,*,#10339,.T.);
#14533=ORIENTED_EDGE('',*,*,#10340,.T.);
#14534=ORIENTED_EDGE('',*,*,#10324,.T.);
#14535=ORIENTED_EDGE('',*,*,#10338,.F.);
#14536=ORIENTED_EDGE('',*,*,#10341,.T.);
#14537=ORIENTED_EDGE('',*,*,#10342,.T.);
#14538=ORIENTED_EDGE('',*,*,#10325,.T.);
#14539=ORIENTED_EDGE('',*,*,#10340,.F.);
#14540=ORIENTED_EDGE('',*,*,#10343,.T.);
#14541=ORIENTED_EDGE('',*,*,#10344,.T.);
#14542=ORIENTED_EDGE('',*,*,#10339,.F.);
#14543=ORIENTED_EDGE('',*,*,#10322,.T.);
#14544=ORIENTED_EDGE('',*,*,#10345,.T.);
#14545=ORIENTED_EDGE('',*,*,#10346,.T.);
#14546=ORIENTED_EDGE('',*,*,#10298,.F.);
#14547=ORIENTED_EDGE('',*,*,#10326,.T.);
#14548=ORIENTED_EDGE('',*,*,#10342,.F.);
#14549=ORIENTED_EDGE('',*,*,#10347,.T.);
#14550=ORIENTED_EDGE('',*,*,#10348,.T.);
#14551=ORIENTED_EDGE('',*,*,#10295,.F.);
#14552=ORIENTED_EDGE('',*,*,#10349,.F.);
#14553=ORIENTED_EDGE('',*,*,#10350,.F.);
#14554=ORIENTED_EDGE('',*,*,#10351,.F.);
#14555=ORIENTED_EDGE('',*,*,#10352,.F.);
#14556=ORIENTED_EDGE('',*,*,#10353,.T.);
#14557=ORIENTED_EDGE('',*,*,#10354,.F.);
#14558=ORIENTED_EDGE('',*,*,#10294,.F.);
#14559=ORIENTED_EDGE('',*,*,#10348,.F.);
#14560=ORIENTED_EDGE('',*,*,#10355,.F.);
#14561=ORIENTED_EDGE('',*,*,#10356,.F.);
#14562=ORIENTED_EDGE('',*,*,#10349,.T.);
#14563=ORIENTED_EDGE('',*,*,#10344,.F.);
#14564=ORIENTED_EDGE('',*,*,#10357,.T.);
#14565=ORIENTED_EDGE('',*,*,#10358,.F.);
#14566=ORIENTED_EDGE('',*,*,#10359,.F.);
#14567=ORIENTED_EDGE('',*,*,#10289,.T.);
#14568=ORIENTED_EDGE('',*,*,#10360,.T.);
#14569=ORIENTED_EDGE('',*,*,#10355,.T.);
#14570=ORIENTED_EDGE('',*,*,#10347,.F.);
#14571=ORIENTED_EDGE('',*,*,#10361,.T.);
#14572=ORIENTED_EDGE('',*,*,#10362,.T.);
#14573=ORIENTED_EDGE('',*,*,#10363,.T.);
#14574=ORIENTED_EDGE('',*,*,#10364,.T.);
#14575=ORIENTED_EDGE('',*,*,#10345,.F.);
#14576=ORIENTED_EDGE('',*,*,#10365,.T.);
#14577=ORIENTED_EDGE('',*,*,#10363,.F.);
#14578=ORIENTED_EDGE('',*,*,#10366,.F.);
#14579=ORIENTED_EDGE('',*,*,#10277,.T.);
#14580=ORIENTED_EDGE('',*,*,#10367,.T.);
#14581=ORIENTED_EDGE('',*,*,#10368,.T.);
#14582=ORIENTED_EDGE('',*,*,#10369,.T.);
#14583=ORIENTED_EDGE('',*,*,#10370,.F.);
#14584=ORIENTED_EDGE('',*,*,#10367,.F.);
#14585=ORIENTED_EDGE('',*,*,#10371,.T.);
#14586=ORIENTED_EDGE('',*,*,#10361,.F.);
#14587=ORIENTED_EDGE('',*,*,#10368,.F.);
#14588=ORIENTED_EDGE('',*,*,#10372,.T.);
#14589=ORIENTED_EDGE('',*,*,#10372,.F.);
#14590=ORIENTED_EDGE('',*,*,#10337,.F.);
#14591=ORIENTED_EDGE('',*,*,#10373,.F.);
#14592=ORIENTED_EDGE('',*,*,#10374,.F.);
#14593=ORIENTED_EDGE('',*,*,#10375,.F.);
#14594=ORIENTED_EDGE('',*,*,#10376,.F.);
#14595=ORIENTED_EDGE('',*,*,#10377,.T.);
#14596=ORIENTED_EDGE('',*,*,#10378,.F.);
#14597=ORIENTED_EDGE('',*,*,#10336,.F.);
#14598=ORIENTED_EDGE('',*,*,#10346,.F.);
#14599=ORIENTED_EDGE('',*,*,#10362,.F.);
#14600=ORIENTED_EDGE('',*,*,#10379,.F.);
#14601=ORIENTED_EDGE('',*,*,#10373,.T.);
#14602=ORIENTED_EDGE('',*,*,#10371,.F.);
#14603=ORIENTED_EDGE('',*,*,#10276,.T.);
#14604=ORIENTED_EDGE('',*,*,#10292,.T.);
#14605=ORIENTED_EDGE('',*,*,#10380,.T.);
#14606=ORIENTED_EDGE('',*,*,#10374,.T.);
#14607=ORIENTED_EDGE('',*,*,#10379,.T.);
#14608=ORIENTED_EDGE('',*,*,#10291,.T.);
#14609=ORIENTED_EDGE('',*,*,#10381,.T.);
#14610=ORIENTED_EDGE('',*,*,#10375,.T.);
#14611=ORIENTED_EDGE('',*,*,#10380,.F.);
#14612=ORIENTED_EDGE('',*,*,#10343,.F.);
#14613=ORIENTED_EDGE('',*,*,#10382,.T.);
#14614=ORIENTED_EDGE('',*,*,#10383,.T.);
#14615=ORIENTED_EDGE('',*,*,#10357,.F.);
#14616=ORIENTED_EDGE('',*,*,#10360,.F.);
#14617=ORIENTED_EDGE('',*,*,#10288,.T.);
#14618=ORIENTED_EDGE('',*,*,#10384,.T.);
#14619=ORIENTED_EDGE('',*,*,#10350,.T.);
#14620=ORIENTED_EDGE('',*,*,#10356,.T.);
#14621=ORIENTED_EDGE('',*,*,#10287,.T.);
#14622=ORIENTED_EDGE('',*,*,#10385,.T.);
#14623=ORIENTED_EDGE('',*,*,#10351,.T.);
#14624=ORIENTED_EDGE('',*,*,#10384,.F.);
#14625=ORIENTED_EDGE('',*,*,#10304,.F.);
#14626=ORIENTED_EDGE('',*,*,#10386,.T.);
#14627=ORIENTED_EDGE('',*,*,#10387,.T.);
#14628=ORIENTED_EDGE('',*,*,#10333,.F.);
#14629=ORIENTED_EDGE('',*,*,#10313,.F.);
#14630=ORIENTED_EDGE('',*,*,#10388,.T.);
#14631=ORIENTED_EDGE('',*,*,#10331,.T.);
#14632=ORIENTED_EDGE('',*,*,#10389,.T.);
#14633=ORIENTED_EDGE('',*,*,#10390,.T.);
#14634=ORIENTED_EDGE('',*,*,#10388,.F.);
#14635=ORIENTED_EDGE('',*,*,#10391,.T.);
#14636=ORIENTED_EDGE('',*,*,#10329,.F.);
#14637=ORIENTED_EDGE('',*,*,#10332,.F.);
#14638=ORIENTED_EDGE('',*,*,#10392,.T.);
#14639=ORIENTED_EDGE('',*,*,#10389,.F.);
#14640=ORIENTED_EDGE('',*,*,#10391,.F.);
#14641=ORIENTED_EDGE('',*,*,#10393,.T.);
#14642=ORIENTED_EDGE('',*,*,#10394,.T.);
#14643=ORIENTED_EDGE('',*,*,#10315,.T.);
#14644=ORIENTED_EDGE('',*,*,#10390,.F.);
#14645=ORIENTED_EDGE('',*,*,#10395,.F.);
#14646=ORIENTED_EDGE('',*,*,#10396,.F.);
#14647=ORIENTED_EDGE('',*,*,#10397,.T.);
#14648=ORIENTED_EDGE('',*,*,#10398,.F.);
#14649=ORIENTED_EDGE('',*,*,#10393,.F.);
#14650=ORIENTED_EDGE('',*,*,#10392,.F.);
#14651=ORIENTED_EDGE('',*,*,#10283,.T.);
#14652=ORIENTED_EDGE('',*,*,#10399,.T.);
#14653=ORIENTED_EDGE('',*,*,#10395,.T.);
#14654=ORIENTED_EDGE('',*,*,#10400,.T.);
#14655=ORIENTED_EDGE('',*,*,#10279,.T.);
#14656=ORIENTED_EDGE('',*,*,#10401,.T.);
#14657=ORIENTED_EDGE('',*,*,#10402,.T.);
#14658=ORIENTED_EDGE('',*,*,#10403,.T.);
#14659=ORIENTED_EDGE('',*,*,#10404,.T.);
#14660=ORIENTED_EDGE('',*,*,#10405,.T.);
#14661=ORIENTED_EDGE('',*,*,#10406,.T.);
#14662=ORIENTED_EDGE('',*,*,#10403,.F.);
#14663=ORIENTED_EDGE('',*,*,#10407,.T.);
#14664=ORIENTED_EDGE('',*,*,#10408,.T.);
#14665=ORIENTED_EDGE('',*,*,#10405,.F.);
#14666=ORIENTED_EDGE('',*,*,#10409,.T.);
#14667=ORIENTED_EDGE('',*,*,#10400,.F.);
#14668=ORIENTED_EDGE('',*,*,#10409,.F.);
#14669=ORIENTED_EDGE('',*,*,#10410,.T.);
#14670=ORIENTED_EDGE('',*,*,#10411,.T.);
#14671=ORIENTED_EDGE('',*,*,#10280,.T.);
#14672=ORIENTED_EDGE('',*,*,#10404,.F.);
#14673=ORIENTED_EDGE('',*,*,#10412,.F.);
#14674=ORIENTED_EDGE('',*,*,#10413,.F.);
#14675=ORIENTED_EDGE('',*,*,#10410,.F.);
#14676=ORIENTED_EDGE('',*,*,#10414,.T.);
#14677=ORIENTED_EDGE('',*,*,#10415,.T.);
#14678=ORIENTED_EDGE('',*,*,#10401,.F.);
#14679=ORIENTED_EDGE('',*,*,#10278,.F.);
#14680=ORIENTED_EDGE('',*,*,#10366,.T.);
#14681=ORIENTED_EDGE('',*,*,#10414,.F.);
#14682=ORIENTED_EDGE('',*,*,#10370,.T.);
#14683=ORIENTED_EDGE('',*,*,#10416,.F.);
#14684=ORIENTED_EDGE('',*,*,#10417,.F.);
#14685=ORIENTED_EDGE('',*,*,#10418,.F.);
#14686=ORIENTED_EDGE('',*,*,#10419,.F.);
#14687=ORIENTED_EDGE('',*,*,#10411,.F.);
#14688=ORIENTED_EDGE('',*,*,#10420,.F.);
#14689=ORIENTED_EDGE('',*,*,#10421,.F.);
#14690=ORIENTED_EDGE('',*,*,#10420,.T.);
#14691=ORIENTED_EDGE('',*,*,#10413,.T.);
#14692=ORIENTED_EDGE('',*,*,#10422,.T.);
#14693=ORIENTED_EDGE('',*,*,#10423,.T.);
#14694=ORIENTED_EDGE('',*,*,#10424,.F.);
#14695=ORIENTED_EDGE('',*,*,#10281,.T.);
#14696=ORIENTED_EDGE('',*,*,#10421,.T.);
#14697=ORIENTED_EDGE('',*,*,#10425,.T.);
#14698=ORIENTED_EDGE('',*,*,#10426,.F.);
#14699=ORIENTED_EDGE('',*,*,#10408,.F.);
#14700=ORIENTED_EDGE('',*,*,#10318,.T.);
#14701=ORIENTED_EDGE('',*,*,#10427,.T.);
#14702=ORIENTED_EDGE('',*,*,#10412,.T.);
#14703=ORIENTED_EDGE('',*,*,#10407,.F.);
#14704=ORIENTED_EDGE('',*,*,#10428,.T.);
#14705=ORIENTED_EDGE('',*,*,#10429,.T.);
#14706=ORIENTED_EDGE('',*,*,#10319,.T.);
#14707=ORIENTED_EDGE('',*,*,#10430,.T.);
#14708=ORIENTED_EDGE('',*,*,#10320,.T.);
#14709=ORIENTED_EDGE('',*,*,#10429,.F.);
#14710=ORIENTED_EDGE('',*,*,#10431,.T.);
#14711=ORIENTED_EDGE('',*,*,#10365,.F.);
#14712=ORIENTED_EDGE('',*,*,#10321,.T.);
#14713=ORIENTED_EDGE('',*,*,#10430,.F.);
#14714=ORIENTED_EDGE('',*,*,#10432,.T.);
#14715=ORIENTED_EDGE('',*,*,#10427,.F.);
#14716=ORIENTED_EDGE('',*,*,#10433,.T.);
#14717=ORIENTED_EDGE('',*,*,#10422,.F.);
#14718=ORIENTED_EDGE('',*,*,#10402,.F.);
#14719=ORIENTED_EDGE('',*,*,#10415,.F.);
#14720=ORIENTED_EDGE('',*,*,#10418,.T.);
#14721=ORIENTED_EDGE('',*,*,#10434,.F.);
#14722=ORIENTED_EDGE('',*,*,#10428,.F.);
#14723=ORIENTED_EDGE('',*,*,#10406,.F.);
#14724=ORIENTED_EDGE('',*,*,#10425,.F.);
#14725=ORIENTED_EDGE('',*,*,#10423,.F.);
#14726=ORIENTED_EDGE('',*,*,#10435,.F.);
#14727=ORIENTED_EDGE('',*,*,#10436,.T.);
#14728=ORIENTED_EDGE('',*,*,#10437,.T.);
#14729=ORIENTED_EDGE('',*,*,#10433,.F.);
#14730=ORIENTED_EDGE('',*,*,#10317,.T.);
#14731=ORIENTED_EDGE('',*,*,#10438,.F.);
#14732=ORIENTED_EDGE('',*,*,#10435,.T.);
#14733=ORIENTED_EDGE('',*,*,#10438,.T.);
#14734=ORIENTED_EDGE('',*,*,#10316,.T.);
#14735=ORIENTED_EDGE('',*,*,#10394,.F.);
#14736=ORIENTED_EDGE('',*,*,#10439,.T.);
#14737=ORIENTED_EDGE('',*,*,#10439,.F.);
#14738=ORIENTED_EDGE('',*,*,#10398,.T.);
#14739=ORIENTED_EDGE('',*,*,#10440,.T.);
#14740=ORIENTED_EDGE('',*,*,#10436,.F.);
#14741=ORIENTED_EDGE('',*,*,#10419,.T.);
#14742=ORIENTED_EDGE('',*,*,#10441,.T.);
#14743=ORIENTED_EDGE('',*,*,#10442,.T.);
#14744=ORIENTED_EDGE('',*,*,#10441,.F.);
#14745=ORIENTED_EDGE('',*,*,#10442,.F.);
#14746=ORIENTED_EDGE('',*,*,#10443,.T.);
#14747=ORIENTED_EDGE('',*,*,#10444,.F.);
#14748=ORIENTED_EDGE('',*,*,#10445,.F.);
#14749=ORIENTED_EDGE('',*,*,#10443,.F.);
#14750=ORIENTED_EDGE('',*,*,#10446,.T.);
#14751=ORIENTED_EDGE('',*,*,#10447,.T.);
#14752=ORIENTED_EDGE('',*,*,#10448,.T.);
#14753=ORIENTED_EDGE('',*,*,#10449,.T.);
#14754=ORIENTED_EDGE('',*,*,#10450,.T.);
#14755=ORIENTED_EDGE('',*,*,#10446,.F.);
#14756=ORIENTED_EDGE('',*,*,#10451,.T.);
#14757=ORIENTED_EDGE('',*,*,#10452,.F.);
#14758=ORIENTED_EDGE('',*,*,#10451,.F.);
#14759=ORIENTED_EDGE('',*,*,#10453,.F.);
#14760=ORIENTED_EDGE('',*,*,#10454,.F.);
#14761=ORIENTED_EDGE('',*,*,#10455,.F.);
#14762=ORIENTED_EDGE('',*,*,#10456,.F.);
#14763=ORIENTED_EDGE('',*,*,#10448,.F.);
#14764=ORIENTED_EDGE('',*,*,#10457,.T.);
#14765=ORIENTED_EDGE('',*,*,#10458,.T.);
#14766=ORIENTED_EDGE('',*,*,#10453,.T.);
#14767=ORIENTED_EDGE('',*,*,#10459,.T.);
#14768=ORIENTED_EDGE('',*,*,#10460,.T.);
#14769=ORIENTED_EDGE('',*,*,#10461,.T.);
#14770=ORIENTED_EDGE('',*,*,#10462,.T.);
#14771=ORIENTED_EDGE('',*,*,#10463,.T.);
#14772=ORIENTED_EDGE('',*,*,#10464,.T.);
#14773=ORIENTED_EDGE('',*,*,#10461,.F.);
#14774=ORIENTED_EDGE('',*,*,#10465,.T.);
#14775=ORIENTED_EDGE('',*,*,#10466,.F.);
#14776=ORIENTED_EDGE('',*,*,#10467,.T.);
#14777=ORIENTED_EDGE('',*,*,#10468,.T.);
#14778=ORIENTED_EDGE('',*,*,#10460,.F.);
#14779=ORIENTED_EDGE('',*,*,#10469,.F.);
#14780=ORIENTED_EDGE('',*,*,#10470,.F.);
#14781=ORIENTED_EDGE('',*,*,#10465,.F.);
#14782=ORIENTED_EDGE('',*,*,#10459,.F.);
#14783=ORIENTED_EDGE('',*,*,#10471,.T.);
#14784=ORIENTED_EDGE('',*,*,#10472,.T.);
#14785=ORIENTED_EDGE('',*,*,#10473,.F.);
#14786=ORIENTED_EDGE('',*,*,#10469,.T.);
#14787=ORIENTED_EDGE('',*,*,#10474,.T.);
#14788=ORIENTED_EDGE('',*,*,#10456,.T.);
#14789=ORIENTED_EDGE('',*,*,#10475,.T.);
#14790=ORIENTED_EDGE('',*,*,#10470,.T.);
#14791=ORIENTED_EDGE('',*,*,#10467,.F.);
#14792=ORIENTED_EDGE('',*,*,#10476,.F.);
#14793=ORIENTED_EDGE('',*,*,#10477,.F.);
#14794=ORIENTED_EDGE('',*,*,#10478,.F.);
#14795=ORIENTED_EDGE('',*,*,#10472,.F.);
#14796=ORIENTED_EDGE('',*,*,#10479,.F.);
#14797=ORIENTED_EDGE('',*,*,#10480,.F.);
#14798=ORIENTED_EDGE('',*,*,#10481,.F.);
#14799=ORIENTED_EDGE('',*,*,#10464,.F.);
#14800=ORIENTED_EDGE('',*,*,#10482,.T.);
#14801=ORIENTED_EDGE('',*,*,#10483,.T.);
#14802=ORIENTED_EDGE('',*,*,#10484,.T.);
#14803=ORIENTED_EDGE('',*,*,#10479,.T.);
#14804=ORIENTED_EDGE('',*,*,#10471,.F.);
#14805=ORIENTED_EDGE('',*,*,#10485,.T.);
#14806=ORIENTED_EDGE('',*,*,#10352,.T.);
#14807=ORIENTED_EDGE('',*,*,#10385,.F.);
#14808=ORIENTED_EDGE('',*,*,#10286,.F.);
#14809=ORIENTED_EDGE('',*,*,#10335,.T.);
#14810=ORIENTED_EDGE('',*,*,#10485,.F.);
#14811=ORIENTED_EDGE('',*,*,#10334,.T.);
#14812=ORIENTED_EDGE('',*,*,#10387,.F.);
#14813=ORIENTED_EDGE('',*,*,#10486,.F.);
#14814=ORIENTED_EDGE('',*,*,#10353,.F.);
#14815=ORIENTED_EDGE('',*,*,#10487,.F.);
#14816=ORIENTED_EDGE('',*,*,#10487,.T.);
#14817=ORIENTED_EDGE('',*,*,#10488,.T.);
#14818=ORIENTED_EDGE('',*,*,#10489,.T.);
#14819=ORIENTED_EDGE('',*,*,#10488,.F.);
#14820=ORIENTED_EDGE('',*,*,#10489,.F.);
#14821=ORIENTED_EDGE('',*,*,#10490,.T.);
#14822=ORIENTED_EDGE('',*,*,#10491,.F.);
#14823=ORIENTED_EDGE('',*,*,#10492,.F.);
#14824=ORIENTED_EDGE('',*,*,#10490,.F.);
#14825=ORIENTED_EDGE('',*,*,#10493,.T.);
#14826=ORIENTED_EDGE('',*,*,#10455,.T.);
#14827=ORIENTED_EDGE('',*,*,#10494,.T.);
#14828=ORIENTED_EDGE('',*,*,#10495,.T.);
#14829=ORIENTED_EDGE('',*,*,#10493,.F.);
#14830=ORIENTED_EDGE('',*,*,#10496,.T.);
#14831=ORIENTED_EDGE('',*,*,#10466,.T.);
#14832=ORIENTED_EDGE('',*,*,#10475,.F.);
#14833=ORIENTED_EDGE('',*,*,#10497,.T.);
#14834=ORIENTED_EDGE('',*,*,#10498,.T.);
#14835=ORIENTED_EDGE('',*,*,#10449,.F.);
#14836=ORIENTED_EDGE('',*,*,#10452,.T.);
#14837=ORIENTED_EDGE('',*,*,#10499,.T.);
#14838=ORIENTED_EDGE('',*,*,#10497,.F.);
#14839=ORIENTED_EDGE('',*,*,#10474,.F.);
#14840=ORIENTED_EDGE('',*,*,#10473,.T.);
#14841=ORIENTED_EDGE('',*,*,#10496,.F.);
#14842=ORIENTED_EDGE('',*,*,#10500,.T.);
#14843=ORIENTED_EDGE('',*,*,#10501,.T.);
#14844=ORIENTED_EDGE('',*,*,#10476,.T.);
#14845=ORIENTED_EDGE('',*,*,#10502,.F.);
#14846=ORIENTED_EDGE('',*,*,#10503,.T.);
#14847=ORIENTED_EDGE('',*,*,#10501,.F.);
#14848=ORIENTED_EDGE('',*,*,#10504,.T.);
#14849=ORIENTED_EDGE('',*,*,#10504,.F.);
#14850=ORIENTED_EDGE('',*,*,#10505,.T.);
#14851=ORIENTED_EDGE('',*,*,#10506,.T.);
#14852=ORIENTED_EDGE('',*,*,#10507,.T.);
#14853=ORIENTED_EDGE('',*,*,#10495,.F.);
#14854=ORIENTED_EDGE('',*,*,#10508,.F.);
#14855=ORIENTED_EDGE('',*,*,#10505,.F.);
#14856=ORIENTED_EDGE('',*,*,#10500,.F.);
#14857=ORIENTED_EDGE('',*,*,#10462,.F.);
#14858=ORIENTED_EDGE('',*,*,#10468,.F.);
#14859=ORIENTED_EDGE('',*,*,#10478,.T.);
#14860=ORIENTED_EDGE('',*,*,#10509,.T.);
#14861=ORIENTED_EDGE('',*,*,#10510,.T.);
#14862=ORIENTED_EDGE('',*,*,#10503,.F.);
#14863=ORIENTED_EDGE('',*,*,#10511,.T.);
#14864=ORIENTED_EDGE('',*,*,#10512,.T.);
#14865=ORIENTED_EDGE('',*,*,#10477,.T.);
#14866=ORIENTED_EDGE('',*,*,#10512,.F.);
#14867=ORIENTED_EDGE('',*,*,#10513,.T.);
#14868=ORIENTED_EDGE('',*,*,#10509,.F.);
#14869=ORIENTED_EDGE('',*,*,#10463,.F.);
#14870=ORIENTED_EDGE('',*,*,#10510,.F.);
#14871=ORIENTED_EDGE('',*,*,#10514,.F.);
#14872=ORIENTED_EDGE('',*,*,#10482,.F.);
#14873=ORIENTED_EDGE('',*,*,#10513,.F.);
#14874=ORIENTED_EDGE('',*,*,#10515,.T.);
#14875=ORIENTED_EDGE('',*,*,#10516,.T.);
#14876=ORIENTED_EDGE('',*,*,#10483,.F.);
#14877=ORIENTED_EDGE('',*,*,#10514,.T.);
#14878=ORIENTED_EDGE('',*,*,#10511,.F.);
#14879=ORIENTED_EDGE('',*,*,#10517,.F.);
#14880=ORIENTED_EDGE('',*,*,#10518,.F.);
#14881=ORIENTED_EDGE('',*,*,#10515,.F.);
#14882=ORIENTED_EDGE('',*,*,#10519,.T.);
#14883=ORIENTED_EDGE('',*,*,#10520,.T.);
#14884=ORIENTED_EDGE('',*,*,#10521,.T.);
#14885=ORIENTED_EDGE('',*,*,#10520,.F.);
#14886=ORIENTED_EDGE('',*,*,#10522,.T.);
#14887=ORIENTED_EDGE('',*,*,#10523,.F.);
#14888=ORIENTED_EDGE('',*,*,#10524,.T.);
#14889=ORIENTED_EDGE('',*,*,#10522,.F.);
#14890=ORIENTED_EDGE('',*,*,#10519,.F.);
#14891=ORIENTED_EDGE('',*,*,#10524,.F.);
#14892=ORIENTED_EDGE('',*,*,#10525,.F.);
#14893=ORIENTED_EDGE('',*,*,#10521,.F.);
#14894=ORIENTED_EDGE('',*,*,#10526,.T.);
#14895=ORIENTED_EDGE('',*,*,#10527,.T.);
#14896=ORIENTED_EDGE('',*,*,#10528,.T.);
#14897=ORIENTED_EDGE('',*,*,#10529,.T.);
#14898=ORIENTED_EDGE('',*,*,#10525,.T.);
#14899=ORIENTED_EDGE('',*,*,#10523,.T.);
#14900=ORIENTED_EDGE('',*,*,#10529,.F.);
#14901=ORIENTED_EDGE('',*,*,#10530,.F.);
#14902=ORIENTED_EDGE('',*,*,#10531,.T.);
#14903=ORIENTED_EDGE('',*,*,#10527,.F.);
#14904=ORIENTED_EDGE('',*,*,#10528,.F.);
#14905=ORIENTED_EDGE('',*,*,#10531,.F.);
#14906=ORIENTED_EDGE('',*,*,#10532,.F.);
#14907=ORIENTED_EDGE('',*,*,#10533,.T.);
#14908=ORIENTED_EDGE('',*,*,#10376,.T.);
#14909=ORIENTED_EDGE('',*,*,#10381,.F.);
#14910=ORIENTED_EDGE('',*,*,#10290,.F.);
#14911=ORIENTED_EDGE('',*,*,#10359,.T.);
#14912=ORIENTED_EDGE('',*,*,#10533,.F.);
#14913=ORIENTED_EDGE('',*,*,#10358,.T.);
#14914=ORIENTED_EDGE('',*,*,#10383,.F.);
#14915=ORIENTED_EDGE('',*,*,#10534,.F.);
#14916=ORIENTED_EDGE('',*,*,#10377,.F.);
#14917=ORIENTED_EDGE('',*,*,#10535,.F.);
#14918=ORIENTED_EDGE('',*,*,#10536,.T.);
#14919=ORIENTED_EDGE('',*,*,#10396,.T.);
#14920=ORIENTED_EDGE('',*,*,#10399,.F.);
#14921=ORIENTED_EDGE('',*,*,#10282,.F.);
#14922=ORIENTED_EDGE('',*,*,#10424,.T.);
#14923=ORIENTED_EDGE('',*,*,#10536,.F.);
#14924=ORIENTED_EDGE('',*,*,#10426,.T.);
#14925=ORIENTED_EDGE('',*,*,#10437,.F.);
#14926=ORIENTED_EDGE('',*,*,#10440,.F.);
#14927=ORIENTED_EDGE('',*,*,#10397,.F.);
#14928=ORIENTED_EDGE('',*,*,#10537,.F.);
#14929=ORIENTED_EDGE('',*,*,#10484,.F.);
#14930=ORIENTED_EDGE('',*,*,#10516,.F.);
#14931=ORIENTED_EDGE('',*,*,#10518,.T.);
#14932=ORIENTED_EDGE('',*,*,#10538,.F.);
#14933=ORIENTED_EDGE('',*,*,#10539,.F.);
#14934=ORIENTED_EDGE('',*,*,#10480,.T.);
#14935=ORIENTED_EDGE('',*,*,#10499,.F.);
#14936=ORIENTED_EDGE('',*,*,#10481,.T.);
#14937=ORIENTED_EDGE('',*,*,#10539,.T.);
#14938=ORIENTED_EDGE('',*,*,#10540,.T.);
#14939=ORIENTED_EDGE('',*,*,#10498,.F.);
#14940=ORIENTED_EDGE('',*,*,#10540,.F.);
#14941=ORIENTED_EDGE('',*,*,#10541,.F.);
#14942=ORIENTED_EDGE('',*,*,#10542,.T.);
#14943=ORIENTED_EDGE('',*,*,#10502,.T.);
#14944=ORIENTED_EDGE('',*,*,#10543,.T.);
#14945=ORIENTED_EDGE('',*,*,#10544,.T.);
#14946=ORIENTED_EDGE('',*,*,#10517,.T.);
#14947=ORIENTED_EDGE('',*,*,#10538,.T.);
#14948=ORIENTED_EDGE('',*,*,#10544,.F.);
#14949=ORIENTED_EDGE('',*,*,#10545,.T.);
#14950=ORIENTED_EDGE('',*,*,#10507,.F.);
#14951=ORIENTED_EDGE('',*,*,#10546,.F.);
#14952=ORIENTED_EDGE('',*,*,#10547,.F.);
#14953=ORIENTED_EDGE('',*,*,#10548,.F.);
#14954=ORIENTED_EDGE('',*,*,#10549,.F.);
#14955=ORIENTED_EDGE('',*,*,#10543,.F.);
#14956=ORIENTED_EDGE('',*,*,#10545,.F.);
#14957=ORIENTED_EDGE('',*,*,#10549,.T.);
#14958=ORIENTED_EDGE('',*,*,#10550,.T.);
#14959=ORIENTED_EDGE('',*,*,#10541,.T.);
#14960=ORIENTED_EDGE('',*,*,#10537,.T.);
#14961=ORIENTED_EDGE('',*,*,#10551,.T.);
#14962=ORIENTED_EDGE('',*,*,#10552,.T.);
#14963=ORIENTED_EDGE('',*,*,#10551,.F.);
#14964=ORIENTED_EDGE('',*,*,#10552,.F.);
#14965=ORIENTED_EDGE('',*,*,#10553,.T.);
#14966=ORIENTED_EDGE('',*,*,#10554,.F.);
#14967=ORIENTED_EDGE('',*,*,#10555,.F.);
#14968=ORIENTED_EDGE('',*,*,#10553,.F.);
#14969=ORIENTED_EDGE('',*,*,#10535,.T.);
#14970=ORIENTED_EDGE('',*,*,#10556,.T.);
#14971=ORIENTED_EDGE('',*,*,#10557,.T.);
#14972=ORIENTED_EDGE('',*,*,#10556,.F.);
#14973=ORIENTED_EDGE('',*,*,#10557,.F.);
#14974=ORIENTED_EDGE('',*,*,#10558,.T.);
#14975=ORIENTED_EDGE('',*,*,#10559,.F.);
#14976=ORIENTED_EDGE('',*,*,#10560,.F.);
#14977=ORIENTED_EDGE('',*,*,#10558,.F.);
#14978=ORIENTED_EDGE('',*,*,#10561,.T.);
#14979=ORIENTED_EDGE('',*,*,#10562,.T.);
#14980=ORIENTED_EDGE('',*,*,#10563,.T.);
#14981=ORIENTED_EDGE('',*,*,#10564,.T.);
#14982=ORIENTED_EDGE('',*,*,#10562,.F.);
#14983=ORIENTED_EDGE('',*,*,#10565,.F.);
#14984=ORIENTED_EDGE('',*,*,#10566,.F.);
#14985=ORIENTED_EDGE('',*,*,#10567,.F.);
#14986=ORIENTED_EDGE('',*,*,#10568,.F.);
#14987=ORIENTED_EDGE('',*,*,#10569,.F.);
#14988=ORIENTED_EDGE('',*,*,#10570,.T.);
#14989=ORIENTED_EDGE('',*,*,#10571,.T.);
#14990=ORIENTED_EDGE('',*,*,#10572,.T.);
#14991=ORIENTED_EDGE('',*,*,#10573,.F.);
#14992=ORIENTED_EDGE('',*,*,#10574,.F.);
#14993=ORIENTED_EDGE('',*,*,#10575,.F.);
#14994=ORIENTED_EDGE('',*,*,#10561,.F.);
#14995=ORIENTED_EDGE('',*,*,#10576,.F.);
#14996=ORIENTED_EDGE('',*,*,#10577,.T.);
#14997=ORIENTED_EDGE('',*,*,#10563,.F.);
#14998=ORIENTED_EDGE('',*,*,#10564,.F.);
#14999=ORIENTED_EDGE('',*,*,#10577,.F.);
#15000=ORIENTED_EDGE('',*,*,#10566,.T.);
#15001=ORIENTED_EDGE('',*,*,#10578,.T.);
#15002=ORIENTED_EDGE('',*,*,#10579,.T.);
#15003=ORIENTED_EDGE('',*,*,#10580,.T.);
#15004=ORIENTED_EDGE('',*,*,#10578,.F.);
#15005=ORIENTED_EDGE('',*,*,#10581,.F.);
#15006=ORIENTED_EDGE('',*,*,#10582,.T.);
#15007=ORIENTED_EDGE('',*,*,#10579,.F.);
#15008=ORIENTED_EDGE('',*,*,#10580,.F.);
#15009=ORIENTED_EDGE('',*,*,#10582,.F.);
#15010=ORIENTED_EDGE('',*,*,#10565,.T.);
#15011=ORIENTED_EDGE('',*,*,#10583,.T.);
#15012=ORIENTED_EDGE('',*,*,#10532,.T.);
#15013=ORIENTED_EDGE('',*,*,#10530,.T.);
#15014=ORIENTED_EDGE('',*,*,#10583,.F.);
#15015=ORIENTED_EDGE('',*,*,#10567,.T.);
#15016=ORIENTED_EDGE('',*,*,#10584,.T.);
#15017=ORIENTED_EDGE('',*,*,#10491,.T.);
#15018=ORIENTED_EDGE('',*,*,#10492,.T.);
#15019=ORIENTED_EDGE('',*,*,#10584,.F.);
#15020=ORIENTED_EDGE('',*,*,#10575,.T.);
#15021=ORIENTED_EDGE('',*,*,#10585,.T.);
#15022=ORIENTED_EDGE('',*,*,#10444,.T.);
#15023=ORIENTED_EDGE('',*,*,#10445,.T.);
#15024=ORIENTED_EDGE('',*,*,#10585,.F.);
#15025=ORIENTED_EDGE('',*,*,#10568,.T.);
#15026=ORIENTED_EDGE('',*,*,#10586,.T.);
#15027=ORIENTED_EDGE('',*,*,#10587,.T.);
#15028=ORIENTED_EDGE('',*,*,#10588,.T.);
#15029=ORIENTED_EDGE('',*,*,#10586,.F.);
#15030=ORIENTED_EDGE('',*,*,#10589,.F.);
#15031=ORIENTED_EDGE('',*,*,#10590,.T.);
#15032=ORIENTED_EDGE('',*,*,#10587,.F.);
#15033=ORIENTED_EDGE('',*,*,#10588,.F.);
#15034=ORIENTED_EDGE('',*,*,#10590,.F.);
#15035=ORIENTED_EDGE('',*,*,#10574,.T.);
#15036=ORIENTED_EDGE('',*,*,#10591,.T.);
#15037=ORIENTED_EDGE('',*,*,#10559,.T.);
#15038=ORIENTED_EDGE('',*,*,#10560,.T.);
#15039=ORIENTED_EDGE('',*,*,#10591,.F.);
#15040=ORIENTED_EDGE('',*,*,#10569,.T.);
#15041=ORIENTED_EDGE('',*,*,#10592,.T.);
#15042=ORIENTED_EDGE('',*,*,#10554,.T.);
#15043=ORIENTED_EDGE('',*,*,#10555,.T.);
#15044=ORIENTED_EDGE('',*,*,#10592,.F.);
#15045=ORIENTED_EDGE('',*,*,#10593,.T.);
#15046=ORIENTED_EDGE('',*,*,#10594,.T.);
#15047=ORIENTED_EDGE('',*,*,#10595,.T.);
#15048=ORIENTED_EDGE('',*,*,#10594,.F.);
#15049=ORIENTED_EDGE('',*,*,#10596,.F.);
#15050=ORIENTED_EDGE('',*,*,#10597,.T.);
#15051=ORIENTED_EDGE('',*,*,#10593,.F.);
#15052=ORIENTED_EDGE('',*,*,#10597,.F.);
#15053=ORIENTED_EDGE('',*,*,#10598,.T.);
#15054=ORIENTED_EDGE('',*,*,#10595,.F.);
#15055=ORIENTED_EDGE('',*,*,#10599,.T.);
#15056=ORIENTED_EDGE('',*,*,#10600,.T.);
#15057=ORIENTED_EDGE('',*,*,#10601,.T.);
#15058=ORIENTED_EDGE('',*,*,#10600,.F.);
#15059=ORIENTED_EDGE('',*,*,#10602,.F.);
#15060=ORIENTED_EDGE('',*,*,#10603,.T.);
#15061=ORIENTED_EDGE('',*,*,#10599,.F.);
#15062=ORIENTED_EDGE('',*,*,#10603,.F.);
#15063=ORIENTED_EDGE('',*,*,#10604,.T.);
#15064=ORIENTED_EDGE('',*,*,#10601,.F.);
#15065=ORIENTED_EDGE('',*,*,#10605,.T.);
#15066=ORIENTED_EDGE('',*,*,#10606,.T.);
#15067=ORIENTED_EDGE('',*,*,#10607,.T.);
#15068=ORIENTED_EDGE('',*,*,#10606,.F.);
#15069=ORIENTED_EDGE('',*,*,#10608,.F.);
#15070=ORIENTED_EDGE('',*,*,#10609,.T.);
#15071=ORIENTED_EDGE('',*,*,#10605,.F.);
#15072=ORIENTED_EDGE('',*,*,#10609,.F.);
#15073=ORIENTED_EDGE('',*,*,#10610,.T.);
#15074=ORIENTED_EDGE('',*,*,#10607,.F.);
#15075=ORIENTED_EDGE('',*,*,#10447,.F.);
#15076=ORIENTED_EDGE('',*,*,#10611,.T.);
#15077=ORIENTED_EDGE('',*,*,#10612,.T.);
#15078=ORIENTED_EDGE('',*,*,#10613,.T.);
#15079=ORIENTED_EDGE('',*,*,#10614,.T.);
#15080=ORIENTED_EDGE('',*,*,#10615,.T.);
#15081=ORIENTED_EDGE('',*,*,#10550,.F.);
#15082=ORIENTED_EDGE('',*,*,#10548,.T.);
#15083=ORIENTED_EDGE('',*,*,#10614,.F.);
#15084=ORIENTED_EDGE('',*,*,#10616,.T.);
#15085=ORIENTED_EDGE('',*,*,#10612,.F.);
#15086=ORIENTED_EDGE('',*,*,#10617,.F.);
#15087=ORIENTED_EDGE('',*,*,#10457,.F.);
#15088=ORIENTED_EDGE('',*,*,#10613,.F.);
#15089=ORIENTED_EDGE('',*,*,#10618,.F.);
#15090=ORIENTED_EDGE('',*,*,#10619,.F.);
#15091=ORIENTED_EDGE('',*,*,#10620,.F.);
#15092=ORIENTED_EDGE('',*,*,#10621,.F.);
#15093=ORIENTED_EDGE('',*,*,#10622,.T.);
#15094=ORIENTED_EDGE('',*,*,#10616,.F.);
#15095=ORIENTED_EDGE('',*,*,#10547,.T.);
#15096=ORIENTED_EDGE('',*,*,#10623,.F.);
#15097=ORIENTED_EDGE('',*,*,#10624,.F.);
#15098=ORIENTED_EDGE('',*,*,#10618,.T.);
#15099=ORIENTED_EDGE('',*,*,#10625,.T.);
#15100=ORIENTED_EDGE('',*,*,#10626,.T.);
#15101=ORIENTED_EDGE('',*,*,#10627,.T.);
#15102=ORIENTED_EDGE('',*,*,#10628,.T.);
#15103=ORIENTED_EDGE('',*,*,#10629,.T.);
#15104=ORIENTED_EDGE('',*,*,#10627,.F.);
#15105=ORIENTED_EDGE('',*,*,#10629,.F.);
#15106=ORIENTED_EDGE('',*,*,#10630,.T.);
#15107=ORIENTED_EDGE('',*,*,#10631,.F.);
#15108=ORIENTED_EDGE('',*,*,#10632,.F.);
#15109=ORIENTED_EDGE('',*,*,#10630,.F.);
#15110=ORIENTED_EDGE('',*,*,#10628,.F.);
#15111=ORIENTED_EDGE('',*,*,#10633,.F.);
#15112=ORIENTED_EDGE('',*,*,#10634,.T.);
#15113=ORIENTED_EDGE('',*,*,#10625,.F.);
#15114=ORIENTED_EDGE('',*,*,#10626,.F.);
#15115=ORIENTED_EDGE('',*,*,#10634,.F.);
#15116=ORIENTED_EDGE('',*,*,#10635,.F.);
#15117=ORIENTED_EDGE('',*,*,#10631,.T.);
#15118=ORIENTED_EDGE('',*,*,#10632,.T.);
#15119=ORIENTED_EDGE('',*,*,#10636,.T.);
#15120=ORIENTED_EDGE('',*,*,#10637,.T.);
#15121=ORIENTED_EDGE('',*,*,#10636,.F.);
#15122=ORIENTED_EDGE('',*,*,#10637,.F.);
#15123=ORIENTED_EDGE('',*,*,#10638,.F.);
#15124=ORIENTED_EDGE('',*,*,#10639,.F.);
#15125=ORIENTED_EDGE('',*,*,#10640,.T.);
#15126=ORIENTED_EDGE('',*,*,#10641,.T.);
#15127=ORIENTED_EDGE('',*,*,#10642,.T.);
#15128=ORIENTED_EDGE('',*,*,#10643,.F.);
#15129=ORIENTED_EDGE('',*,*,#10644,.F.);
#15130=ORIENTED_EDGE('',*,*,#10638,.T.);
#15131=ORIENTED_EDGE('',*,*,#10645,.T.);
#15132=ORIENTED_EDGE('',*,*,#10608,.T.);
#15133=ORIENTED_EDGE('',*,*,#10645,.F.);
#15134=ORIENTED_EDGE('',*,*,#10644,.T.);
#15135=ORIENTED_EDGE('',*,*,#10646,.T.);
#15136=ORIENTED_EDGE('',*,*,#10602,.T.);
#15137=ORIENTED_EDGE('',*,*,#10646,.F.);
#15138=ORIENTED_EDGE('',*,*,#10639,.T.);
#15139=ORIENTED_EDGE('',*,*,#10647,.T.);
#15140=ORIENTED_EDGE('',*,*,#10596,.T.);
#15141=ORIENTED_EDGE('',*,*,#10647,.F.);
#15142=ORIENTED_EDGE('',*,*,#10648,.T.);
#15143=ORIENTED_EDGE('',*,*,#10649,.T.);
#15144=ORIENTED_EDGE('',*,*,#10650,.T.);
#15145=ORIENTED_EDGE('',*,*,#10573,.T.);
#15146=ORIENTED_EDGE('',*,*,#10650,.F.);
#15147=ORIENTED_EDGE('',*,*,#10648,.F.);
#15148=ORIENTED_EDGE('',*,*,#10649,.F.);
#15149=ORIENTED_EDGE('',*,*,#10651,.T.);
#15150=ORIENTED_EDGE('',*,*,#10652,.F.);
#15151=ORIENTED_EDGE('',*,*,#10653,.F.);
#15152=ORIENTED_EDGE('',*,*,#10651,.F.);
#15153=ORIENTED_EDGE('',*,*,#10654,.T.);
#15154=ORIENTED_EDGE('',*,*,#10655,.T.);
#15155=ORIENTED_EDGE('',*,*,#10327,.T.);
#15156=ORIENTED_EDGE('',*,*,#10655,.F.);
#15157=ORIENTED_EDGE('',*,*,#10656,.T.);
#15158=ORIENTED_EDGE('',*,*,#10654,.F.);
#15159=ORIENTED_EDGE('',*,*,#10657,.T.);
#15160=ORIENTED_EDGE('',*,*,#10658,.F.);
#15161=ORIENTED_EDGE('',*,*,#10659,.F.);
#15162=ORIENTED_EDGE('',*,*,#10657,.F.);
#15163=ORIENTED_EDGE('',*,*,#10656,.F.);
#15164=ORIENTED_EDGE('',*,*,#10659,.T.);
#15165=ORIENTED_EDGE('',*,*,#10660,.T.);
#15166=ORIENTED_EDGE('',*,*,#10652,.T.);
#15167=ORIENTED_EDGE('',*,*,#10653,.T.);
#15168=ORIENTED_EDGE('',*,*,#10660,.F.);
#15169=ORIENTED_EDGE('',*,*,#10658,.T.);
#15170=ORIENTED_EDGE('',*,*,#10643,.T.);
#15171=ORIENTED_EDGE('',*,*,#10661,.T.);
#15172=ORIENTED_EDGE('',*,*,#10662,.T.);
#15173=ORIENTED_EDGE('',*,*,#10663,.T.);
#15174=ORIENTED_EDGE('',*,*,#10661,.F.);
#15175=ORIENTED_EDGE('',*,*,#10664,.F.);
#15176=ORIENTED_EDGE('',*,*,#10665,.T.);
#15177=ORIENTED_EDGE('',*,*,#10662,.F.);
#15178=ORIENTED_EDGE('',*,*,#10663,.F.);
#15179=ORIENTED_EDGE('',*,*,#10665,.F.);
#15180=ORIENTED_EDGE('',*,*,#10666,.F.);
#15181=ORIENTED_EDGE('',*,*,#10667,.T.);
#15182=ORIENTED_EDGE('',*,*,#10668,.T.);
#15183=ORIENTED_EDGE('',*,*,#10669,.T.);
#15184=ORIENTED_EDGE('',*,*,#10635,.T.);
#15185=ORIENTED_EDGE('',*,*,#10633,.T.);
#15186=ORIENTED_EDGE('',*,*,#10669,.F.);
#15187=ORIENTED_EDGE('',*,*,#10622,.F.);
#15188=ORIENTED_EDGE('',*,*,#10670,.F.);
#15189=ORIENTED_EDGE('',*,*,#10671,.T.);
#15190=ORIENTED_EDGE('',*,*,#10667,.F.);
#15191=ORIENTED_EDGE('',*,*,#10668,.F.);
#15192=ORIENTED_EDGE('',*,*,#10671,.F.);
#15193=ORIENTED_EDGE('',*,*,#10672,.F.);
#15194=ORIENTED_EDGE('',*,*,#10673,.F.);
#15195=ORIENTED_EDGE('',*,*,#10674,.F.);
#15196=ORIENTED_EDGE('',*,*,#10675,.T.);
#15197=ORIENTED_EDGE('',*,*,#10028,.F.);
#15198=ORIENTED_EDGE('',*,*,#10063,.F.);
#15199=ORIENTED_EDGE('',*,*,#10676,.T.);
#15200=ORIENTED_EDGE('',*,*,#10061,.T.);
#15201=ORIENTED_EDGE('',*,*,#10068,.T.);
#15202=ORIENTED_EDGE('',*,*,#10677,.T.);
#15203=ORIENTED_EDGE('',*,*,#10134,.F.);
#15204=ORIENTED_EDGE('',*,*,#10128,.F.);
#15205=ORIENTED_EDGE('',*,*,#10678,.T.);
#15206=ORIENTED_EDGE('',*,*,#10126,.T.);
#15207=ORIENTED_EDGE('',*,*,#10115,.T.);
#15208=ORIENTED_EDGE('',*,*,#10679,.T.);
#15209=ORIENTED_EDGE('',*,*,#10262,.F.);
#15210=ORIENTED_EDGE('',*,*,#10680,.F.);
#15211=ORIENTED_EDGE('',*,*,#10681,.T.);
#15212=ORIENTED_EDGE('',*,*,#10682,.F.);
#15213=ORIENTED_EDGE('',*,*,#10672,.T.);
#15214=ORIENTED_EDGE('',*,*,#10670,.T.);
#15215=ORIENTED_EDGE('',*,*,#10621,.T.);
#15216=ORIENTED_EDGE('',*,*,#10683,.T.);
#15217=ORIENTED_EDGE('',*,*,#10619,.T.);
#15218=ORIENTED_EDGE('',*,*,#10624,.T.);
#15219=ORIENTED_EDGE('',*,*,#10684,.T.);
#15220=ORIENTED_EDGE('',*,*,#10685,.T.);
#15221=ORIENTED_EDGE('',*,*,#10686,.T.);
#15222=ORIENTED_EDGE('',*,*,#10687,.T.);
#15223=ORIENTED_EDGE('',*,*,#10685,.F.);
#15224=ORIENTED_EDGE('',*,*,#10675,.F.);
#15225=ORIENTED_EDGE('',*,*,#10623,.T.);
#15226=ORIENTED_EDGE('',*,*,#10546,.T.);
#15227=ORIENTED_EDGE('',*,*,#10506,.F.);
#15228=ORIENTED_EDGE('',*,*,#10508,.T.);
#15229=ORIENTED_EDGE('',*,*,#10494,.F.);
#15230=ORIENTED_EDGE('',*,*,#10454,.T.);
#15231=ORIENTED_EDGE('',*,*,#10458,.F.);
#15232=ORIENTED_EDGE('',*,*,#10617,.T.);
#15233=ORIENTED_EDGE('',*,*,#10674,.T.);
#15234=ORIENTED_EDGE('',*,*,#10688,.T.);
#15235=ORIENTED_EDGE('',*,*,#10184,.T.);
#15236=ORIENTED_EDGE('',*,*,#10245,.T.);
#15237=ORIENTED_EDGE('',*,*,#10233,.F.);
#15238=ORIENTED_EDGE('',*,*,#10235,.T.);
#15239=ORIENTED_EDGE('',*,*,#10197,.F.);
#15240=ORIENTED_EDGE('',*,*,#10253,.T.);
#15241=ORIENTED_EDGE('',*,*,#10263,.F.);
#15242=ORIENTED_EDGE('',*,*,#10679,.F.);
#15243=ORIENTED_EDGE('',*,*,#10119,.T.);
#15244=ORIENTED_EDGE('',*,*,#10132,.T.);
#15245=ORIENTED_EDGE('',*,*,#10071,.F.);
#15246=ORIENTED_EDGE('',*,*,#10082,.T.);
#15247=ORIENTED_EDGE('',*,*,#10159,.F.);
#15248=ORIENTED_EDGE('',*,*,#10156,.T.);
#15249=ORIENTED_EDGE('',*,*,#10135,.F.);
#15250=ORIENTED_EDGE('',*,*,#10677,.F.);
#15251=ORIENTED_EDGE('',*,*,#10067,.T.);
#15252=ORIENTED_EDGE('',*,*,#10048,.T.);
#15253=ORIENTED_EDGE('',*,*,#10046,.F.);
#15254=ORIENTED_EDGE('',*,*,#10689,.T.);
#15255=ORIENTED_EDGE('',*,*,#10017,.F.);
#15256=ORIENTED_EDGE('',*,*,#10021,.T.);
#15257=ORIENTED_EDGE('',*,*,#10029,.F.);
#15258=ORIENTED_EDGE('',*,*,#10690,.F.);
#15259=ORIENTED_EDGE('',*,*,#10691,.F.);
#15260=ORIENTED_EDGE('',*,*,#10692,.F.);
#15261=ORIENTED_EDGE('',*,*,#10684,.F.);
#15262=ORIENTED_EDGE('',*,*,#10610,.F.);
#15263=ORIENTED_EDGE('',*,*,#10693,.T.);
#15264=ORIENTED_EDGE('',*,*,#10686,.F.);
#15265=ORIENTED_EDGE('',*,*,#10687,.F.);
#15266=ORIENTED_EDGE('',*,*,#10693,.F.);
#15267=ORIENTED_EDGE('',*,*,#10690,.T.);
#15268=ORIENTED_EDGE('',*,*,#10694,.T.);
#15269=ORIENTED_EDGE('',*,*,#10695,.T.);
#15270=ORIENTED_EDGE('',*,*,#10696,.T.);
#15271=ORIENTED_EDGE('',*,*,#10694,.F.);
#15272=ORIENTED_EDGE('',*,*,#10604,.F.);
#15273=ORIENTED_EDGE('',*,*,#10697,.T.);
#15274=ORIENTED_EDGE('',*,*,#10695,.F.);
#15275=ORIENTED_EDGE('',*,*,#10696,.F.);
#15276=ORIENTED_EDGE('',*,*,#10697,.F.);
#15277=ORIENTED_EDGE('',*,*,#10692,.T.);
#15278=ORIENTED_EDGE('',*,*,#10698,.T.);
#15279=ORIENTED_EDGE('',*,*,#10699,.T.);
#15280=ORIENTED_EDGE('',*,*,#10700,.T.);
#15281=ORIENTED_EDGE('',*,*,#10698,.F.);
#15282=ORIENTED_EDGE('',*,*,#10598,.F.);
#15283=ORIENTED_EDGE('',*,*,#10701,.T.);
#15284=ORIENTED_EDGE('',*,*,#10699,.F.);
#15285=ORIENTED_EDGE('',*,*,#10700,.F.);
#15286=ORIENTED_EDGE('',*,*,#10701,.F.);
#15287=ORIENTED_EDGE('',*,*,#10702,.T.);
#15288=ORIENTED_EDGE('',*,*,#10703,.T.);
#15289=ORIENTED_EDGE('',*,*,#10666,.T.);
#15290=ORIENTED_EDGE('',*,*,#10664,.T.);
#15291=ORIENTED_EDGE('',*,*,#10703,.F.);
#15292=ORIENTED_EDGE('',*,*,#10704,.T.);
#15293=ORIENTED_EDGE('',*,*,#10702,.F.);
#15294=ORIENTED_EDGE('',*,*,#10705,.T.);
#15295=ORIENTED_EDGE('',*,*,#10706,.F.);
#15296=ORIENTED_EDGE('',*,*,#10707,.F.);
#15297=ORIENTED_EDGE('',*,*,#10705,.F.);
#15298=ORIENTED_EDGE('',*,*,#10704,.F.);
#15299=ORIENTED_EDGE('',*,*,#10707,.T.);
#15300=ORIENTED_EDGE('',*,*,#10708,.T.);
#15301=ORIENTED_EDGE('',*,*,#10691,.T.);
#15302=ORIENTED_EDGE('',*,*,#10708,.F.);
#15303=ORIENTED_EDGE('',*,*,#10706,.T.);
#15304=ORIENTED_EDGE('',*,*,#10364,.F.);
#15305=ORIENTED_EDGE('',*,*,#10432,.F.);
#15306=ORIENTED_EDGE('',*,*,#10709,.T.);
#15307=ORIENTED_EDGE('',*,*,#10416,.T.);
#15308=ORIENTED_EDGE('',*,*,#10369,.F.);
#15309=ORIENTED_EDGE('',*,*,#10431,.F.);
#15310=ORIENTED_EDGE('',*,*,#10434,.T.);
#15311=ORIENTED_EDGE('',*,*,#10417,.T.);
#15312=ORIENTED_EDGE('',*,*,#10709,.F.);
#15313=ORIENTED_EDGE('',*,*,#10341,.F.);
#15314=ORIENTED_EDGE('',*,*,#10378,.T.);
#15315=ORIENTED_EDGE('',*,*,#10534,.T.);
#15316=ORIENTED_EDGE('',*,*,#10382,.F.);
#15317=ORIENTED_EDGE('',*,*,#10301,.F.);
#15318=ORIENTED_EDGE('',*,*,#10354,.T.);
#15319=ORIENTED_EDGE('',*,*,#10486,.T.);
#15320=ORIENTED_EDGE('',*,*,#10386,.F.);
#15321=ORIENTED_EDGE('',*,*,#10589,.T.);
#15322=ORIENTED_EDGE('',*,*,#10576,.T.);
#15323=ORIENTED_EDGE('',*,*,#10581,.T.);
#15324=ORIENTED_EDGE('',*,*,#10688,.F.);
#15325=ORIENTED_EDGE('',*,*,#10673,.T.);
#15326=ORIENTED_EDGE('',*,*,#10682,.T.);
#15327=ORIENTED_EDGE('',*,*,#10710,.F.);
#15328=ORIENTED_EDGE('',*,*,#10680,.T.);
#15329=ORIENTED_EDGE('',*,*,#10261,.F.);
#15330=ORIENTED_EDGE('',*,*,#10180,.F.);
#15331=ORIENTED_EDGE('',*,*,#10185,.F.);
#15332=ORIENTED_EDGE('',*,*,#10681,.F.);
#15333=ORIENTED_EDGE('',*,*,#10710,.T.);
#15334=ORIENTED_EDGE('',*,*,#10678,.F.);
#15335=ORIENTED_EDGE('',*,*,#10127,.T.);
#15336=ORIENTED_EDGE('',*,*,#10676,.F.);
#15337=ORIENTED_EDGE('',*,*,#10062,.T.);
#15338=ORIENTED_EDGE('',*,*,#10450,.F.);
#15339=ORIENTED_EDGE('',*,*,#10542,.F.);
#15340=ORIENTED_EDGE('',*,*,#10615,.F.);
#15341=ORIENTED_EDGE('',*,*,#10611,.F.);
#15342=ORIENTED_EDGE('',*,*,#10683,.F.);
#15343=ORIENTED_EDGE('',*,*,#10620,.T.);
#15344=ORIENTED_EDGE('',*,*,#9976,.F.);
#15345=ORIENTED_EDGE('',*,*,#10018,.F.);
#15346=ORIENTED_EDGE('',*,*,#10689,.F.);
#15347=ORIENTED_EDGE('',*,*,#10045,.F.);
#15348=ORIENTED_EDGE('',*,*,#10293,.T.);
#15349=ORIENTED_EDGE('',*,*,#10711,.T.);
#15350=ORIENTED_EDGE('',*,*,#10526,.F.);
#15351=ORIENTED_EDGE('',*,*,#10711,.F.);
#15352=ORIENTED_EDGE('',*,*,#10640,.F.);
#15353=ORIENTED_EDGE('',*,*,#10712,.T.);
#15354=ORIENTED_EDGE('',*,*,#10570,.F.);
#15355=ORIENTED_EDGE('',*,*,#10712,.F.);
#15356=ORIENTED_EDGE('',*,*,#10641,.F.);
#15357=ORIENTED_EDGE('',*,*,#10713,.T.);
#15358=ORIENTED_EDGE('',*,*,#10571,.F.);
#15359=ORIENTED_EDGE('',*,*,#10713,.F.);
#15360=ORIENTED_EDGE('',*,*,#10642,.F.);
#15361=ORIENTED_EDGE('',*,*,#10714,.T.);
#15362=ORIENTED_EDGE('',*,*,#10572,.F.);
#15363=ORIENTED_EDGE('',*,*,#10714,.F.);
#15364=ORIENTED_EDGE('',*,*,#10715,.T.);
#15365=ORIENTED_EDGE('',*,*,#10716,.T.);
#15366=ORIENTED_EDGE('',*,*,#10717,.T.);
#15367=ORIENTED_EDGE('',*,*,#10718,.T.);
#15368=ORIENTED_EDGE('',*,*,#10717,.F.);
#15369=ORIENTED_EDGE('',*,*,#10715,.F.);
#15370=ORIENTED_EDGE('',*,*,#10716,.F.);
#15371=ORIENTED_EDGE('',*,*,#10719,.T.);
#15372=ORIENTED_EDGE('',*,*,#10720,.F.);
#15373=ORIENTED_EDGE('',*,*,#10721,.F.);
#15374=ORIENTED_EDGE('',*,*,#10719,.F.);
#15375=ORIENTED_EDGE('',*,*,#10722,.T.);
#15376=ORIENTED_EDGE('',*,*,#10723,.T.);
#15377=ORIENTED_EDGE('',*,*,#10724,.T.);
#15378=ORIENTED_EDGE('',*,*,#10725,.T.);
#15379=ORIENTED_EDGE('',*,*,#10726,.T.);
#15380=ORIENTED_EDGE('',*,*,#10727,.T.);
#15381=ORIENTED_EDGE('',*,*,#10728,.T.);
#15382=ORIENTED_EDGE('',*,*,#10729,.T.);
#15383=ORIENTED_EDGE('',*,*,#10730,.T.);
#15384=ORIENTED_EDGE('',*,*,#10731,.T.);
#15385=ORIENTED_EDGE('',*,*,#10732,.T.);
#15386=ORIENTED_EDGE('',*,*,#10733,.T.);
#15387=ORIENTED_EDGE('',*,*,#10734,.T.);
#15388=ORIENTED_EDGE('',*,*,#10735,.T.);
#15389=ORIENTED_EDGE('',*,*,#10736,.T.);
#15390=ORIENTED_EDGE('',*,*,#10737,.T.);
#15391=ORIENTED_EDGE('',*,*,#10738,.T.);
#15392=ORIENTED_EDGE('',*,*,#10739,.T.);
#15393=ORIENTED_EDGE('',*,*,#10740,.T.);
#15394=ORIENTED_EDGE('',*,*,#10741,.T.);
#15395=ORIENTED_EDGE('',*,*,#10742,.T.);
#15396=ORIENTED_EDGE('',*,*,#10743,.T.);
#15397=ORIENTED_EDGE('',*,*,#10744,.T.);
#15398=ORIENTED_EDGE('',*,*,#10745,.T.);
#15399=ORIENTED_EDGE('',*,*,#10746,.T.);
#15400=ORIENTED_EDGE('',*,*,#10747,.T.);
#15401=ORIENTED_EDGE('',*,*,#10748,.T.);
#15402=ORIENTED_EDGE('',*,*,#10749,.T.);
#15403=ORIENTED_EDGE('',*,*,#10750,.T.);
#15404=ORIENTED_EDGE('',*,*,#10751,.T.);
#15405=ORIENTED_EDGE('',*,*,#10752,.T.);
#15406=ORIENTED_EDGE('',*,*,#10753,.T.);
#15407=ORIENTED_EDGE('',*,*,#10754,.T.);
#15408=ORIENTED_EDGE('',*,*,#10755,.T.);
#15409=ORIENTED_EDGE('',*,*,#10756,.T.);
#15410=ORIENTED_EDGE('',*,*,#10757,.T.);
#15411=ORIENTED_EDGE('',*,*,#10758,.T.);
#15412=ORIENTED_EDGE('',*,*,#10759,.T.);
#15413=ORIENTED_EDGE('',*,*,#10760,.T.);
#15414=ORIENTED_EDGE('',*,*,#10761,.T.);
#15415=ORIENTED_EDGE('',*,*,#10762,.T.);
#15416=ORIENTED_EDGE('',*,*,#10763,.T.);
#15417=ORIENTED_EDGE('',*,*,#10764,.T.);
#15418=ORIENTED_EDGE('',*,*,#10765,.T.);
#15419=ORIENTED_EDGE('',*,*,#10766,.T.);
#15420=ORIENTED_EDGE('',*,*,#10767,.T.);
#15421=ORIENTED_EDGE('',*,*,#10768,.T.);
#15422=ORIENTED_EDGE('',*,*,#10769,.T.);
#15423=ORIENTED_EDGE('',*,*,#10770,.T.);
#15424=ORIENTED_EDGE('',*,*,#10771,.T.);
#15425=ORIENTED_EDGE('',*,*,#10772,.T.);
#15426=ORIENTED_EDGE('',*,*,#10773,.T.);
#15427=ORIENTED_EDGE('',*,*,#10774,.T.);
#15428=ORIENTED_EDGE('',*,*,#10775,.T.);
#15429=ORIENTED_EDGE('',*,*,#10776,.T.);
#15430=ORIENTED_EDGE('',*,*,#10777,.T.);
#15431=ORIENTED_EDGE('',*,*,#10718,.F.);
#15432=ORIENTED_EDGE('',*,*,#10778,.T.);
#15433=ORIENTED_EDGE('',*,*,#10779,.T.);
#15434=ORIENTED_EDGE('',*,*,#10720,.T.);
#15435=ORIENTED_EDGE('',*,*,#10721,.T.);
#15436=ORIENTED_EDGE('',*,*,#10779,.F.);
#15437=ORIENTED_EDGE('',*,*,#10780,.T.);
#15438=ORIENTED_EDGE('',*,*,#10781,.T.);
#15439=ORIENTED_EDGE('',*,*,#10782,.T.);
#15440=ORIENTED_EDGE('',*,*,#10783,.F.);
#15441=ORIENTED_EDGE('',*,*,#10784,.T.);
#15442=ORIENTED_EDGE('',*,*,#10785,.T.);
#15443=ORIENTED_EDGE('',*,*,#10786,.T.);
#15444=ORIENTED_EDGE('',*,*,#10787,.F.);
#15445=ORIENTED_EDGE('',*,*,#10788,.T.);
#15446=ORIENTED_EDGE('',*,*,#10789,.T.);
#15447=ORIENTED_EDGE('',*,*,#10790,.T.);
#15448=ORIENTED_EDGE('',*,*,#10791,.F.);
#15449=ORIENTED_EDGE('',*,*,#10792,.T.);
#15450=ORIENTED_EDGE('',*,*,#10793,.T.);
#15451=ORIENTED_EDGE('',*,*,#10794,.T.);
#15452=ORIENTED_EDGE('',*,*,#10795,.F.);
#15453=ORIENTED_EDGE('',*,*,#10796,.T.);
#15454=ORIENTED_EDGE('',*,*,#10797,.T.);
#15455=ORIENTED_EDGE('',*,*,#10798,.T.);
#15456=ORIENTED_EDGE('',*,*,#10799,.F.);
#15457=ORIENTED_EDGE('',*,*,#10800,.T.);
#15458=ORIENTED_EDGE('',*,*,#10801,.T.);
#15459=ORIENTED_EDGE('',*,*,#10802,.T.);
#15460=ORIENTED_EDGE('',*,*,#10803,.F.);
#15461=ORIENTED_EDGE('',*,*,#10804,.T.);
#15462=ORIENTED_EDGE('',*,*,#10805,.T.);
#15463=ORIENTED_EDGE('',*,*,#10806,.T.);
#15464=ORIENTED_EDGE('',*,*,#10807,.F.);
#15465=ORIENTED_EDGE('',*,*,#10808,.T.);
#15466=ORIENTED_EDGE('',*,*,#10809,.T.);
#15467=ORIENTED_EDGE('',*,*,#10810,.T.);
#15468=ORIENTED_EDGE('',*,*,#10811,.F.);
#15469=ORIENTED_EDGE('',*,*,#10812,.T.);
#15470=ORIENTED_EDGE('',*,*,#10813,.T.);
#15471=ORIENTED_EDGE('',*,*,#10814,.T.);
#15472=ORIENTED_EDGE('',*,*,#10815,.F.);
#15473=ORIENTED_EDGE('',*,*,#10816,.T.);
#15474=ORIENTED_EDGE('',*,*,#10817,.T.);
#15475=ORIENTED_EDGE('',*,*,#10818,.T.);
#15476=ORIENTED_EDGE('',*,*,#10819,.F.);
#15477=ORIENTED_EDGE('',*,*,#10820,.T.);
#15478=ORIENTED_EDGE('',*,*,#10821,.T.);
#15479=ORIENTED_EDGE('',*,*,#10822,.T.);
#15480=ORIENTED_EDGE('',*,*,#10823,.F.);
#15481=ORIENTED_EDGE('',*,*,#10824,.T.);
#15482=ORIENTED_EDGE('',*,*,#10825,.T.);
#15483=ORIENTED_EDGE('',*,*,#10826,.T.);
#15484=ORIENTED_EDGE('',*,*,#10827,.F.);
#15485=ORIENTED_EDGE('',*,*,#10828,.T.);
#15486=ORIENTED_EDGE('',*,*,#10829,.T.);
#15487=ORIENTED_EDGE('',*,*,#10830,.T.);
#15488=ORIENTED_EDGE('',*,*,#10831,.F.);
#15489=ORIENTED_EDGE('',*,*,#10832,.T.);
#15490=ORIENTED_EDGE('',*,*,#10833,.T.);
#15491=ORIENTED_EDGE('',*,*,#10834,.T.);
#15492=ORIENTED_EDGE('',*,*,#10835,.F.);
#15493=ORIENTED_EDGE('',*,*,#10836,.T.);
#15494=ORIENTED_EDGE('',*,*,#10837,.T.);
#15495=ORIENTED_EDGE('',*,*,#10838,.T.);
#15496=ORIENTED_EDGE('',*,*,#10839,.F.);
#15497=ORIENTED_EDGE('',*,*,#10840,.T.);
#15498=ORIENTED_EDGE('',*,*,#10841,.T.);
#15499=ORIENTED_EDGE('',*,*,#10842,.T.);
#15500=ORIENTED_EDGE('',*,*,#10843,.F.);
#15501=ORIENTED_EDGE('',*,*,#10844,.T.);
#15502=ORIENTED_EDGE('',*,*,#10845,.T.);
#15503=ORIENTED_EDGE('',*,*,#10846,.T.);
#15504=ORIENTED_EDGE('',*,*,#10847,.F.);
#15505=ORIENTED_EDGE('',*,*,#10848,.T.);
#15506=ORIENTED_EDGE('',*,*,#10849,.T.);
#15507=ORIENTED_EDGE('',*,*,#10850,.T.);
#15508=ORIENTED_EDGE('',*,*,#10851,.F.);
#15509=ORIENTED_EDGE('',*,*,#10852,.T.);
#15510=ORIENTED_EDGE('',*,*,#10853,.T.);
#15511=ORIENTED_EDGE('',*,*,#10854,.T.);
#15512=ORIENTED_EDGE('',*,*,#10855,.F.);
#15513=ORIENTED_EDGE('',*,*,#10856,.T.);
#15514=ORIENTED_EDGE('',*,*,#10857,.T.);
#15515=ORIENTED_EDGE('',*,*,#10858,.T.);
#15516=ORIENTED_EDGE('',*,*,#10859,.F.);
#15517=ORIENTED_EDGE('',*,*,#10860,.T.);
#15518=ORIENTED_EDGE('',*,*,#10861,.T.);
#15519=ORIENTED_EDGE('',*,*,#10862,.T.);
#15520=ORIENTED_EDGE('',*,*,#10863,.F.);
#15521=ORIENTED_EDGE('',*,*,#10864,.T.);
#15522=ORIENTED_EDGE('',*,*,#10865,.T.);
#15523=ORIENTED_EDGE('',*,*,#10866,.T.);
#15524=ORIENTED_EDGE('',*,*,#10867,.F.);
#15525=ORIENTED_EDGE('',*,*,#10868,.T.);
#15526=ORIENTED_EDGE('',*,*,#10869,.T.);
#15527=ORIENTED_EDGE('',*,*,#10870,.T.);
#15528=ORIENTED_EDGE('',*,*,#10871,.F.);
#15529=ORIENTED_EDGE('',*,*,#10872,.T.);
#15530=ORIENTED_EDGE('',*,*,#10873,.T.);
#15531=ORIENTED_EDGE('',*,*,#10874,.T.);
#15532=ORIENTED_EDGE('',*,*,#10875,.F.);
#15533=ORIENTED_EDGE('',*,*,#10876,.T.);
#15534=ORIENTED_EDGE('',*,*,#10877,.T.);
#15535=ORIENTED_EDGE('',*,*,#10878,.T.);
#15536=ORIENTED_EDGE('',*,*,#10879,.F.);
#15537=ORIENTED_EDGE('',*,*,#10778,.F.);
#15538=ORIENTED_EDGE('',*,*,#10880,.F.);
#15539=ORIENTED_EDGE('',*,*,#10724,.F.);
#15540=ORIENTED_EDGE('',*,*,#10881,.F.);
#15541=ORIENTED_EDGE('',*,*,#10882,.T.);
#15542=ORIENTED_EDGE('',*,*,#10883,.F.);
#15543=ORIENTED_EDGE('',*,*,#10884,.T.);
#15544=ORIENTED_EDGE('',*,*,#10881,.T.);
#15545=ORIENTED_EDGE('',*,*,#10723,.F.);
#15546=ORIENTED_EDGE('',*,*,#10885,.F.);
#15547=ORIENTED_EDGE('',*,*,#10886,.F.);
#15548=ORIENTED_EDGE('',*,*,#10887,.F.);
#15549=ORIENTED_EDGE('',*,*,#10888,.T.);
#15550=ORIENTED_EDGE('',*,*,#10885,.T.);
#15551=ORIENTED_EDGE('',*,*,#10722,.F.);
#15552=ORIENTED_EDGE('',*,*,#10880,.T.);
#15553=ORIENTED_EDGE('',*,*,#10889,.T.);
#15554=ORIENTED_EDGE('',*,*,#10890,.T.);
#15555=ORIENTED_EDGE('',*,*,#10725,.F.);
#15556=ORIENTED_EDGE('',*,*,#10883,.T.);
#15557=ORIENTED_EDGE('',*,*,#10891,.T.);
#15558=ORIENTED_EDGE('',*,*,#10892,.T.);
#15559=ORIENTED_EDGE('',*,*,#10889,.F.);
#15560=ORIENTED_EDGE('',*,*,#10893,.F.);
#15561=ORIENTED_EDGE('',*,*,#10894,.T.);
#15562=ORIENTED_EDGE('',*,*,#10895,.T.);
#15563=ORIENTED_EDGE('',*,*,#10774,.F.);
#15564=ORIENTED_EDGE('',*,*,#10896,.F.);
#15565=ORIENTED_EDGE('',*,*,#10897,.T.);
#15566=ORIENTED_EDGE('',*,*,#10898,.T.);
#15567=ORIENTED_EDGE('',*,*,#10775,.F.);
#15568=ORIENTED_EDGE('',*,*,#10895,.F.);
#15569=ORIENTED_EDGE('',*,*,#10899,.F.);
#15570=ORIENTED_EDGE('',*,*,#10900,.F.);
#15571=ORIENTED_EDGE('',*,*,#10776,.F.);
#15572=ORIENTED_EDGE('',*,*,#10898,.F.);
#15573=ORIENTED_EDGE('',*,*,#10901,.T.);
#15574=ORIENTED_EDGE('',*,*,#10902,.T.);
#15575=ORIENTED_EDGE('',*,*,#10903,.T.);
#15576=ORIENTED_EDGE('',*,*,#10904,.T.);
#15577=ORIENTED_EDGE('',*,*,#10905,.T.);
#15578=ORIENTED_EDGE('',*,*,#10906,.T.);
#15579=ORIENTED_EDGE('',*,*,#10907,.T.);
#15580=ORIENTED_EDGE('',*,*,#10908,.T.);
#15581=ORIENTED_EDGE('',*,*,#10909,.T.);
#15582=ORIENTED_EDGE('',*,*,#10910,.T.);
#15583=ORIENTED_EDGE('',*,*,#10911,.T.);
#15584=ORIENTED_EDGE('',*,*,#10912,.T.);
#15585=ORIENTED_EDGE('',*,*,#10913,.T.);
#15586=ORIENTED_EDGE('',*,*,#10914,.T.);
#15587=ORIENTED_EDGE('',*,*,#10915,.T.);
#15588=ORIENTED_EDGE('',*,*,#10916,.T.);
#15589=ORIENTED_EDGE('',*,*,#10917,.T.);
#15590=ORIENTED_EDGE('',*,*,#10918,.T.);
#15591=ORIENTED_EDGE('',*,*,#10919,.T.);
#15592=ORIENTED_EDGE('',*,*,#10920,.T.);
#15593=ORIENTED_EDGE('',*,*,#10921,.T.);
#15594=ORIENTED_EDGE('',*,*,#10922,.T.);
#15595=ORIENTED_EDGE('',*,*,#10923,.T.);
#15596=ORIENTED_EDGE('',*,*,#10924,.T.);
#15597=ORIENTED_EDGE('',*,*,#10925,.T.);
#15598=ORIENTED_EDGE('',*,*,#10926,.T.);
#15599=ORIENTED_EDGE('',*,*,#10927,.T.);
#15600=ORIENTED_EDGE('',*,*,#10928,.T.);
#15601=ORIENTED_EDGE('',*,*,#10929,.T.);
#15602=ORIENTED_EDGE('',*,*,#10930,.T.);
#15603=ORIENTED_EDGE('',*,*,#10931,.T.);
#15604=ORIENTED_EDGE('',*,*,#10932,.T.);
#15605=ORIENTED_EDGE('',*,*,#10933,.T.);
#15606=ORIENTED_EDGE('',*,*,#10934,.T.);
#15607=ORIENTED_EDGE('',*,*,#10935,.T.);
#15608=ORIENTED_EDGE('',*,*,#10936,.T.);
#15609=ORIENTED_EDGE('',*,*,#10937,.T.);
#15610=ORIENTED_EDGE('',*,*,#10938,.T.);
#15611=ORIENTED_EDGE('',*,*,#10939,.T.);
#15612=ORIENTED_EDGE('',*,*,#10940,.T.);
#15613=ORIENTED_EDGE('',*,*,#10941,.T.);
#15614=ORIENTED_EDGE('',*,*,#10942,.T.);
#15615=ORIENTED_EDGE('',*,*,#10943,.T.);
#15616=ORIENTED_EDGE('',*,*,#10944,.T.);
#15617=ORIENTED_EDGE('',*,*,#10945,.T.);
#15618=ORIENTED_EDGE('',*,*,#10946,.T.);
#15619=ORIENTED_EDGE('',*,*,#10947,.T.);
#15620=ORIENTED_EDGE('',*,*,#10948,.T.);
#15621=ORIENTED_EDGE('',*,*,#10949,.T.);
#15622=ORIENTED_EDGE('',*,*,#10950,.T.);
#15623=ORIENTED_EDGE('',*,*,#10951,.T.);
#15624=ORIENTED_EDGE('',*,*,#10952,.T.);
#15625=ORIENTED_EDGE('',*,*,#10953,.T.);
#15626=ORIENTED_EDGE('',*,*,#10954,.T.);
#15627=ORIENTED_EDGE('',*,*,#10955,.T.);
#15628=ORIENTED_EDGE('',*,*,#10956,.T.);
#15629=ORIENTED_EDGE('',*,*,#10957,.T.);
#15630=ORIENTED_EDGE('',*,*,#10958,.T.);
#15631=ORIENTED_EDGE('',*,*,#10959,.T.);
#15632=ORIENTED_EDGE('',*,*,#10960,.T.);
#15633=ORIENTED_EDGE('',*,*,#10961,.T.);
#15634=ORIENTED_EDGE('',*,*,#10962,.T.);
#15635=ORIENTED_EDGE('',*,*,#10963,.T.);
#15636=ORIENTED_EDGE('',*,*,#10964,.T.);
#15637=ORIENTED_EDGE('',*,*,#10965,.T.);
#15638=ORIENTED_EDGE('',*,*,#10966,.T.);
#15639=ORIENTED_EDGE('',*,*,#10967,.T.);
#15640=ORIENTED_EDGE('',*,*,#10968,.T.);
#15641=ORIENTED_EDGE('',*,*,#10969,.T.);
#15642=ORIENTED_EDGE('',*,*,#10970,.T.);
#15643=ORIENTED_EDGE('',*,*,#10971,.T.);
#15644=ORIENTED_EDGE('',*,*,#10972,.T.);
#15645=ORIENTED_EDGE('',*,*,#10973,.T.);
#15646=ORIENTED_EDGE('',*,*,#10974,.T.);
#15647=ORIENTED_EDGE('',*,*,#10975,.T.);
#15648=ORIENTED_EDGE('',*,*,#10976,.T.);
#15649=ORIENTED_EDGE('',*,*,#10977,.T.);
#15650=ORIENTED_EDGE('',*,*,#10978,.T.);
#15651=ORIENTED_EDGE('',*,*,#10979,.T.);
#15652=ORIENTED_EDGE('',*,*,#10980,.T.);
#15653=ORIENTED_EDGE('',*,*,#10981,.T.);
#15654=ORIENTED_EDGE('',*,*,#10982,.T.);
#15655=ORIENTED_EDGE('',*,*,#10983,.T.);
#15656=ORIENTED_EDGE('',*,*,#10984,.T.);
#15657=ORIENTED_EDGE('',*,*,#10985,.T.);
#15658=ORIENTED_EDGE('',*,*,#10986,.T.);
#15659=ORIENTED_EDGE('',*,*,#10987,.T.);
#15660=ORIENTED_EDGE('',*,*,#10988,.T.);
#15661=ORIENTED_EDGE('',*,*,#10989,.T.);
#15662=ORIENTED_EDGE('',*,*,#10990,.T.);
#15663=ORIENTED_EDGE('',*,*,#10991,.T.);
#15664=ORIENTED_EDGE('',*,*,#10992,.T.);
#15665=ORIENTED_EDGE('',*,*,#10993,.T.);
#15666=ORIENTED_EDGE('',*,*,#10994,.T.);
#15667=ORIENTED_EDGE('',*,*,#10995,.T.);
#15668=ORIENTED_EDGE('',*,*,#10996,.T.);
#15669=ORIENTED_EDGE('',*,*,#10997,.T.);
#15670=ORIENTED_EDGE('',*,*,#10998,.T.);
#15671=ORIENTED_EDGE('',*,*,#10999,.T.);
#15672=ORIENTED_EDGE('',*,*,#11000,.T.);
#15673=ORIENTED_EDGE('',*,*,#11001,.T.);
#15674=ORIENTED_EDGE('',*,*,#11002,.F.);
#15675=ORIENTED_EDGE('',*,*,#10901,.F.);
#15676=ORIENTED_EDGE('',*,*,#10897,.F.);
#15677=ORIENTED_EDGE('',*,*,#10894,.F.);
#15678=ORIENTED_EDGE('',*,*,#11003,.F.);
#15679=ORIENTED_EDGE('',*,*,#11004,.F.);
#15680=ORIENTED_EDGE('',*,*,#11005,.F.);
#15681=ORIENTED_EDGE('',*,*,#11006,.F.);
#15682=ORIENTED_EDGE('',*,*,#11007,.F.);
#15683=ORIENTED_EDGE('',*,*,#11008,.F.);
#15684=ORIENTED_EDGE('',*,*,#11009,.F.);
#15685=ORIENTED_EDGE('',*,*,#11010,.F.);
#15686=ORIENTED_EDGE('',*,*,#11011,.F.);
#15687=ORIENTED_EDGE('',*,*,#11012,.F.);
#15688=ORIENTED_EDGE('',*,*,#11013,.F.);
#15689=ORIENTED_EDGE('',*,*,#11014,.F.);
#15690=ORIENTED_EDGE('',*,*,#11015,.F.);
#15691=ORIENTED_EDGE('',*,*,#11016,.F.);
#15692=ORIENTED_EDGE('',*,*,#11017,.F.);
#15693=ORIENTED_EDGE('',*,*,#11018,.F.);
#15694=ORIENTED_EDGE('',*,*,#11019,.F.);
#15695=ORIENTED_EDGE('',*,*,#11020,.F.);
#15696=ORIENTED_EDGE('',*,*,#11021,.F.);
#15697=ORIENTED_EDGE('',*,*,#11022,.F.);
#15698=ORIENTED_EDGE('',*,*,#11023,.F.);
#15699=ORIENTED_EDGE('',*,*,#11024,.F.);
#15700=ORIENTED_EDGE('',*,*,#11025,.F.);
#15701=ORIENTED_EDGE('',*,*,#11026,.F.);
#15702=ORIENTED_EDGE('',*,*,#11027,.F.);
#15703=ORIENTED_EDGE('',*,*,#11028,.F.);
#15704=ORIENTED_EDGE('',*,*,#11029,.F.);
#15705=ORIENTED_EDGE('',*,*,#11030,.F.);
#15706=ORIENTED_EDGE('',*,*,#11031,.F.);
#15707=ORIENTED_EDGE('',*,*,#11032,.F.);
#15708=ORIENTED_EDGE('',*,*,#11033,.F.);
#15709=ORIENTED_EDGE('',*,*,#11034,.F.);
#15710=ORIENTED_EDGE('',*,*,#11035,.F.);
#15711=ORIENTED_EDGE('',*,*,#11036,.F.);
#15712=ORIENTED_EDGE('',*,*,#11037,.F.);
#15713=ORIENTED_EDGE('',*,*,#11038,.F.);
#15714=ORIENTED_EDGE('',*,*,#11039,.F.);
#15715=ORIENTED_EDGE('',*,*,#11040,.F.);
#15716=ORIENTED_EDGE('',*,*,#11041,.F.);
#15717=ORIENTED_EDGE('',*,*,#11042,.F.);
#15718=ORIENTED_EDGE('',*,*,#11043,.F.);
#15719=ORIENTED_EDGE('',*,*,#11044,.F.);
#15720=ORIENTED_EDGE('',*,*,#11045,.F.);
#15721=ORIENTED_EDGE('',*,*,#11046,.F.);
#15722=ORIENTED_EDGE('',*,*,#11047,.F.);
#15723=ORIENTED_EDGE('',*,*,#11048,.F.);
#15724=ORIENTED_EDGE('',*,*,#11049,.F.);
#15725=ORIENTED_EDGE('',*,*,#11050,.F.);
#15726=ORIENTED_EDGE('',*,*,#10891,.F.);
#15727=ORIENTED_EDGE('',*,*,#10882,.F.);
#15728=ORIENTED_EDGE('',*,*,#10884,.F.);
#15729=ORIENTED_EDGE('',*,*,#10888,.F.);
#15730=ORIENTED_EDGE('',*,*,#10893,.T.);
#15731=ORIENTED_EDGE('',*,*,#11051,.F.);
#15732=ORIENTED_EDGE('',*,*,#11052,.T.);
#15733=ORIENTED_EDGE('',*,*,#11003,.T.);
#15734=ORIENTED_EDGE('',*,*,#10896,.T.);
#15735=ORIENTED_EDGE('',*,*,#10773,.F.);
#15736=ORIENTED_EDGE('',*,*,#11053,.T.);
#15737=ORIENTED_EDGE('',*,*,#11051,.T.);
#15738=ORIENTED_EDGE('',*,*,#11053,.F.);
#15739=ORIENTED_EDGE('',*,*,#10772,.F.);
#15740=ORIENTED_EDGE('',*,*,#11054,.F.);
#15741=ORIENTED_EDGE('',*,*,#11004,.T.);
#15742=ORIENTED_EDGE('',*,*,#11052,.F.);
#15743=ORIENTED_EDGE('',*,*,#11005,.T.);
#15744=ORIENTED_EDGE('',*,*,#11054,.T.);
#15745=ORIENTED_EDGE('',*,*,#10771,.F.);
#15746=ORIENTED_EDGE('',*,*,#11055,.F.);
#15747=ORIENTED_EDGE('',*,*,#11056,.F.);
#15748=ORIENTED_EDGE('',*,*,#11057,.F.);
#15749=ORIENTED_EDGE('',*,*,#11006,.T.);
#15750=ORIENTED_EDGE('',*,*,#11055,.T.);
#15751=ORIENTED_EDGE('',*,*,#10770,.F.);
#15752=ORIENTED_EDGE('',*,*,#10886,.T.);
#15753=ORIENTED_EDGE('',*,*,#10777,.F.);
#15754=ORIENTED_EDGE('',*,*,#10900,.T.);
#15755=ORIENTED_EDGE('',*,*,#11058,.T.);
#15756=ORIENTED_EDGE('',*,*,#10887,.T.);
#15757=ORIENTED_EDGE('',*,*,#11058,.F.);
#15758=ORIENTED_EDGE('',*,*,#10899,.T.);
#15759=ORIENTED_EDGE('',*,*,#11002,.T.);
#15760=ORIENTED_EDGE('',*,*,#11059,.F.);
#15761=ORIENTED_EDGE('',*,*,#11010,.T.);
#15762=ORIENTED_EDGE('',*,*,#11060,.T.);
#15763=ORIENTED_EDGE('',*,*,#10766,.F.);
#15764=ORIENTED_EDGE('',*,*,#11061,.F.);
#15765=ORIENTED_EDGE('',*,*,#11009,.T.);
#15766=ORIENTED_EDGE('',*,*,#11062,.T.);
#15767=ORIENTED_EDGE('',*,*,#10767,.F.);
#15768=ORIENTED_EDGE('',*,*,#11060,.F.);
#15769=ORIENTED_EDGE('',*,*,#11063,.F.);
#15770=ORIENTED_EDGE('',*,*,#11064,.F.);
#15771=ORIENTED_EDGE('',*,*,#10768,.F.);
#15772=ORIENTED_EDGE('',*,*,#11062,.F.);
#15773=ORIENTED_EDGE('',*,*,#11008,.T.);
#15774=ORIENTED_EDGE('',*,*,#11059,.T.);
#15775=ORIENTED_EDGE('',*,*,#11065,.F.);
#15776=ORIENTED_EDGE('',*,*,#11066,.T.);
#15777=ORIENTED_EDGE('',*,*,#11011,.T.);
#15778=ORIENTED_EDGE('',*,*,#11061,.T.);
#15779=ORIENTED_EDGE('',*,*,#10765,.F.);
#15780=ORIENTED_EDGE('',*,*,#11067,.T.);
#15781=ORIENTED_EDGE('',*,*,#11065,.T.);
#15782=ORIENTED_EDGE('',*,*,#11067,.F.);
#15783=ORIENTED_EDGE('',*,*,#10764,.F.);
#15784=ORIENTED_EDGE('',*,*,#11068,.F.);
#15785=ORIENTED_EDGE('',*,*,#11012,.T.);
#15786=ORIENTED_EDGE('',*,*,#11066,.F.);
#15787=ORIENTED_EDGE('',*,*,#11013,.T.);
#15788=ORIENTED_EDGE('',*,*,#11068,.T.);
#15789=ORIENTED_EDGE('',*,*,#10763,.F.);
#15790=ORIENTED_EDGE('',*,*,#11069,.F.);
#15791=ORIENTED_EDGE('',*,*,#11070,.F.);
#15792=ORIENTED_EDGE('',*,*,#11071,.F.);
#15793=ORIENTED_EDGE('',*,*,#11014,.T.);
#15794=ORIENTED_EDGE('',*,*,#11069,.T.);
#15795=ORIENTED_EDGE('',*,*,#10762,.F.);
#15796=ORIENTED_EDGE('',*,*,#11056,.T.);
#15797=ORIENTED_EDGE('',*,*,#10769,.F.);
#15798=ORIENTED_EDGE('',*,*,#11064,.T.);
#15799=ORIENTED_EDGE('',*,*,#11072,.T.);
#15800=ORIENTED_EDGE('',*,*,#11057,.T.);
#15801=ORIENTED_EDGE('',*,*,#11072,.F.);
#15802=ORIENTED_EDGE('',*,*,#11063,.T.);
#15803=ORIENTED_EDGE('',*,*,#11007,.T.);
#15804=ORIENTED_EDGE('',*,*,#11073,.F.);
#15805=ORIENTED_EDGE('',*,*,#11018,.T.);
#15806=ORIENTED_EDGE('',*,*,#11074,.T.);
#15807=ORIENTED_EDGE('',*,*,#10758,.F.);
#15808=ORIENTED_EDGE('',*,*,#11075,.F.);
#15809=ORIENTED_EDGE('',*,*,#11017,.T.);
#15810=ORIENTED_EDGE('',*,*,#11076,.T.);
#15811=ORIENTED_EDGE('',*,*,#10759,.F.);
#15812=ORIENTED_EDGE('',*,*,#11074,.F.);
#15813=ORIENTED_EDGE('',*,*,#11077,.F.);
#15814=ORIENTED_EDGE('',*,*,#11078,.F.);
#15815=ORIENTED_EDGE('',*,*,#10760,.F.);
#15816=ORIENTED_EDGE('',*,*,#11076,.F.);
#15817=ORIENTED_EDGE('',*,*,#11016,.T.);
#15818=ORIENTED_EDGE('',*,*,#11073,.T.);
#15819=ORIENTED_EDGE('',*,*,#11079,.F.);
#15820=ORIENTED_EDGE('',*,*,#11080,.T.);
#15821=ORIENTED_EDGE('',*,*,#11019,.T.);
#15822=ORIENTED_EDGE('',*,*,#11075,.T.);
#15823=ORIENTED_EDGE('',*,*,#10757,.F.);
#15824=ORIENTED_EDGE('',*,*,#11081,.T.);
#15825=ORIENTED_EDGE('',*,*,#11079,.T.);
#15826=ORIENTED_EDGE('',*,*,#11081,.F.);
#15827=ORIENTED_EDGE('',*,*,#10756,.F.);
#15828=ORIENTED_EDGE('',*,*,#11082,.F.);
#15829=ORIENTED_EDGE('',*,*,#11020,.T.);
#15830=ORIENTED_EDGE('',*,*,#11080,.F.);
#15831=ORIENTED_EDGE('',*,*,#11021,.T.);
#15832=ORIENTED_EDGE('',*,*,#11082,.T.);
#15833=ORIENTED_EDGE('',*,*,#10755,.F.);
#15834=ORIENTED_EDGE('',*,*,#11083,.F.);
#15835=ORIENTED_EDGE('',*,*,#11084,.F.);
#15836=ORIENTED_EDGE('',*,*,#11085,.F.);
#15837=ORIENTED_EDGE('',*,*,#11022,.T.);
#15838=ORIENTED_EDGE('',*,*,#11083,.T.);
#15839=ORIENTED_EDGE('',*,*,#10754,.F.);
#15840=ORIENTED_EDGE('',*,*,#11070,.T.);
#15841=ORIENTED_EDGE('',*,*,#10761,.F.);
#15842=ORIENTED_EDGE('',*,*,#11078,.T.);
#15843=ORIENTED_EDGE('',*,*,#11086,.T.);
#15844=ORIENTED_EDGE('',*,*,#11071,.T.);
#15845=ORIENTED_EDGE('',*,*,#11086,.F.);
#15846=ORIENTED_EDGE('',*,*,#11077,.T.);
#15847=ORIENTED_EDGE('',*,*,#11015,.T.);
#15848=ORIENTED_EDGE('',*,*,#11087,.F.);
#15849=ORIENTED_EDGE('',*,*,#11026,.T.);
#15850=ORIENTED_EDGE('',*,*,#11088,.T.);
#15851=ORIENTED_EDGE('',*,*,#10750,.F.);
#15852=ORIENTED_EDGE('',*,*,#11089,.F.);
#15853=ORIENTED_EDGE('',*,*,#11025,.T.);
#15854=ORIENTED_EDGE('',*,*,#11090,.T.);
#15855=ORIENTED_EDGE('',*,*,#10751,.F.);
#15856=ORIENTED_EDGE('',*,*,#11088,.F.);
#15857=ORIENTED_EDGE('',*,*,#11091,.F.);
#15858=ORIENTED_EDGE('',*,*,#11092,.F.);
#15859=ORIENTED_EDGE('',*,*,#10752,.F.);
#15860=ORIENTED_EDGE('',*,*,#11090,.F.);
#15861=ORIENTED_EDGE('',*,*,#11024,.T.);
#15862=ORIENTED_EDGE('',*,*,#11087,.T.);
#15863=ORIENTED_EDGE('',*,*,#11093,.F.);
#15864=ORIENTED_EDGE('',*,*,#11094,.T.);
#15865=ORIENTED_EDGE('',*,*,#11027,.T.);
#15866=ORIENTED_EDGE('',*,*,#11089,.T.);
#15867=ORIENTED_EDGE('',*,*,#10749,.F.);
#15868=ORIENTED_EDGE('',*,*,#11095,.T.);
#15869=ORIENTED_EDGE('',*,*,#11093,.T.);
#15870=ORIENTED_EDGE('',*,*,#11095,.F.);
#15871=ORIENTED_EDGE('',*,*,#10748,.F.);
#15872=ORIENTED_EDGE('',*,*,#11096,.F.);
#15873=ORIENTED_EDGE('',*,*,#11028,.T.);
#15874=ORIENTED_EDGE('',*,*,#11094,.F.);
#15875=ORIENTED_EDGE('',*,*,#11029,.T.);
#15876=ORIENTED_EDGE('',*,*,#11096,.T.);
#15877=ORIENTED_EDGE('',*,*,#10747,.F.);
#15878=ORIENTED_EDGE('',*,*,#11097,.F.);
#15879=ORIENTED_EDGE('',*,*,#11098,.F.);
#15880=ORIENTED_EDGE('',*,*,#11099,.F.);
#15881=ORIENTED_EDGE('',*,*,#11030,.T.);
#15882=ORIENTED_EDGE('',*,*,#11097,.T.);
#15883=ORIENTED_EDGE('',*,*,#10746,.F.);
#15884=ORIENTED_EDGE('',*,*,#11084,.T.);
#15885=ORIENTED_EDGE('',*,*,#10753,.F.);
#15886=ORIENTED_EDGE('',*,*,#11092,.T.);
#15887=ORIENTED_EDGE('',*,*,#11100,.T.);
#15888=ORIENTED_EDGE('',*,*,#11085,.T.);
#15889=ORIENTED_EDGE('',*,*,#11100,.F.);
#15890=ORIENTED_EDGE('',*,*,#11091,.T.);
#15891=ORIENTED_EDGE('',*,*,#11023,.T.);
#15892=ORIENTED_EDGE('',*,*,#11101,.F.);
#15893=ORIENTED_EDGE('',*,*,#11034,.T.);
#15894=ORIENTED_EDGE('',*,*,#11102,.T.);
#15895=ORIENTED_EDGE('',*,*,#10742,.F.);
#15896=ORIENTED_EDGE('',*,*,#11103,.F.);
#15897=ORIENTED_EDGE('',*,*,#11033,.T.);
#15898=ORIENTED_EDGE('',*,*,#11104,.T.);
#15899=ORIENTED_EDGE('',*,*,#10743,.F.);
#15900=ORIENTED_EDGE('',*,*,#11102,.F.);
#15901=ORIENTED_EDGE('',*,*,#11105,.F.);
#15902=ORIENTED_EDGE('',*,*,#11106,.F.);
#15903=ORIENTED_EDGE('',*,*,#10744,.F.);
#15904=ORIENTED_EDGE('',*,*,#11104,.F.);
#15905=ORIENTED_EDGE('',*,*,#11032,.T.);
#15906=ORIENTED_EDGE('',*,*,#11101,.T.);
#15907=ORIENTED_EDGE('',*,*,#11107,.F.);
#15908=ORIENTED_EDGE('',*,*,#11108,.T.);
#15909=ORIENTED_EDGE('',*,*,#11035,.T.);
#15910=ORIENTED_EDGE('',*,*,#11103,.T.);
#15911=ORIENTED_EDGE('',*,*,#10741,.F.);
#15912=ORIENTED_EDGE('',*,*,#11109,.T.);
#15913=ORIENTED_EDGE('',*,*,#11107,.T.);
#15914=ORIENTED_EDGE('',*,*,#11109,.F.);
#15915=ORIENTED_EDGE('',*,*,#10740,.F.);
#15916=ORIENTED_EDGE('',*,*,#11110,.F.);
#15917=ORIENTED_EDGE('',*,*,#11036,.T.);
#15918=ORIENTED_EDGE('',*,*,#11108,.F.);
#15919=ORIENTED_EDGE('',*,*,#11037,.T.);
#15920=ORIENTED_EDGE('',*,*,#11110,.T.);
#15921=ORIENTED_EDGE('',*,*,#10739,.F.);
#15922=ORIENTED_EDGE('',*,*,#11111,.F.);
#15923=ORIENTED_EDGE('',*,*,#11112,.F.);
#15924=ORIENTED_EDGE('',*,*,#11113,.F.);
#15925=ORIENTED_EDGE('',*,*,#11038,.T.);
#15926=ORIENTED_EDGE('',*,*,#11111,.T.);
#15927=ORIENTED_EDGE('',*,*,#10738,.F.);
#15928=ORIENTED_EDGE('',*,*,#11098,.T.);
#15929=ORIENTED_EDGE('',*,*,#10745,.F.);
#15930=ORIENTED_EDGE('',*,*,#11106,.T.);
#15931=ORIENTED_EDGE('',*,*,#11114,.T.);
#15932=ORIENTED_EDGE('',*,*,#11099,.T.);
#15933=ORIENTED_EDGE('',*,*,#11114,.F.);
#15934=ORIENTED_EDGE('',*,*,#11105,.T.);
#15935=ORIENTED_EDGE('',*,*,#11031,.T.);
#15936=ORIENTED_EDGE('',*,*,#11115,.F.);
#15937=ORIENTED_EDGE('',*,*,#11042,.T.);
#15938=ORIENTED_EDGE('',*,*,#11116,.T.);
#15939=ORIENTED_EDGE('',*,*,#10734,.F.);
#15940=ORIENTED_EDGE('',*,*,#11117,.F.);
#15941=ORIENTED_EDGE('',*,*,#11041,.T.);
#15942=ORIENTED_EDGE('',*,*,#11118,.T.);
#15943=ORIENTED_EDGE('',*,*,#10735,.F.);
#15944=ORIENTED_EDGE('',*,*,#11116,.F.);
#15945=ORIENTED_EDGE('',*,*,#11119,.F.);
#15946=ORIENTED_EDGE('',*,*,#11120,.F.);
#15947=ORIENTED_EDGE('',*,*,#10736,.F.);
#15948=ORIENTED_EDGE('',*,*,#11118,.F.);
#15949=ORIENTED_EDGE('',*,*,#11040,.T.);
#15950=ORIENTED_EDGE('',*,*,#11115,.T.);
#15951=ORIENTED_EDGE('',*,*,#11121,.F.);
#15952=ORIENTED_EDGE('',*,*,#11122,.T.);
#15953=ORIENTED_EDGE('',*,*,#11043,.T.);
#15954=ORIENTED_EDGE('',*,*,#11117,.T.);
#15955=ORIENTED_EDGE('',*,*,#10733,.F.);
#15956=ORIENTED_EDGE('',*,*,#11123,.T.);
#15957=ORIENTED_EDGE('',*,*,#11121,.T.);
#15958=ORIENTED_EDGE('',*,*,#11123,.F.);
#15959=ORIENTED_EDGE('',*,*,#10732,.F.);
#15960=ORIENTED_EDGE('',*,*,#11124,.F.);
#15961=ORIENTED_EDGE('',*,*,#11044,.T.);
#15962=ORIENTED_EDGE('',*,*,#11122,.F.);
#15963=ORIENTED_EDGE('',*,*,#11045,.T.);
#15964=ORIENTED_EDGE('',*,*,#11124,.T.);
#15965=ORIENTED_EDGE('',*,*,#10731,.F.);
#15966=ORIENTED_EDGE('',*,*,#11125,.F.);
#15967=ORIENTED_EDGE('',*,*,#11126,.F.);
#15968=ORIENTED_EDGE('',*,*,#11127,.F.);
#15969=ORIENTED_EDGE('',*,*,#11046,.T.);
#15970=ORIENTED_EDGE('',*,*,#11125,.T.);
#15971=ORIENTED_EDGE('',*,*,#10730,.F.);
#15972=ORIENTED_EDGE('',*,*,#11112,.T.);
#15973=ORIENTED_EDGE('',*,*,#10737,.F.);
#15974=ORIENTED_EDGE('',*,*,#11120,.T.);
#15975=ORIENTED_EDGE('',*,*,#11128,.T.);
#15976=ORIENTED_EDGE('',*,*,#11113,.T.);
#15977=ORIENTED_EDGE('',*,*,#11128,.F.);
#15978=ORIENTED_EDGE('',*,*,#11119,.T.);
#15979=ORIENTED_EDGE('',*,*,#11039,.T.);
#15980=ORIENTED_EDGE('',*,*,#11129,.F.);
#15981=ORIENTED_EDGE('',*,*,#10728,.F.);
#15982=ORIENTED_EDGE('',*,*,#11130,.F.);
#15983=ORIENTED_EDGE('',*,*,#11048,.T.);
#15984=ORIENTED_EDGE('',*,*,#11131,.F.);
#15985=ORIENTED_EDGE('',*,*,#11049,.T.);
#15986=ORIENTED_EDGE('',*,*,#11130,.T.);
#15987=ORIENTED_EDGE('',*,*,#10727,.F.);
#15988=ORIENTED_EDGE('',*,*,#11132,.F.);
#15989=ORIENTED_EDGE('',*,*,#10890,.F.);
#15990=ORIENTED_EDGE('',*,*,#10892,.F.);
#15991=ORIENTED_EDGE('',*,*,#11050,.T.);
#15992=ORIENTED_EDGE('',*,*,#11132,.T.);
#15993=ORIENTED_EDGE('',*,*,#10726,.F.);
#15994=ORIENTED_EDGE('',*,*,#11133,.F.);
#15995=ORIENTED_EDGE('',*,*,#10782,.F.);
#15996=ORIENTED_EDGE('',*,*,#11134,.T.);
#15997=ORIENTED_EDGE('',*,*,#11000,.F.);
#15998=ORIENTED_EDGE('',*,*,#11135,.F.);
#15999=ORIENTED_EDGE('',*,*,#11136,.F.);
#16000=ORIENTED_EDGE('',*,*,#10781,.F.);
#16001=ORIENTED_EDGE('',*,*,#11137,.T.);
#16002=ORIENTED_EDGE('',*,*,#11001,.F.);
#16003=ORIENTED_EDGE('',*,*,#11134,.F.);
#16004=ORIENTED_EDGE('',*,*,#11138,.F.);
#16005=ORIENTED_EDGE('',*,*,#11139,.F.);
#16006=ORIENTED_EDGE('',*,*,#11140,.F.);
#16007=ORIENTED_EDGE('',*,*,#10902,.F.);
#16008=ORIENTED_EDGE('',*,*,#11137,.F.);
#16009=ORIENTED_EDGE('',*,*,#10780,.F.);
#16010=ORIENTED_EDGE('',*,*,#11133,.T.);
#16011=ORIENTED_EDGE('',*,*,#11141,.F.);
#16012=ORIENTED_EDGE('',*,*,#11142,.T.);
#16013=ORIENTED_EDGE('',*,*,#10783,.T.);
#16014=ORIENTED_EDGE('',*,*,#11136,.T.);
#16015=ORIENTED_EDGE('',*,*,#11143,.F.);
#16016=ORIENTED_EDGE('',*,*,#11144,.T.);
#16017=ORIENTED_EDGE('',*,*,#11141,.T.);
#16018=ORIENTED_EDGE('',*,*,#11135,.T.);
#16019=ORIENTED_EDGE('',*,*,#10999,.F.);
#16020=ORIENTED_EDGE('',*,*,#11145,.T.);
#16021=ORIENTED_EDGE('',*,*,#11143,.T.);
#16022=ORIENTED_EDGE('',*,*,#11146,.F.);
#16023=ORIENTED_EDGE('',*,*,#10786,.F.);
#16024=ORIENTED_EDGE('',*,*,#11147,.T.);
#16025=ORIENTED_EDGE('',*,*,#10996,.F.);
#16026=ORIENTED_EDGE('',*,*,#11148,.F.);
#16027=ORIENTED_EDGE('',*,*,#11149,.F.);
#16028=ORIENTED_EDGE('',*,*,#10785,.F.);
#16029=ORIENTED_EDGE('',*,*,#11150,.T.);
#16030=ORIENTED_EDGE('',*,*,#10997,.F.);
#16031=ORIENTED_EDGE('',*,*,#11147,.F.);
#16032=ORIENTED_EDGE('',*,*,#11142,.F.);
#16033=ORIENTED_EDGE('',*,*,#11144,.F.);
#16034=ORIENTED_EDGE('',*,*,#11145,.F.);
#16035=ORIENTED_EDGE('',*,*,#10998,.F.);
#16036=ORIENTED_EDGE('',*,*,#11150,.F.);
#16037=ORIENTED_EDGE('',*,*,#10784,.F.);
#16038=ORIENTED_EDGE('',*,*,#11146,.T.);
#16039=ORIENTED_EDGE('',*,*,#11151,.F.);
#16040=ORIENTED_EDGE('',*,*,#11152,.T.);
#16041=ORIENTED_EDGE('',*,*,#10787,.T.);
#16042=ORIENTED_EDGE('',*,*,#11149,.T.);
#16043=ORIENTED_EDGE('',*,*,#11153,.F.);
#16044=ORIENTED_EDGE('',*,*,#11154,.T.);
#16045=ORIENTED_EDGE('',*,*,#11151,.T.);
#16046=ORIENTED_EDGE('',*,*,#11148,.T.);
#16047=ORIENTED_EDGE('',*,*,#10995,.F.);
#16048=ORIENTED_EDGE('',*,*,#11155,.T.);
#16049=ORIENTED_EDGE('',*,*,#11153,.T.);
#16050=ORIENTED_EDGE('',*,*,#11156,.F.);
#16051=ORIENTED_EDGE('',*,*,#10790,.F.);
#16052=ORIENTED_EDGE('',*,*,#11157,.T.);
#16053=ORIENTED_EDGE('',*,*,#10992,.F.);
#16054=ORIENTED_EDGE('',*,*,#11158,.F.);
#16055=ORIENTED_EDGE('',*,*,#11159,.F.);
#16056=ORIENTED_EDGE('',*,*,#10789,.F.);
#16057=ORIENTED_EDGE('',*,*,#11160,.T.);
#16058=ORIENTED_EDGE('',*,*,#10993,.F.);
#16059=ORIENTED_EDGE('',*,*,#11157,.F.);
#16060=ORIENTED_EDGE('',*,*,#11152,.F.);
#16061=ORIENTED_EDGE('',*,*,#11154,.F.);
#16062=ORIENTED_EDGE('',*,*,#11155,.F.);
#16063=ORIENTED_EDGE('',*,*,#10994,.F.);
#16064=ORIENTED_EDGE('',*,*,#11160,.F.);
#16065=ORIENTED_EDGE('',*,*,#10788,.F.);
#16066=ORIENTED_EDGE('',*,*,#11156,.T.);
#16067=ORIENTED_EDGE('',*,*,#11161,.F.);
#16068=ORIENTED_EDGE('',*,*,#11162,.T.);
#16069=ORIENTED_EDGE('',*,*,#10791,.T.);
#16070=ORIENTED_EDGE('',*,*,#11159,.T.);
#16071=ORIENTED_EDGE('',*,*,#11163,.F.);
#16072=ORIENTED_EDGE('',*,*,#11164,.T.);
#16073=ORIENTED_EDGE('',*,*,#11161,.T.);
#16074=ORIENTED_EDGE('',*,*,#11158,.T.);
#16075=ORIENTED_EDGE('',*,*,#10991,.F.);
#16076=ORIENTED_EDGE('',*,*,#11165,.T.);
#16077=ORIENTED_EDGE('',*,*,#11163,.T.);
#16078=ORIENTED_EDGE('',*,*,#11166,.F.);
#16079=ORIENTED_EDGE('',*,*,#10794,.F.);
#16080=ORIENTED_EDGE('',*,*,#11167,.T.);
#16081=ORIENTED_EDGE('',*,*,#10988,.F.);
#16082=ORIENTED_EDGE('',*,*,#11168,.F.);
#16083=ORIENTED_EDGE('',*,*,#11169,.F.);
#16084=ORIENTED_EDGE('',*,*,#10793,.F.);
#16085=ORIENTED_EDGE('',*,*,#11170,.T.);
#16086=ORIENTED_EDGE('',*,*,#10989,.F.);
#16087=ORIENTED_EDGE('',*,*,#11167,.F.);
#16088=ORIENTED_EDGE('',*,*,#11162,.F.);
#16089=ORIENTED_EDGE('',*,*,#11164,.F.);
#16090=ORIENTED_EDGE('',*,*,#11165,.F.);
#16091=ORIENTED_EDGE('',*,*,#10990,.F.);
#16092=ORIENTED_EDGE('',*,*,#11170,.F.);
#16093=ORIENTED_EDGE('',*,*,#10792,.F.);
#16094=ORIENTED_EDGE('',*,*,#11166,.T.);
#16095=ORIENTED_EDGE('',*,*,#11171,.F.);
#16096=ORIENTED_EDGE('',*,*,#11172,.T.);
#16097=ORIENTED_EDGE('',*,*,#10795,.T.);
#16098=ORIENTED_EDGE('',*,*,#11169,.T.);
#16099=ORIENTED_EDGE('',*,*,#11173,.F.);
#16100=ORIENTED_EDGE('',*,*,#11174,.T.);
#16101=ORIENTED_EDGE('',*,*,#11171,.T.);
#16102=ORIENTED_EDGE('',*,*,#11168,.T.);
#16103=ORIENTED_EDGE('',*,*,#10987,.F.);
#16104=ORIENTED_EDGE('',*,*,#11175,.T.);
#16105=ORIENTED_EDGE('',*,*,#11173,.T.);
#16106=ORIENTED_EDGE('',*,*,#11176,.F.);
#16107=ORIENTED_EDGE('',*,*,#10798,.F.);
#16108=ORIENTED_EDGE('',*,*,#11177,.T.);
#16109=ORIENTED_EDGE('',*,*,#10984,.F.);
#16110=ORIENTED_EDGE('',*,*,#11178,.F.);
#16111=ORIENTED_EDGE('',*,*,#11179,.F.);
#16112=ORIENTED_EDGE('',*,*,#10797,.F.);
#16113=ORIENTED_EDGE('',*,*,#11180,.T.);
#16114=ORIENTED_EDGE('',*,*,#10985,.F.);
#16115=ORIENTED_EDGE('',*,*,#11177,.F.);
#16116=ORIENTED_EDGE('',*,*,#11172,.F.);
#16117=ORIENTED_EDGE('',*,*,#11174,.F.);
#16118=ORIENTED_EDGE('',*,*,#11175,.F.);
#16119=ORIENTED_EDGE('',*,*,#10986,.F.);
#16120=ORIENTED_EDGE('',*,*,#11180,.F.);
#16121=ORIENTED_EDGE('',*,*,#10796,.F.);
#16122=ORIENTED_EDGE('',*,*,#11176,.T.);
#16123=ORIENTED_EDGE('',*,*,#11181,.F.);
#16124=ORIENTED_EDGE('',*,*,#11182,.T.);
#16125=ORIENTED_EDGE('',*,*,#10799,.T.);
#16126=ORIENTED_EDGE('',*,*,#11179,.T.);
#16127=ORIENTED_EDGE('',*,*,#11183,.F.);
#16128=ORIENTED_EDGE('',*,*,#11184,.T.);
#16129=ORIENTED_EDGE('',*,*,#11181,.T.);
#16130=ORIENTED_EDGE('',*,*,#11178,.T.);
#16131=ORIENTED_EDGE('',*,*,#10983,.F.);
#16132=ORIENTED_EDGE('',*,*,#11185,.T.);
#16133=ORIENTED_EDGE('',*,*,#11183,.T.);
#16134=ORIENTED_EDGE('',*,*,#11186,.F.);
#16135=ORIENTED_EDGE('',*,*,#10802,.F.);
#16136=ORIENTED_EDGE('',*,*,#11187,.T.);
#16137=ORIENTED_EDGE('',*,*,#10980,.F.);
#16138=ORIENTED_EDGE('',*,*,#11188,.F.);
#16139=ORIENTED_EDGE('',*,*,#11189,.F.);
#16140=ORIENTED_EDGE('',*,*,#10801,.F.);
#16141=ORIENTED_EDGE('',*,*,#11190,.T.);
#16142=ORIENTED_EDGE('',*,*,#10981,.F.);
#16143=ORIENTED_EDGE('',*,*,#11187,.F.);
#16144=ORIENTED_EDGE('',*,*,#11182,.F.);
#16145=ORIENTED_EDGE('',*,*,#11184,.F.);
#16146=ORIENTED_EDGE('',*,*,#11185,.F.);
#16147=ORIENTED_EDGE('',*,*,#10982,.F.);
#16148=ORIENTED_EDGE('',*,*,#11190,.F.);
#16149=ORIENTED_EDGE('',*,*,#10800,.F.);
#16150=ORIENTED_EDGE('',*,*,#11186,.T.);
#16151=ORIENTED_EDGE('',*,*,#11191,.F.);
#16152=ORIENTED_EDGE('',*,*,#11192,.T.);
#16153=ORIENTED_EDGE('',*,*,#10803,.T.);
#16154=ORIENTED_EDGE('',*,*,#11189,.T.);
#16155=ORIENTED_EDGE('',*,*,#11193,.F.);
#16156=ORIENTED_EDGE('',*,*,#11194,.T.);
#16157=ORIENTED_EDGE('',*,*,#11191,.T.);
#16158=ORIENTED_EDGE('',*,*,#11188,.T.);
#16159=ORIENTED_EDGE('',*,*,#10979,.F.);
#16160=ORIENTED_EDGE('',*,*,#11195,.T.);
#16161=ORIENTED_EDGE('',*,*,#11193,.T.);
#16162=ORIENTED_EDGE('',*,*,#11196,.F.);
#16163=ORIENTED_EDGE('',*,*,#10806,.F.);
#16164=ORIENTED_EDGE('',*,*,#11197,.T.);
#16165=ORIENTED_EDGE('',*,*,#10976,.F.);
#16166=ORIENTED_EDGE('',*,*,#11198,.F.);
#16167=ORIENTED_EDGE('',*,*,#11199,.F.);
#16168=ORIENTED_EDGE('',*,*,#10805,.F.);
#16169=ORIENTED_EDGE('',*,*,#11200,.T.);
#16170=ORIENTED_EDGE('',*,*,#10977,.F.);
#16171=ORIENTED_EDGE('',*,*,#11197,.F.);
#16172=ORIENTED_EDGE('',*,*,#11192,.F.);
#16173=ORIENTED_EDGE('',*,*,#11194,.F.);
#16174=ORIENTED_EDGE('',*,*,#11195,.F.);
#16175=ORIENTED_EDGE('',*,*,#10978,.F.);
#16176=ORIENTED_EDGE('',*,*,#11200,.F.);
#16177=ORIENTED_EDGE('',*,*,#10804,.F.);
#16178=ORIENTED_EDGE('',*,*,#11196,.T.);
#16179=ORIENTED_EDGE('',*,*,#11201,.F.);
#16180=ORIENTED_EDGE('',*,*,#11202,.T.);
#16181=ORIENTED_EDGE('',*,*,#10807,.T.);
#16182=ORIENTED_EDGE('',*,*,#11199,.T.);
#16183=ORIENTED_EDGE('',*,*,#11203,.F.);
#16184=ORIENTED_EDGE('',*,*,#11204,.T.);
#16185=ORIENTED_EDGE('',*,*,#11201,.T.);
#16186=ORIENTED_EDGE('',*,*,#11198,.T.);
#16187=ORIENTED_EDGE('',*,*,#10975,.F.);
#16188=ORIENTED_EDGE('',*,*,#11205,.T.);
#16189=ORIENTED_EDGE('',*,*,#11203,.T.);
#16190=ORIENTED_EDGE('',*,*,#11206,.F.);
#16191=ORIENTED_EDGE('',*,*,#10810,.F.);
#16192=ORIENTED_EDGE('',*,*,#11207,.T.);
#16193=ORIENTED_EDGE('',*,*,#10972,.F.);
#16194=ORIENTED_EDGE('',*,*,#11208,.F.);
#16195=ORIENTED_EDGE('',*,*,#11209,.F.);
#16196=ORIENTED_EDGE('',*,*,#10809,.F.);
#16197=ORIENTED_EDGE('',*,*,#11210,.T.);
#16198=ORIENTED_EDGE('',*,*,#10973,.F.);
#16199=ORIENTED_EDGE('',*,*,#11207,.F.);
#16200=ORIENTED_EDGE('',*,*,#11202,.F.);
#16201=ORIENTED_EDGE('',*,*,#11204,.F.);
#16202=ORIENTED_EDGE('',*,*,#11205,.F.);
#16203=ORIENTED_EDGE('',*,*,#10974,.F.);
#16204=ORIENTED_EDGE('',*,*,#11210,.F.);
#16205=ORIENTED_EDGE('',*,*,#10808,.F.);
#16206=ORIENTED_EDGE('',*,*,#11206,.T.);
#16207=ORIENTED_EDGE('',*,*,#11211,.F.);
#16208=ORIENTED_EDGE('',*,*,#11212,.T.);
#16209=ORIENTED_EDGE('',*,*,#10811,.T.);
#16210=ORIENTED_EDGE('',*,*,#11209,.T.);
#16211=ORIENTED_EDGE('',*,*,#11213,.F.);
#16212=ORIENTED_EDGE('',*,*,#11214,.T.);
#16213=ORIENTED_EDGE('',*,*,#11211,.T.);
#16214=ORIENTED_EDGE('',*,*,#11208,.T.);
#16215=ORIENTED_EDGE('',*,*,#10971,.F.);
#16216=ORIENTED_EDGE('',*,*,#11215,.T.);
#16217=ORIENTED_EDGE('',*,*,#11213,.T.);
#16218=ORIENTED_EDGE('',*,*,#11216,.F.);
#16219=ORIENTED_EDGE('',*,*,#10814,.F.);
#16220=ORIENTED_EDGE('',*,*,#11217,.T.);
#16221=ORIENTED_EDGE('',*,*,#10968,.F.);
#16222=ORIENTED_EDGE('',*,*,#11218,.F.);
#16223=ORIENTED_EDGE('',*,*,#11219,.F.);
#16224=ORIENTED_EDGE('',*,*,#10813,.F.);
#16225=ORIENTED_EDGE('',*,*,#11220,.T.);
#16226=ORIENTED_EDGE('',*,*,#10969,.F.);
#16227=ORIENTED_EDGE('',*,*,#11217,.F.);
#16228=ORIENTED_EDGE('',*,*,#11212,.F.);
#16229=ORIENTED_EDGE('',*,*,#11214,.F.);
#16230=ORIENTED_EDGE('',*,*,#11215,.F.);
#16231=ORIENTED_EDGE('',*,*,#10970,.F.);
#16232=ORIENTED_EDGE('',*,*,#11220,.F.);
#16233=ORIENTED_EDGE('',*,*,#10812,.F.);
#16234=ORIENTED_EDGE('',*,*,#11216,.T.);
#16235=ORIENTED_EDGE('',*,*,#11221,.F.);
#16236=ORIENTED_EDGE('',*,*,#11222,.T.);
#16237=ORIENTED_EDGE('',*,*,#10815,.T.);
#16238=ORIENTED_EDGE('',*,*,#11219,.T.);
#16239=ORIENTED_EDGE('',*,*,#11223,.F.);
#16240=ORIENTED_EDGE('',*,*,#11224,.T.);
#16241=ORIENTED_EDGE('',*,*,#11221,.T.);
#16242=ORIENTED_EDGE('',*,*,#11218,.T.);
#16243=ORIENTED_EDGE('',*,*,#10967,.F.);
#16244=ORIENTED_EDGE('',*,*,#11225,.T.);
#16245=ORIENTED_EDGE('',*,*,#11223,.T.);
#16246=ORIENTED_EDGE('',*,*,#11226,.F.);
#16247=ORIENTED_EDGE('',*,*,#10818,.F.);
#16248=ORIENTED_EDGE('',*,*,#11227,.T.);
#16249=ORIENTED_EDGE('',*,*,#10964,.F.);
#16250=ORIENTED_EDGE('',*,*,#11228,.F.);
#16251=ORIENTED_EDGE('',*,*,#11229,.F.);
#16252=ORIENTED_EDGE('',*,*,#10817,.F.);
#16253=ORIENTED_EDGE('',*,*,#11230,.T.);
#16254=ORIENTED_EDGE('',*,*,#10965,.F.);
#16255=ORIENTED_EDGE('',*,*,#11227,.F.);
#16256=ORIENTED_EDGE('',*,*,#11222,.F.);
#16257=ORIENTED_EDGE('',*,*,#11224,.F.);
#16258=ORIENTED_EDGE('',*,*,#11225,.F.);
#16259=ORIENTED_EDGE('',*,*,#10966,.F.);
#16260=ORIENTED_EDGE('',*,*,#11230,.F.);
#16261=ORIENTED_EDGE('',*,*,#10816,.F.);
#16262=ORIENTED_EDGE('',*,*,#11226,.T.);
#16263=ORIENTED_EDGE('',*,*,#11231,.F.);
#16264=ORIENTED_EDGE('',*,*,#11232,.T.);
#16265=ORIENTED_EDGE('',*,*,#10819,.T.);
#16266=ORIENTED_EDGE('',*,*,#11229,.T.);
#16267=ORIENTED_EDGE('',*,*,#11233,.F.);
#16268=ORIENTED_EDGE('',*,*,#11234,.T.);
#16269=ORIENTED_EDGE('',*,*,#11231,.T.);
#16270=ORIENTED_EDGE('',*,*,#11228,.T.);
#16271=ORIENTED_EDGE('',*,*,#10963,.F.);
#16272=ORIENTED_EDGE('',*,*,#11235,.T.);
#16273=ORIENTED_EDGE('',*,*,#11233,.T.);
#16274=ORIENTED_EDGE('',*,*,#11236,.F.);
#16275=ORIENTED_EDGE('',*,*,#10822,.F.);
#16276=ORIENTED_EDGE('',*,*,#11237,.T.);
#16277=ORIENTED_EDGE('',*,*,#10960,.F.);
#16278=ORIENTED_EDGE('',*,*,#11238,.F.);
#16279=ORIENTED_EDGE('',*,*,#11239,.F.);
#16280=ORIENTED_EDGE('',*,*,#10821,.F.);
#16281=ORIENTED_EDGE('',*,*,#11240,.T.);
#16282=ORIENTED_EDGE('',*,*,#10961,.F.);
#16283=ORIENTED_EDGE('',*,*,#11237,.F.);
#16284=ORIENTED_EDGE('',*,*,#11232,.F.);
#16285=ORIENTED_EDGE('',*,*,#11234,.F.);
#16286=ORIENTED_EDGE('',*,*,#11235,.F.);
#16287=ORIENTED_EDGE('',*,*,#10962,.F.);
#16288=ORIENTED_EDGE('',*,*,#11240,.F.);
#16289=ORIENTED_EDGE('',*,*,#10820,.F.);
#16290=ORIENTED_EDGE('',*,*,#11236,.T.);
#16291=ORIENTED_EDGE('',*,*,#11241,.F.);
#16292=ORIENTED_EDGE('',*,*,#11242,.T.);
#16293=ORIENTED_EDGE('',*,*,#10823,.T.);
#16294=ORIENTED_EDGE('',*,*,#11239,.T.);
#16295=ORIENTED_EDGE('',*,*,#11243,.F.);
#16296=ORIENTED_EDGE('',*,*,#11244,.T.);
#16297=ORIENTED_EDGE('',*,*,#11241,.T.);
#16298=ORIENTED_EDGE('',*,*,#11238,.T.);
#16299=ORIENTED_EDGE('',*,*,#10959,.F.);
#16300=ORIENTED_EDGE('',*,*,#11245,.T.);
#16301=ORIENTED_EDGE('',*,*,#11243,.T.);
#16302=ORIENTED_EDGE('',*,*,#11246,.F.);
#16303=ORIENTED_EDGE('',*,*,#10826,.F.);
#16304=ORIENTED_EDGE('',*,*,#11247,.T.);
#16305=ORIENTED_EDGE('',*,*,#10956,.F.);
#16306=ORIENTED_EDGE('',*,*,#11248,.F.);
#16307=ORIENTED_EDGE('',*,*,#11249,.F.);
#16308=ORIENTED_EDGE('',*,*,#10825,.F.);
#16309=ORIENTED_EDGE('',*,*,#11250,.T.);
#16310=ORIENTED_EDGE('',*,*,#10957,.F.);
#16311=ORIENTED_EDGE('',*,*,#11247,.F.);
#16312=ORIENTED_EDGE('',*,*,#11242,.F.);
#16313=ORIENTED_EDGE('',*,*,#11244,.F.);
#16314=ORIENTED_EDGE('',*,*,#11245,.F.);
#16315=ORIENTED_EDGE('',*,*,#10958,.F.);
#16316=ORIENTED_EDGE('',*,*,#11250,.F.);
#16317=ORIENTED_EDGE('',*,*,#10824,.F.);
#16318=ORIENTED_EDGE('',*,*,#11246,.T.);
#16319=ORIENTED_EDGE('',*,*,#11251,.F.);
#16320=ORIENTED_EDGE('',*,*,#11252,.T.);
#16321=ORIENTED_EDGE('',*,*,#10827,.T.);
#16322=ORIENTED_EDGE('',*,*,#11249,.T.);
#16323=ORIENTED_EDGE('',*,*,#11253,.F.);
#16324=ORIENTED_EDGE('',*,*,#11254,.T.);
#16325=ORIENTED_EDGE('',*,*,#11251,.T.);
#16326=ORIENTED_EDGE('',*,*,#11248,.T.);
#16327=ORIENTED_EDGE('',*,*,#10955,.F.);
#16328=ORIENTED_EDGE('',*,*,#11255,.T.);
#16329=ORIENTED_EDGE('',*,*,#11253,.T.);
#16330=ORIENTED_EDGE('',*,*,#11256,.F.);
#16331=ORIENTED_EDGE('',*,*,#10830,.F.);
#16332=ORIENTED_EDGE('',*,*,#11257,.T.);
#16333=ORIENTED_EDGE('',*,*,#10952,.F.);
#16334=ORIENTED_EDGE('',*,*,#11258,.F.);
#16335=ORIENTED_EDGE('',*,*,#11259,.F.);
#16336=ORIENTED_EDGE('',*,*,#10829,.F.);
#16337=ORIENTED_EDGE('',*,*,#11260,.T.);
#16338=ORIENTED_EDGE('',*,*,#10953,.F.);
#16339=ORIENTED_EDGE('',*,*,#11257,.F.);
#16340=ORIENTED_EDGE('',*,*,#11252,.F.);
#16341=ORIENTED_EDGE('',*,*,#11254,.F.);
#16342=ORIENTED_EDGE('',*,*,#11255,.F.);
#16343=ORIENTED_EDGE('',*,*,#10954,.F.);
#16344=ORIENTED_EDGE('',*,*,#11260,.F.);
#16345=ORIENTED_EDGE('',*,*,#10828,.F.);
#16346=ORIENTED_EDGE('',*,*,#11256,.T.);
#16347=ORIENTED_EDGE('',*,*,#11261,.F.);
#16348=ORIENTED_EDGE('',*,*,#11262,.T.);
#16349=ORIENTED_EDGE('',*,*,#10831,.T.);
#16350=ORIENTED_EDGE('',*,*,#11259,.T.);
#16351=ORIENTED_EDGE('',*,*,#11263,.F.);
#16352=ORIENTED_EDGE('',*,*,#11264,.T.);
#16353=ORIENTED_EDGE('',*,*,#11261,.T.);
#16354=ORIENTED_EDGE('',*,*,#11258,.T.);
#16355=ORIENTED_EDGE('',*,*,#10951,.F.);
#16356=ORIENTED_EDGE('',*,*,#11265,.T.);
#16357=ORIENTED_EDGE('',*,*,#11263,.T.);
#16358=ORIENTED_EDGE('',*,*,#11266,.F.);
#16359=ORIENTED_EDGE('',*,*,#10834,.F.);
#16360=ORIENTED_EDGE('',*,*,#11267,.T.);
#16361=ORIENTED_EDGE('',*,*,#10948,.F.);
#16362=ORIENTED_EDGE('',*,*,#11268,.F.);
#16363=ORIENTED_EDGE('',*,*,#11269,.F.);
#16364=ORIENTED_EDGE('',*,*,#10833,.F.);
#16365=ORIENTED_EDGE('',*,*,#11270,.T.);
#16366=ORIENTED_EDGE('',*,*,#10949,.F.);
#16367=ORIENTED_EDGE('',*,*,#11267,.F.);
#16368=ORIENTED_EDGE('',*,*,#11262,.F.);
#16369=ORIENTED_EDGE('',*,*,#11264,.F.);
#16370=ORIENTED_EDGE('',*,*,#11265,.F.);
#16371=ORIENTED_EDGE('',*,*,#10950,.F.);
#16372=ORIENTED_EDGE('',*,*,#11270,.F.);
#16373=ORIENTED_EDGE('',*,*,#10832,.F.);
#16374=ORIENTED_EDGE('',*,*,#11266,.T.);
#16375=ORIENTED_EDGE('',*,*,#11271,.F.);
#16376=ORIENTED_EDGE('',*,*,#11272,.T.);
#16377=ORIENTED_EDGE('',*,*,#10835,.T.);
#16378=ORIENTED_EDGE('',*,*,#11269,.T.);
#16379=ORIENTED_EDGE('',*,*,#11273,.F.);
#16380=ORIENTED_EDGE('',*,*,#11274,.T.);
#16381=ORIENTED_EDGE('',*,*,#11271,.T.);
#16382=ORIENTED_EDGE('',*,*,#11268,.T.);
#16383=ORIENTED_EDGE('',*,*,#10947,.F.);
#16384=ORIENTED_EDGE('',*,*,#11275,.T.);
#16385=ORIENTED_EDGE('',*,*,#11273,.T.);
#16386=ORIENTED_EDGE('',*,*,#11276,.F.);
#16387=ORIENTED_EDGE('',*,*,#10838,.F.);
#16388=ORIENTED_EDGE('',*,*,#11277,.T.);
#16389=ORIENTED_EDGE('',*,*,#10944,.F.);
#16390=ORIENTED_EDGE('',*,*,#11278,.F.);
#16391=ORIENTED_EDGE('',*,*,#11279,.F.);
#16392=ORIENTED_EDGE('',*,*,#10837,.F.);
#16393=ORIENTED_EDGE('',*,*,#11280,.T.);
#16394=ORIENTED_EDGE('',*,*,#10945,.F.);
#16395=ORIENTED_EDGE('',*,*,#11277,.F.);
#16396=ORIENTED_EDGE('',*,*,#11272,.F.);
#16397=ORIENTED_EDGE('',*,*,#11274,.F.);
#16398=ORIENTED_EDGE('',*,*,#11275,.F.);
#16399=ORIENTED_EDGE('',*,*,#10946,.F.);
#16400=ORIENTED_EDGE('',*,*,#11280,.F.);
#16401=ORIENTED_EDGE('',*,*,#10836,.F.);
#16402=ORIENTED_EDGE('',*,*,#11276,.T.);
#16403=ORIENTED_EDGE('',*,*,#11281,.F.);
#16404=ORIENTED_EDGE('',*,*,#11282,.T.);
#16405=ORIENTED_EDGE('',*,*,#10839,.T.);
#16406=ORIENTED_EDGE('',*,*,#11279,.T.);
#16407=ORIENTED_EDGE('',*,*,#11283,.F.);
#16408=ORIENTED_EDGE('',*,*,#11284,.T.);
#16409=ORIENTED_EDGE('',*,*,#11281,.T.);
#16410=ORIENTED_EDGE('',*,*,#11278,.T.);
#16411=ORIENTED_EDGE('',*,*,#10943,.F.);
#16412=ORIENTED_EDGE('',*,*,#11285,.T.);
#16413=ORIENTED_EDGE('',*,*,#11283,.T.);
#16414=ORIENTED_EDGE('',*,*,#11286,.F.);
#16415=ORIENTED_EDGE('',*,*,#10842,.F.);
#16416=ORIENTED_EDGE('',*,*,#11287,.T.);
#16417=ORIENTED_EDGE('',*,*,#10940,.F.);
#16418=ORIENTED_EDGE('',*,*,#11288,.F.);
#16419=ORIENTED_EDGE('',*,*,#11289,.F.);
#16420=ORIENTED_EDGE('',*,*,#10841,.F.);
#16421=ORIENTED_EDGE('',*,*,#11290,.T.);
#16422=ORIENTED_EDGE('',*,*,#10941,.F.);
#16423=ORIENTED_EDGE('',*,*,#11287,.F.);
#16424=ORIENTED_EDGE('',*,*,#11282,.F.);
#16425=ORIENTED_EDGE('',*,*,#11284,.F.);
#16426=ORIENTED_EDGE('',*,*,#11285,.F.);
#16427=ORIENTED_EDGE('',*,*,#10942,.F.);
#16428=ORIENTED_EDGE('',*,*,#11290,.F.);
#16429=ORIENTED_EDGE('',*,*,#10840,.F.);
#16430=ORIENTED_EDGE('',*,*,#11286,.T.);
#16431=ORIENTED_EDGE('',*,*,#11291,.F.);
#16432=ORIENTED_EDGE('',*,*,#11292,.T.);
#16433=ORIENTED_EDGE('',*,*,#10843,.T.);
#16434=ORIENTED_EDGE('',*,*,#11289,.T.);
#16435=ORIENTED_EDGE('',*,*,#11293,.F.);
#16436=ORIENTED_EDGE('',*,*,#11294,.T.);
#16437=ORIENTED_EDGE('',*,*,#11291,.T.);
#16438=ORIENTED_EDGE('',*,*,#11288,.T.);
#16439=ORIENTED_EDGE('',*,*,#10939,.F.);
#16440=ORIENTED_EDGE('',*,*,#11295,.T.);
#16441=ORIENTED_EDGE('',*,*,#11293,.T.);
#16442=ORIENTED_EDGE('',*,*,#11296,.F.);
#16443=ORIENTED_EDGE('',*,*,#10846,.F.);
#16444=ORIENTED_EDGE('',*,*,#11297,.T.);
#16445=ORIENTED_EDGE('',*,*,#10936,.F.);
#16446=ORIENTED_EDGE('',*,*,#11298,.F.);
#16447=ORIENTED_EDGE('',*,*,#11299,.F.);
#16448=ORIENTED_EDGE('',*,*,#10845,.F.);
#16449=ORIENTED_EDGE('',*,*,#11300,.T.);
#16450=ORIENTED_EDGE('',*,*,#10937,.F.);
#16451=ORIENTED_EDGE('',*,*,#11297,.F.);
#16452=ORIENTED_EDGE('',*,*,#11292,.F.);
#16453=ORIENTED_EDGE('',*,*,#11294,.F.);
#16454=ORIENTED_EDGE('',*,*,#11295,.F.);
#16455=ORIENTED_EDGE('',*,*,#10938,.F.);
#16456=ORIENTED_EDGE('',*,*,#11300,.F.);
#16457=ORIENTED_EDGE('',*,*,#10844,.F.);
#16458=ORIENTED_EDGE('',*,*,#11296,.T.);
#16459=ORIENTED_EDGE('',*,*,#11301,.F.);
#16460=ORIENTED_EDGE('',*,*,#11302,.T.);
#16461=ORIENTED_EDGE('',*,*,#10847,.T.);
#16462=ORIENTED_EDGE('',*,*,#11299,.T.);
#16463=ORIENTED_EDGE('',*,*,#11303,.F.);
#16464=ORIENTED_EDGE('',*,*,#11304,.T.);
#16465=ORIENTED_EDGE('',*,*,#11301,.T.);
#16466=ORIENTED_EDGE('',*,*,#11298,.T.);
#16467=ORIENTED_EDGE('',*,*,#10935,.F.);
#16468=ORIENTED_EDGE('',*,*,#11305,.T.);
#16469=ORIENTED_EDGE('',*,*,#11303,.T.);
#16470=ORIENTED_EDGE('',*,*,#11306,.F.);
#16471=ORIENTED_EDGE('',*,*,#10850,.F.);
#16472=ORIENTED_EDGE('',*,*,#11307,.T.);
#16473=ORIENTED_EDGE('',*,*,#10932,.F.);
#16474=ORIENTED_EDGE('',*,*,#11308,.F.);
#16475=ORIENTED_EDGE('',*,*,#11309,.F.);
#16476=ORIENTED_EDGE('',*,*,#10849,.F.);
#16477=ORIENTED_EDGE('',*,*,#11310,.T.);
#16478=ORIENTED_EDGE('',*,*,#10933,.F.);
#16479=ORIENTED_EDGE('',*,*,#11307,.F.);
#16480=ORIENTED_EDGE('',*,*,#11302,.F.);
#16481=ORIENTED_EDGE('',*,*,#11304,.F.);
#16482=ORIENTED_EDGE('',*,*,#11305,.F.);
#16483=ORIENTED_EDGE('',*,*,#10934,.F.);
#16484=ORIENTED_EDGE('',*,*,#11310,.F.);
#16485=ORIENTED_EDGE('',*,*,#10848,.F.);
#16486=ORIENTED_EDGE('',*,*,#11306,.T.);
#16487=ORIENTED_EDGE('',*,*,#11311,.F.);
#16488=ORIENTED_EDGE('',*,*,#11312,.T.);
#16489=ORIENTED_EDGE('',*,*,#10851,.T.);
#16490=ORIENTED_EDGE('',*,*,#11309,.T.);
#16491=ORIENTED_EDGE('',*,*,#11313,.F.);
#16492=ORIENTED_EDGE('',*,*,#11314,.T.);
#16493=ORIENTED_EDGE('',*,*,#11311,.T.);
#16494=ORIENTED_EDGE('',*,*,#11308,.T.);
#16495=ORIENTED_EDGE('',*,*,#10931,.F.);
#16496=ORIENTED_EDGE('',*,*,#11315,.T.);
#16497=ORIENTED_EDGE('',*,*,#11313,.T.);
#16498=ORIENTED_EDGE('',*,*,#11316,.F.);
#16499=ORIENTED_EDGE('',*,*,#10854,.F.);
#16500=ORIENTED_EDGE('',*,*,#11317,.T.);
#16501=ORIENTED_EDGE('',*,*,#10928,.F.);
#16502=ORIENTED_EDGE('',*,*,#11318,.F.);
#16503=ORIENTED_EDGE('',*,*,#11319,.F.);
#16504=ORIENTED_EDGE('',*,*,#10853,.F.);
#16505=ORIENTED_EDGE('',*,*,#11320,.T.);
#16506=ORIENTED_EDGE('',*,*,#10929,.F.);
#16507=ORIENTED_EDGE('',*,*,#11317,.F.);
#16508=ORIENTED_EDGE('',*,*,#11312,.F.);
#16509=ORIENTED_EDGE('',*,*,#11314,.F.);
#16510=ORIENTED_EDGE('',*,*,#11315,.F.);
#16511=ORIENTED_EDGE('',*,*,#10930,.F.);
#16512=ORIENTED_EDGE('',*,*,#11320,.F.);
#16513=ORIENTED_EDGE('',*,*,#10852,.F.);
#16514=ORIENTED_EDGE('',*,*,#11316,.T.);
#16515=ORIENTED_EDGE('',*,*,#11321,.F.);
#16516=ORIENTED_EDGE('',*,*,#11322,.T.);
#16517=ORIENTED_EDGE('',*,*,#10855,.T.);
#16518=ORIENTED_EDGE('',*,*,#11319,.T.);
#16519=ORIENTED_EDGE('',*,*,#11323,.F.);
#16520=ORIENTED_EDGE('',*,*,#11324,.T.);
#16521=ORIENTED_EDGE('',*,*,#11321,.T.);
#16522=ORIENTED_EDGE('',*,*,#11318,.T.);
#16523=ORIENTED_EDGE('',*,*,#10927,.F.);
#16524=ORIENTED_EDGE('',*,*,#11325,.T.);
#16525=ORIENTED_EDGE('',*,*,#11323,.T.);
#16526=ORIENTED_EDGE('',*,*,#11326,.F.);
#16527=ORIENTED_EDGE('',*,*,#10858,.F.);
#16528=ORIENTED_EDGE('',*,*,#11327,.T.);
#16529=ORIENTED_EDGE('',*,*,#10924,.F.);
#16530=ORIENTED_EDGE('',*,*,#11328,.F.);
#16531=ORIENTED_EDGE('',*,*,#11329,.F.);
#16532=ORIENTED_EDGE('',*,*,#10857,.F.);
#16533=ORIENTED_EDGE('',*,*,#11330,.T.);
#16534=ORIENTED_EDGE('',*,*,#10925,.F.);
#16535=ORIENTED_EDGE('',*,*,#11327,.F.);
#16536=ORIENTED_EDGE('',*,*,#11322,.F.);
#16537=ORIENTED_EDGE('',*,*,#11324,.F.);
#16538=ORIENTED_EDGE('',*,*,#11325,.F.);
#16539=ORIENTED_EDGE('',*,*,#10926,.F.);
#16540=ORIENTED_EDGE('',*,*,#11330,.F.);
#16541=ORIENTED_EDGE('',*,*,#10856,.F.);
#16542=ORIENTED_EDGE('',*,*,#11326,.T.);
#16543=ORIENTED_EDGE('',*,*,#11331,.F.);
#16544=ORIENTED_EDGE('',*,*,#11332,.T.);
#16545=ORIENTED_EDGE('',*,*,#10859,.T.);
#16546=ORIENTED_EDGE('',*,*,#11329,.T.);
#16547=ORIENTED_EDGE('',*,*,#11333,.F.);
#16548=ORIENTED_EDGE('',*,*,#11334,.T.);
#16549=ORIENTED_EDGE('',*,*,#11331,.T.);
#16550=ORIENTED_EDGE('',*,*,#11328,.T.);
#16551=ORIENTED_EDGE('',*,*,#10923,.F.);
#16552=ORIENTED_EDGE('',*,*,#11335,.T.);
#16553=ORIENTED_EDGE('',*,*,#11333,.T.);
#16554=ORIENTED_EDGE('',*,*,#11336,.F.);
#16555=ORIENTED_EDGE('',*,*,#10862,.F.);
#16556=ORIENTED_EDGE('',*,*,#11337,.T.);
#16557=ORIENTED_EDGE('',*,*,#10920,.F.);
#16558=ORIENTED_EDGE('',*,*,#11338,.F.);
#16559=ORIENTED_EDGE('',*,*,#11339,.F.);
#16560=ORIENTED_EDGE('',*,*,#10861,.F.);
#16561=ORIENTED_EDGE('',*,*,#11340,.T.);
#16562=ORIENTED_EDGE('',*,*,#10921,.F.);
#16563=ORIENTED_EDGE('',*,*,#11337,.F.);
#16564=ORIENTED_EDGE('',*,*,#11332,.F.);
#16565=ORIENTED_EDGE('',*,*,#11334,.F.);
#16566=ORIENTED_EDGE('',*,*,#11335,.F.);
#16567=ORIENTED_EDGE('',*,*,#10922,.F.);
#16568=ORIENTED_EDGE('',*,*,#11340,.F.);
#16569=ORIENTED_EDGE('',*,*,#10860,.F.);
#16570=ORIENTED_EDGE('',*,*,#11336,.T.);
#16571=ORIENTED_EDGE('',*,*,#11341,.F.);
#16572=ORIENTED_EDGE('',*,*,#11342,.T.);
#16573=ORIENTED_EDGE('',*,*,#10863,.T.);
#16574=ORIENTED_EDGE('',*,*,#11339,.T.);
#16575=ORIENTED_EDGE('',*,*,#11343,.F.);
#16576=ORIENTED_EDGE('',*,*,#11344,.T.);
#16577=ORIENTED_EDGE('',*,*,#11341,.T.);
#16578=ORIENTED_EDGE('',*,*,#11338,.T.);
#16579=ORIENTED_EDGE('',*,*,#10919,.F.);
#16580=ORIENTED_EDGE('',*,*,#11345,.T.);
#16581=ORIENTED_EDGE('',*,*,#11343,.T.);
#16582=ORIENTED_EDGE('',*,*,#11346,.F.);
#16583=ORIENTED_EDGE('',*,*,#10866,.F.);
#16584=ORIENTED_EDGE('',*,*,#11347,.T.);
#16585=ORIENTED_EDGE('',*,*,#10916,.F.);
#16586=ORIENTED_EDGE('',*,*,#11348,.F.);
#16587=ORIENTED_EDGE('',*,*,#11349,.F.);
#16588=ORIENTED_EDGE('',*,*,#10865,.F.);
#16589=ORIENTED_EDGE('',*,*,#11350,.T.);
#16590=ORIENTED_EDGE('',*,*,#10917,.F.);
#16591=ORIENTED_EDGE('',*,*,#11347,.F.);
#16592=ORIENTED_EDGE('',*,*,#11342,.F.);
#16593=ORIENTED_EDGE('',*,*,#11344,.F.);
#16594=ORIENTED_EDGE('',*,*,#11345,.F.);
#16595=ORIENTED_EDGE('',*,*,#10918,.F.);
#16596=ORIENTED_EDGE('',*,*,#11350,.F.);
#16597=ORIENTED_EDGE('',*,*,#10864,.F.);
#16598=ORIENTED_EDGE('',*,*,#11346,.T.);
#16599=ORIENTED_EDGE('',*,*,#11351,.F.);
#16600=ORIENTED_EDGE('',*,*,#11352,.T.);
#16601=ORIENTED_EDGE('',*,*,#10867,.T.);
#16602=ORIENTED_EDGE('',*,*,#11349,.T.);
#16603=ORIENTED_EDGE('',*,*,#11353,.F.);
#16604=ORIENTED_EDGE('',*,*,#11354,.T.);
#16605=ORIENTED_EDGE('',*,*,#11351,.T.);
#16606=ORIENTED_EDGE('',*,*,#11348,.T.);
#16607=ORIENTED_EDGE('',*,*,#10915,.F.);
#16608=ORIENTED_EDGE('',*,*,#11355,.T.);
#16609=ORIENTED_EDGE('',*,*,#11353,.T.);
#16610=ORIENTED_EDGE('',*,*,#11356,.F.);
#16611=ORIENTED_EDGE('',*,*,#10870,.F.);
#16612=ORIENTED_EDGE('',*,*,#11357,.T.);
#16613=ORIENTED_EDGE('',*,*,#10912,.F.);
#16614=ORIENTED_EDGE('',*,*,#11358,.F.);
#16615=ORIENTED_EDGE('',*,*,#11359,.F.);
#16616=ORIENTED_EDGE('',*,*,#10869,.F.);
#16617=ORIENTED_EDGE('',*,*,#11360,.T.);
#16618=ORIENTED_EDGE('',*,*,#10913,.F.);
#16619=ORIENTED_EDGE('',*,*,#11357,.F.);
#16620=ORIENTED_EDGE('',*,*,#11352,.F.);
#16621=ORIENTED_EDGE('',*,*,#11354,.F.);
#16622=ORIENTED_EDGE('',*,*,#11355,.F.);
#16623=ORIENTED_EDGE('',*,*,#10914,.F.);
#16624=ORIENTED_EDGE('',*,*,#11360,.F.);
#16625=ORIENTED_EDGE('',*,*,#10868,.F.);
#16626=ORIENTED_EDGE('',*,*,#11356,.T.);
#16627=ORIENTED_EDGE('',*,*,#11361,.F.);
#16628=ORIENTED_EDGE('',*,*,#11362,.T.);
#16629=ORIENTED_EDGE('',*,*,#10871,.T.);
#16630=ORIENTED_EDGE('',*,*,#11359,.T.);
#16631=ORIENTED_EDGE('',*,*,#11363,.F.);
#16632=ORIENTED_EDGE('',*,*,#11364,.T.);
#16633=ORIENTED_EDGE('',*,*,#11361,.T.);
#16634=ORIENTED_EDGE('',*,*,#11358,.T.);
#16635=ORIENTED_EDGE('',*,*,#10911,.F.);
#16636=ORIENTED_EDGE('',*,*,#11365,.T.);
#16637=ORIENTED_EDGE('',*,*,#11363,.T.);
#16638=ORIENTED_EDGE('',*,*,#11366,.F.);
#16639=ORIENTED_EDGE('',*,*,#10874,.F.);
#16640=ORIENTED_EDGE('',*,*,#11367,.T.);
#16641=ORIENTED_EDGE('',*,*,#10908,.F.);
#16642=ORIENTED_EDGE('',*,*,#11368,.F.);
#16643=ORIENTED_EDGE('',*,*,#11369,.F.);
#16644=ORIENTED_EDGE('',*,*,#10873,.F.);
#16645=ORIENTED_EDGE('',*,*,#11370,.T.);
#16646=ORIENTED_EDGE('',*,*,#10909,.F.);
#16647=ORIENTED_EDGE('',*,*,#11367,.F.);
#16648=ORIENTED_EDGE('',*,*,#11362,.F.);
#16649=ORIENTED_EDGE('',*,*,#11364,.F.);
#16650=ORIENTED_EDGE('',*,*,#11365,.F.);
#16651=ORIENTED_EDGE('',*,*,#10910,.F.);
#16652=ORIENTED_EDGE('',*,*,#11370,.F.);
#16653=ORIENTED_EDGE('',*,*,#10872,.F.);
#16654=ORIENTED_EDGE('',*,*,#11366,.T.);
#16655=ORIENTED_EDGE('',*,*,#11371,.F.);
#16656=ORIENTED_EDGE('',*,*,#11372,.T.);
#16657=ORIENTED_EDGE('',*,*,#10875,.T.);
#16658=ORIENTED_EDGE('',*,*,#11369,.T.);
#16659=ORIENTED_EDGE('',*,*,#11373,.F.);
#16660=ORIENTED_EDGE('',*,*,#11374,.T.);
#16661=ORIENTED_EDGE('',*,*,#11371,.T.);
#16662=ORIENTED_EDGE('',*,*,#11368,.T.);
#16663=ORIENTED_EDGE('',*,*,#10907,.F.);
#16664=ORIENTED_EDGE('',*,*,#11375,.T.);
#16665=ORIENTED_EDGE('',*,*,#11373,.T.);
#16666=ORIENTED_EDGE('',*,*,#11376,.F.);
#16667=ORIENTED_EDGE('',*,*,#10878,.F.);
#16668=ORIENTED_EDGE('',*,*,#11377,.T.);
#16669=ORIENTED_EDGE('',*,*,#10904,.F.);
#16670=ORIENTED_EDGE('',*,*,#11378,.F.);
#16671=ORIENTED_EDGE('',*,*,#11379,.F.);
#16672=ORIENTED_EDGE('',*,*,#10877,.F.);
#16673=ORIENTED_EDGE('',*,*,#11380,.T.);
#16674=ORIENTED_EDGE('',*,*,#10905,.F.);
#16675=ORIENTED_EDGE('',*,*,#11377,.F.);
#16676=ORIENTED_EDGE('',*,*,#11372,.F.);
#16677=ORIENTED_EDGE('',*,*,#11374,.F.);
#16678=ORIENTED_EDGE('',*,*,#11375,.F.);
#16679=ORIENTED_EDGE('',*,*,#10906,.F.);
#16680=ORIENTED_EDGE('',*,*,#11380,.F.);
#16681=ORIENTED_EDGE('',*,*,#10876,.F.);
#16682=ORIENTED_EDGE('',*,*,#11138,.T.);
#16683=ORIENTED_EDGE('',*,*,#10879,.T.);
#16684=ORIENTED_EDGE('',*,*,#11376,.T.);
#16685=ORIENTED_EDGE('',*,*,#11381,.F.);
#16686=ORIENTED_EDGE('',*,*,#11139,.T.);
#16687=ORIENTED_EDGE('',*,*,#11381,.T.);
#16688=ORIENTED_EDGE('',*,*,#11379,.T.);
#16689=ORIENTED_EDGE('',*,*,#11382,.F.);
#16690=ORIENTED_EDGE('',*,*,#11140,.T.);
#16691=ORIENTED_EDGE('',*,*,#11382,.T.);
#16692=ORIENTED_EDGE('',*,*,#11378,.T.);
#16693=ORIENTED_EDGE('',*,*,#10903,.F.);
#16694=ORIENTED_EDGE('',*,*,#11127,.T.);
#16695=ORIENTED_EDGE('',*,*,#11383,.F.);
#16696=ORIENTED_EDGE('',*,*,#11131,.T.);
#16697=ORIENTED_EDGE('',*,*,#11047,.T.);
#16698=ORIENTED_EDGE('',*,*,#11126,.T.);
#16699=ORIENTED_EDGE('',*,*,#10729,.F.);
#16700=ORIENTED_EDGE('',*,*,#11129,.T.);
#16701=ORIENTED_EDGE('',*,*,#11383,.T.);
#16702=ORIENTED_EDGE('',*,*,#11384,.T.);
#16703=ORIENTED_EDGE('',*,*,#11385,.T.);
#16704=ORIENTED_EDGE('',*,*,#11386,.T.);
#16705=ORIENTED_EDGE('',*,*,#11387,.T.);
#16706=ORIENTED_EDGE('',*,*,#11385,.F.);
#16707=ORIENTED_EDGE('',*,*,#11387,.F.);
#16708=ORIENTED_EDGE('',*,*,#11388,.T.);
#16709=ORIENTED_EDGE('',*,*,#11389,.F.);
#16710=ORIENTED_EDGE('',*,*,#11390,.F.);
#16711=ORIENTED_EDGE('',*,*,#11388,.F.);
#16712=ORIENTED_EDGE('',*,*,#11386,.F.);
#16713=ORIENTED_EDGE('',*,*,#11384,.F.);
#16714=ORIENTED_EDGE('',*,*,#11389,.T.);
#16715=ORIENTED_EDGE('',*,*,#11390,.T.);
#16716=ORIENTED_EDGE('',*,*,#11391,.T.);
#16717=ORIENTED_EDGE('',*,*,#11392,.T.);
#16718=ORIENTED_EDGE('',*,*,#11393,.T.);
#16719=ORIENTED_EDGE('',*,*,#11391,.F.);
#16720=ORIENTED_EDGE('',*,*,#11393,.F.);
#16721=ORIENTED_EDGE('',*,*,#11394,.T.);
#16722=ORIENTED_EDGE('',*,*,#11395,.F.);
#16723=ORIENTED_EDGE('',*,*,#11396,.F.);
#16724=ORIENTED_EDGE('',*,*,#11394,.F.);
#16725=ORIENTED_EDGE('',*,*,#11392,.F.);
#16726=ORIENTED_EDGE('',*,*,#11395,.T.);
#16727=ORIENTED_EDGE('',*,*,#11396,.T.);
#16728=ORIENTED_EDGE('',*,*,#11397,.T.);
#16729=ORIENTED_EDGE('',*,*,#11398,.T.);
#16730=ORIENTED_EDGE('',*,*,#11399,.T.);
#16731=ORIENTED_EDGE('',*,*,#11397,.F.);
#16732=ORIENTED_EDGE('',*,*,#11399,.F.);
#16733=ORIENTED_EDGE('',*,*,#11400,.T.);
#16734=ORIENTED_EDGE('',*,*,#11401,.F.);
#16735=ORIENTED_EDGE('',*,*,#11402,.F.);
#16736=ORIENTED_EDGE('',*,*,#11400,.F.);
#16737=ORIENTED_EDGE('',*,*,#11398,.F.);
#16738=ORIENTED_EDGE('',*,*,#11401,.T.);
#16739=ORIENTED_EDGE('',*,*,#11402,.T.);
#16740=ORIENTED_EDGE('',*,*,#11403,.T.);
#16741=ORIENTED_EDGE('',*,*,#11404,.T.);
#16742=ORIENTED_EDGE('',*,*,#11403,.F.);
#16743=ORIENTED_EDGE('',*,*,#11404,.F.);
#16744=ORIENTED_EDGE('',*,*,#11405,.T.);
#16745=ORIENTED_EDGE('',*,*,#11406,.T.);
#16746=ORIENTED_EDGE('',*,*,#11407,.T.);
#16747=ORIENTED_EDGE('',*,*,#11408,.T.);
#16748=ORIENTED_EDGE('',*,*,#11409,.T.);
#16749=ORIENTED_EDGE('',*,*,#11410,.T.);
#16750=ORIENTED_EDGE('',*,*,#11407,.F.);
#16751=ORIENTED_EDGE('',*,*,#11411,.T.);
#16752=ORIENTED_EDGE('',*,*,#11412,.T.);
#16753=ORIENTED_EDGE('',*,*,#11413,.T.);
#16754=ORIENTED_EDGE('',*,*,#11409,.F.);
#16755=ORIENTED_EDGE('',*,*,#11414,.T.);
#16756=ORIENTED_EDGE('',*,*,#11405,.F.);
#16757=ORIENTED_EDGE('',*,*,#11415,.T.);
#16758=ORIENTED_EDGE('',*,*,#11412,.F.);
#16759=ORIENTED_EDGE('',*,*,#11416,.T.);
#16760=ORIENTED_EDGE('',*,*,#11411,.F.);
#16761=ORIENTED_EDGE('',*,*,#11417,.F.);
#16762=ORIENTED_EDGE('',*,*,#11418,.F.);
#16763=ORIENTED_EDGE('',*,*,#11419,.T.);
#16764=ORIENTED_EDGE('',*,*,#11406,.F.);
#16765=ORIENTED_EDGE('',*,*,#11420,.F.);
#16766=ORIENTED_EDGE('',*,*,#11421,.F.);
#16767=ORIENTED_EDGE('',*,*,#11417,.T.);
#16768=ORIENTED_EDGE('',*,*,#11408,.F.);
#16769=ORIENTED_EDGE('',*,*,#11410,.F.);
#16770=ORIENTED_EDGE('',*,*,#11413,.F.);
#16771=ORIENTED_EDGE('',*,*,#11415,.F.);
#16772=ORIENTED_EDGE('',*,*,#11422,.F.);
#16773=ORIENTED_EDGE('',*,*,#11423,.T.);
#16774=ORIENTED_EDGE('',*,*,#11421,.T.);
#16775=ORIENTED_EDGE('',*,*,#11424,.T.);
#16776=ORIENTED_EDGE('',*,*,#11425,.T.);
#16777=ORIENTED_EDGE('',*,*,#11426,.T.);
#16778=ORIENTED_EDGE('',*,*,#11427,.T.);
#16779=ORIENTED_EDGE('',*,*,#11424,.F.);
#16780=ORIENTED_EDGE('',*,*,#11428,.T.);
#16781=ORIENTED_EDGE('',*,*,#11429,.T.);
#16782=ORIENTED_EDGE('',*,*,#11430,.T.);
#16783=ORIENTED_EDGE('',*,*,#11426,.F.);
#16784=ORIENTED_EDGE('',*,*,#11431,.T.);
#16785=ORIENTED_EDGE('',*,*,#11429,.F.);
#16786=ORIENTED_EDGE('',*,*,#11418,.T.);
#16787=ORIENTED_EDGE('',*,*,#11423,.F.);
#16788=ORIENTED_EDGE('',*,*,#11432,.T.);
#16789=ORIENTED_EDGE('',*,*,#11416,.F.);
#16790=ORIENTED_EDGE('',*,*,#11433,.F.);
#16791=ORIENTED_EDGE('',*,*,#11428,.F.);
#16792=ORIENTED_EDGE('',*,*,#11420,.T.);
#16793=ORIENTED_EDGE('',*,*,#11425,.F.);
#16794=ORIENTED_EDGE('',*,*,#11427,.F.);
#16795=ORIENTED_EDGE('',*,*,#11430,.F.);
#16796=ORIENTED_EDGE('',*,*,#11432,.F.);
#16797=ORIENTED_EDGE('',*,*,#11434,.F.);
#16798=ORIENTED_EDGE('',*,*,#11434,.T.);
#16799=ORIENTED_EDGE('',*,*,#11435,.T.);
#16800=ORIENTED_EDGE('',*,*,#11436,.T.);
#16801=ORIENTED_EDGE('',*,*,#11435,.F.);
#16802=ORIENTED_EDGE('',*,*,#11436,.F.);
#16803=ORIENTED_EDGE('',*,*,#11437,.T.);
#16804=ORIENTED_EDGE('',*,*,#11438,.F.);
#16805=ORIENTED_EDGE('',*,*,#11439,.F.);
#16806=ORIENTED_EDGE('',*,*,#11437,.F.);
#16807=ORIENTED_EDGE('',*,*,#11422,.T.);
#16808=ORIENTED_EDGE('',*,*,#11440,.T.);
#16809=ORIENTED_EDGE('',*,*,#11438,.T.);
#16810=ORIENTED_EDGE('',*,*,#11439,.T.);
#16811=ORIENTED_EDGE('',*,*,#11440,.F.);
#16812=ORIENTED_EDGE('',*,*,#11414,.F.);
#16813=ORIENTED_EDGE('',*,*,#11419,.F.);
#16814=ORIENTED_EDGE('',*,*,#11431,.F.);
#16815=ORIENTED_EDGE('',*,*,#11433,.T.);
#16816=ORIENTED_EDGE('',*,*,#11441,.T.);
#16817=ORIENTED_EDGE('',*,*,#11442,.T.);
#16818=ORIENTED_EDGE('',*,*,#11443,.T.);
#16819=ORIENTED_EDGE('',*,*,#11444,.T.);
#16820=ORIENTED_EDGE('',*,*,#11442,.F.);
#16821=ORIENTED_EDGE('',*,*,#11444,.F.);
#16822=ORIENTED_EDGE('',*,*,#11445,.T.);
#16823=ORIENTED_EDGE('',*,*,#11446,.F.);
#16824=ORIENTED_EDGE('',*,*,#11447,.F.);
#16825=ORIENTED_EDGE('',*,*,#11445,.F.);
#16826=ORIENTED_EDGE('',*,*,#11443,.F.);
#16827=ORIENTED_EDGE('',*,*,#11441,.F.);
#16828=ORIENTED_EDGE('',*,*,#11446,.T.);
#16829=ORIENTED_EDGE('',*,*,#11447,.T.);
#16830=ORIENTED_EDGE('',*,*,#11448,.T.);
#16831=ORIENTED_EDGE('',*,*,#11449,.T.);
#16832=ORIENTED_EDGE('',*,*,#11450,.T.);
#16833=ORIENTED_EDGE('',*,*,#11448,.F.);
#16834=ORIENTED_EDGE('',*,*,#11450,.F.);
#16835=ORIENTED_EDGE('',*,*,#11451,.T.);
#16836=ORIENTED_EDGE('',*,*,#11452,.F.);
#16837=ORIENTED_EDGE('',*,*,#11453,.F.);
#16838=ORIENTED_EDGE('',*,*,#11451,.F.);
#16839=ORIENTED_EDGE('',*,*,#11449,.F.);
#16840=ORIENTED_EDGE('',*,*,#11452,.T.);
#16841=ORIENTED_EDGE('',*,*,#11453,.T.);
#16842=ORIENTED_EDGE('',*,*,#11454,.T.);
#16843=ORIENTED_EDGE('',*,*,#11455,.T.);
#16844=ORIENTED_EDGE('',*,*,#11456,.T.);
#16845=ORIENTED_EDGE('',*,*,#11454,.F.);
#16846=ORIENTED_EDGE('',*,*,#11456,.F.);
#16847=ORIENTED_EDGE('',*,*,#11457,.T.);
#16848=ORIENTED_EDGE('',*,*,#11458,.F.);
#16849=ORIENTED_EDGE('',*,*,#11459,.F.);
#16850=ORIENTED_EDGE('',*,*,#11457,.F.);
#16851=ORIENTED_EDGE('',*,*,#11455,.F.);
#16852=ORIENTED_EDGE('',*,*,#11458,.T.);
#16853=ORIENTED_EDGE('',*,*,#11459,.T.);
#16854=ORIENTED_EDGE('',*,*,#11460,.T.);
#16855=ORIENTED_EDGE('',*,*,#11461,.T.);
#16856=ORIENTED_EDGE('',*,*,#11460,.F.);
#16857=ORIENTED_EDGE('',*,*,#11461,.F.);
#16858=ORIENTED_EDGE('',*,*,#11462,.F.);
#16859=ORIENTED_EDGE('',*,*,#11463,.T.);
#16860=ORIENTED_EDGE('',*,*,#11464,.T.);
#16861=ORIENTED_EDGE('',*,*,#11463,.F.);
#16862=ORIENTED_EDGE('',*,*,#11462,.T.);
#16863=ORIENTED_EDGE('',*,*,#11464,.F.);
#16864=ORIENTED_EDGE('',*,*,#11465,.F.);
#16865=ORIENTED_EDGE('',*,*,#11466,.T.);
#16866=ORIENTED_EDGE('',*,*,#11467,.T.);
#16867=ORIENTED_EDGE('',*,*,#11468,.T.);
#16868=ORIENTED_EDGE('',*,*,#11469,.T.);
#16869=ORIENTED_EDGE('',*,*,#11470,.F.);
#16870=ORIENTED_EDGE('',*,*,#11471,.T.);
#16871=ORIENTED_EDGE('',*,*,#11472,.T.);
#16872=ORIENTED_EDGE('',*,*,#11473,.T.);
#16873=ORIENTED_EDGE('',*,*,#11474,.T.);
#16874=ORIENTED_EDGE('',*,*,#11475,.F.);
#16875=ORIENTED_EDGE('',*,*,#11476,.F.);
#16876=ORIENTED_EDGE('',*,*,#11477,.F.);
#16877=ORIENTED_EDGE('',*,*,#11478,.T.);
#16878=ORIENTED_EDGE('',*,*,#11476,.T.);
#16879=ORIENTED_EDGE('',*,*,#11479,.T.);
#16880=ORIENTED_EDGE('',*,*,#11474,.F.);
#16881=ORIENTED_EDGE('',*,*,#11480,.T.);
#16882=ORIENTED_EDGE('',*,*,#11481,.T.);
#16883=ORIENTED_EDGE('',*,*,#11477,.T.);
#16884=ORIENTED_EDGE('',*,*,#11482,.T.);
#16885=ORIENTED_EDGE('',*,*,#11480,.F.);
#16886=ORIENTED_EDGE('',*,*,#11483,.T.);
#16887=ORIENTED_EDGE('',*,*,#11484,.T.);
#16888=ORIENTED_EDGE('',*,*,#11485,.T.);
#16889=ORIENTED_EDGE('',*,*,#11486,.T.);
#16890=ORIENTED_EDGE('',*,*,#11487,.T.);
#16891=ORIENTED_EDGE('',*,*,#11485,.F.);
#16892=ORIENTED_EDGE('',*,*,#11488,.T.);
#16893=ORIENTED_EDGE('',*,*,#11475,.T.);
#16894=ORIENTED_EDGE('',*,*,#11489,.T.);
#16895=ORIENTED_EDGE('',*,*,#11472,.F.);
#16896=ORIENTED_EDGE('',*,*,#11490,.T.);
#16897=ORIENTED_EDGE('',*,*,#11467,.F.);
#16898=ORIENTED_EDGE('',*,*,#11469,.F.);
#16899=ORIENTED_EDGE('',*,*,#11491,.T.);
#16900=ORIENTED_EDGE('',*,*,#11492,.T.);
#16901=ORIENTED_EDGE('',*,*,#11493,.T.);
#16902=ORIENTED_EDGE('',*,*,#11494,.T.);
#16903=ORIENTED_EDGE('',*,*,#11468,.F.);
#16904=ORIENTED_EDGE('',*,*,#11495,.F.);
#16905=ORIENTED_EDGE('',*,*,#11496,.F.);
#16906=ORIENTED_EDGE('',*,*,#11491,.F.);
#16907=ORIENTED_EDGE('',*,*,#11471,.F.);
#16908=ORIENTED_EDGE('',*,*,#11479,.F.);
#16909=ORIENTED_EDGE('',*,*,#11488,.F.);
#16910=ORIENTED_EDGE('',*,*,#11497,.F.);
#16911=ORIENTED_EDGE('',*,*,#11490,.F.);
#16912=ORIENTED_EDGE('',*,*,#11497,.T.);
#16913=ORIENTED_EDGE('',*,*,#11487,.F.);
#16914=ORIENTED_EDGE('',*,*,#11495,.T.);
#16915=ORIENTED_EDGE('',*,*,#11483,.F.);
#16916=ORIENTED_EDGE('',*,*,#11498,.T.);
#16917=ORIENTED_EDGE('',*,*,#11499,.T.);
#16918=ORIENTED_EDGE('',*,*,#11500,.T.);
#16919=ORIENTED_EDGE('',*,*,#11501,.F.);
#16920=ORIENTED_EDGE('',*,*,#11492,.F.);
#16921=ORIENTED_EDGE('',*,*,#11502,.F.);
#16922=ORIENTED_EDGE('',*,*,#11486,.F.);
#16923=ORIENTED_EDGE('',*,*,#11503,.T.);
#16924=ORIENTED_EDGE('',*,*,#11502,.T.);
#16925=ORIENTED_EDGE('',*,*,#11496,.T.);
#16926=ORIENTED_EDGE('',*,*,#11484,.F.);
#16927=ORIENTED_EDGE('',*,*,#11504,.T.);
#16928=ORIENTED_EDGE('',*,*,#11501,.T.);
#16929=ORIENTED_EDGE('',*,*,#11505,.T.);
#16930=ORIENTED_EDGE('',*,*,#11481,.F.);
#16931=ORIENTED_EDGE('',*,*,#11505,.F.);
#16932=ORIENTED_EDGE('',*,*,#11503,.F.);
#16933=ORIENTED_EDGE('',*,*,#11489,.F.);
#16934=ORIENTED_EDGE('',*,*,#11466,.F.);
#16935=ORIENTED_EDGE('',*,*,#11506,.T.);
#16936=ORIENTED_EDGE('',*,*,#11507,.T.);
#16937=ORIENTED_EDGE('',*,*,#11473,.F.);
#16938=ORIENTED_EDGE('',*,*,#11508,.F.);
#16939=ORIENTED_EDGE('',*,*,#11509,.T.);
#16940=ORIENTED_EDGE('',*,*,#11510,.T.);
#16941=ORIENTED_EDGE('',*,*,#11511,.T.);
#16942=ORIENTED_EDGE('',*,*,#11512,.T.);
#16943=ORIENTED_EDGE('',*,*,#11513,.F.);
#16944=ORIENTED_EDGE('',*,*,#11514,.T.);
#16945=ORIENTED_EDGE('',*,*,#11515,.T.);
#16946=ORIENTED_EDGE('',*,*,#11516,.T.);
#16947=ORIENTED_EDGE('',*,*,#11517,.T.);
#16948=ORIENTED_EDGE('',*,*,#11516,.F.);
#16949=ORIENTED_EDGE('',*,*,#11518,.T.);
#16950=ORIENTED_EDGE('',*,*,#11519,.T.);
#16951=ORIENTED_EDGE('',*,*,#11520,.T.);
#16952=ORIENTED_EDGE('',*,*,#11521,.T.);
#16953=ORIENTED_EDGE('',*,*,#11522,.T.);
#16954=ORIENTED_EDGE('',*,*,#11523,.T.);
#16955=ORIENTED_EDGE('',*,*,#11524,.T.);
#16956=ORIENTED_EDGE('',*,*,#11525,.T.);
#16957=ORIENTED_EDGE('',*,*,#11526,.T.);
#16958=ORIENTED_EDGE('',*,*,#11523,.F.);
#16959=ORIENTED_EDGE('',*,*,#11525,.F.);
#16960=ORIENTED_EDGE('',*,*,#11527,.T.);
#16961=ORIENTED_EDGE('',*,*,#11514,.F.);
#16962=ORIENTED_EDGE('',*,*,#11521,.F.);
#16963=ORIENTED_EDGE('',*,*,#11528,.T.);
#16964=ORIENTED_EDGE('',*,*,#11510,.F.);
#16965=ORIENTED_EDGE('',*,*,#11512,.F.);
#16966=ORIENTED_EDGE('',*,*,#11529,.T.);
#16967=ORIENTED_EDGE('',*,*,#11530,.T.);
#16968=ORIENTED_EDGE('',*,*,#11531,.T.);
#16969=ORIENTED_EDGE('',*,*,#11532,.T.);
#16970=ORIENTED_EDGE('',*,*,#11511,.F.);
#16971=ORIENTED_EDGE('',*,*,#11533,.F.);
#16972=ORIENTED_EDGE('',*,*,#11534,.F.);
#16973=ORIENTED_EDGE('',*,*,#11529,.F.);
#16974=ORIENTED_EDGE('',*,*,#11519,.F.);
#16975=ORIENTED_EDGE('',*,*,#11533,.T.);
#16976=ORIENTED_EDGE('',*,*,#11528,.F.);
#16977=ORIENTED_EDGE('',*,*,#11535,.T.);
#16978=ORIENTED_EDGE('',*,*,#11536,.F.);
#16979=ORIENTED_EDGE('',*,*,#11537,.F.);
#16980=ORIENTED_EDGE('',*,*,#11538,.F.);
#16981=ORIENTED_EDGE('',*,*,#11539,.T.);
#16982=ORIENTED_EDGE('',*,*,#11540,.T.);
#16983=ORIENTED_EDGE('',*,*,#11537,.T.);
#16984=ORIENTED_EDGE('',*,*,#11541,.T.);
#16985=ORIENTED_EDGE('',*,*,#11542,.F.);
#16986=ORIENTED_EDGE('',*,*,#11530,.F.);
#16987=ORIENTED_EDGE('',*,*,#11543,.F.);
#16988=ORIENTED_EDGE('',*,*,#11518,.F.);
#16989=ORIENTED_EDGE('',*,*,#11544,.T.);
#16990=ORIENTED_EDGE('',*,*,#11543,.T.);
#16991=ORIENTED_EDGE('',*,*,#11534,.T.);
#16992=ORIENTED_EDGE('',*,*,#11542,.T.);
#16993=ORIENTED_EDGE('',*,*,#11545,.T.);
#16994=ORIENTED_EDGE('',*,*,#11538,.T.);
#16995=ORIENTED_EDGE('',*,*,#11546,.T.);
#16996=ORIENTED_EDGE('',*,*,#11527,.F.);
#16997=ORIENTED_EDGE('',*,*,#11547,.T.);
#16998=ORIENTED_EDGE('',*,*,#11536,.T.);
#16999=ORIENTED_EDGE('',*,*,#11548,.T.);
#17000=ORIENTED_EDGE('',*,*,#11515,.F.);
#17001=ORIENTED_EDGE('',*,*,#11548,.F.);
#17002=ORIENTED_EDGE('',*,*,#11545,.F.);
#17003=ORIENTED_EDGE('',*,*,#11544,.F.);
#17004=ORIENTED_EDGE('',*,*,#11509,.F.);
#17005=ORIENTED_EDGE('',*,*,#11549,.T.);
#17006=ORIENTED_EDGE('',*,*,#11550,.T.);
#17007=ORIENTED_EDGE('',*,*,#11551,.T.);
#17008=ORIENTED_EDGE('',*,*,#11522,.F.);
#17009=ORIENTED_EDGE('',*,*,#11552,.T.);
#17010=ORIENTED_EDGE('',*,*,#11553,.T.);
#17011=ORIENTED_EDGE('',*,*,#11554,.T.);
#17012=ORIENTED_EDGE('',*,*,#11555,.T.);
#17013=ORIENTED_EDGE('',*,*,#11554,.F.);
#17014=ORIENTED_EDGE('',*,*,#11556,.T.);
#17015=ORIENTED_EDGE('',*,*,#11557,.T.);
#17016=ORIENTED_EDGE('',*,*,#11552,.F.);
#17017=ORIENTED_EDGE('',*,*,#11558,.T.);
#17018=ORIENTED_EDGE('',*,*,#11559,.T.);
#17019=ORIENTED_EDGE('',*,*,#11559,.F.);
#17020=ORIENTED_EDGE('',*,*,#11560,.T.);
#17021=ORIENTED_EDGE('',*,*,#11561,.F.);
#17022=ORIENTED_EDGE('',*,*,#11562,.T.);
#17023=ORIENTED_EDGE('',*,*,#11558,.F.);
#17024=ORIENTED_EDGE('',*,*,#11563,.T.);
#17025=ORIENTED_EDGE('',*,*,#11564,.T.);
#17026=ORIENTED_EDGE('',*,*,#11565,.T.);
#17027=ORIENTED_EDGE('',*,*,#11555,.F.);
#17028=ORIENTED_EDGE('',*,*,#11566,.F.);
#17029=ORIENTED_EDGE('',*,*,#11567,.F.);
#17030=ORIENTED_EDGE('',*,*,#11563,.F.);
#17031=ORIENTED_EDGE('',*,*,#11568,.F.);
#17032=ORIENTED_EDGE('',*,*,#11569,.T.);
#17033=ORIENTED_EDGE('',*,*,#11570,.T.);
#17034=ORIENTED_EDGE('',*,*,#11571,.T.);
#17035=ORIENTED_EDGE('',*,*,#11572,.T.);
#17036=ORIENTED_EDGE('',*,*,#11573,.F.);
#17037=ORIENTED_EDGE('',*,*,#11574,.T.);
#17038=ORIENTED_EDGE('',*,*,#11575,.T.);
#17039=ORIENTED_EDGE('',*,*,#11576,.T.);
#17040=ORIENTED_EDGE('',*,*,#11577,.T.);
#17041=ORIENTED_EDGE('',*,*,#11578,.T.);
#17042=ORIENTED_EDGE('',*,*,#11579,.T.);
#17043=ORIENTED_EDGE('',*,*,#11580,.T.);
#17044=ORIENTED_EDGE('',*,*,#11581,.T.);
#17045=ORIENTED_EDGE('',*,*,#11582,.T.);
#17046=ORIENTED_EDGE('',*,*,#11583,.T.);
#17047=ORIENTED_EDGE('',*,*,#11580,.F.);
#17048=ORIENTED_EDGE('',*,*,#11584,.T.);
#17049=ORIENTED_EDGE('',*,*,#11576,.F.);
#17050=ORIENTED_EDGE('',*,*,#11574,.F.);
#17051=ORIENTED_EDGE('',*,*,#11561,.T.);
#17052=ORIENTED_EDGE('',*,*,#11570,.F.);
#17053=ORIENTED_EDGE('',*,*,#11572,.F.);
#17054=ORIENTED_EDGE('',*,*,#11585,.T.);
#17055=ORIENTED_EDGE('',*,*,#11586,.F.);
#17056=ORIENTED_EDGE('',*,*,#11587,.T.);
#17057=ORIENTED_EDGE('',*,*,#11588,.T.);
#17058=ORIENTED_EDGE('',*,*,#11571,.F.);
#17059=ORIENTED_EDGE('',*,*,#11560,.F.);
#17060=ORIENTED_EDGE('',*,*,#11565,.F.);
#17061=ORIENTED_EDGE('',*,*,#11585,.F.);
#17062=ORIENTED_EDGE('',*,*,#11553,.F.);
#17063=ORIENTED_EDGE('',*,*,#11562,.F.);
#17064=ORIENTED_EDGE('',*,*,#11577,.F.);
#17065=ORIENTED_EDGE('',*,*,#11589,.F.);
#17066=ORIENTED_EDGE('',*,*,#11556,.F.);
#17067=ORIENTED_EDGE('',*,*,#11589,.T.);
#17068=ORIENTED_EDGE('',*,*,#11584,.F.);
#17069=ORIENTED_EDGE('',*,*,#11590,.T.);
#17070=ORIENTED_EDGE('',*,*,#11579,.F.);
#17071=ORIENTED_EDGE('',*,*,#11591,.F.);
#17072=ORIENTED_EDGE('',*,*,#11592,.F.);
#17073=ORIENTED_EDGE('',*,*,#11590,.F.);
#17074=ORIENTED_EDGE('',*,*,#11578,.F.);
#17075=ORIENTED_EDGE('',*,*,#11593,.T.);
#17076=ORIENTED_EDGE('',*,*,#11594,.T.);
#17077=ORIENTED_EDGE('',*,*,#11595,.T.);
#17078=ORIENTED_EDGE('',*,*,#11591,.T.);
#17079=ORIENTED_EDGE('',*,*,#11596,.F.);
#17080=ORIENTED_EDGE('',*,*,#11550,.F.);
#17081=ORIENTED_EDGE('',*,*,#11597,.T.);
#17082=ORIENTED_EDGE('',*,*,#11598,.T.);
#17083=ORIENTED_EDGE('',*,*,#11599,.T.);
#17084=ORIENTED_EDGE('',*,*,#11597,.F.);
#17085=ORIENTED_EDGE('',*,*,#11549,.F.);
#17086=ORIENTED_EDGE('',*,*,#11508,.T.);
#17087=ORIENTED_EDGE('',*,*,#11600,.F.);
#17088=ORIENTED_EDGE('',*,*,#11582,.F.);
#17089=ORIENTED_EDGE('',*,*,#11601,.T.);
#17090=ORIENTED_EDGE('',*,*,#11568,.T.);
#17091=ORIENTED_EDGE('',*,*,#11602,.F.);
#17092=ORIENTED_EDGE('',*,*,#11603,.T.);
#17093=ORIENTED_EDGE('',*,*,#11604,.T.);
#17094=ORIENTED_EDGE('',*,*,#11605,.F.);
#17095=ORIENTED_EDGE('',*,*,#11606,.T.);
#17096=ORIENTED_EDGE('',*,*,#11607,.F.);
#17097=ORIENTED_EDGE('',*,*,#11506,.F.);
#17098=ORIENTED_EDGE('',*,*,#11465,.T.);
#17099=ORIENTED_EDGE('',*,*,#11608,.F.);
#17100=ORIENTED_EDGE('',*,*,#11606,.F.);
#17101=ORIENTED_EDGE('',*,*,#11609,.T.);
#17102=ORIENTED_EDGE('',*,*,#11610,.F.);
#17103=ORIENTED_EDGE('',*,*,#11611,.T.);
#17104=ORIENTED_EDGE('',*,*,#11612,.F.);
#17105=ORIENTED_EDGE('',*,*,#11613,.F.);
#17106=ORIENTED_EDGE('',*,*,#11602,.T.);
#17107=ORIENTED_EDGE('',*,*,#11573,.T.);
#17108=ORIENTED_EDGE('',*,*,#11588,.F.);
#17109=ORIENTED_EDGE('',*,*,#11614,.T.);
#17110=ORIENTED_EDGE('',*,*,#11593,.F.);
#17111=ORIENTED_EDGE('',*,*,#11583,.F.);
#17112=ORIENTED_EDGE('',*,*,#11600,.T.);
#17113=ORIENTED_EDGE('',*,*,#11513,.T.);
#17114=ORIENTED_EDGE('',*,*,#11532,.F.);
#17115=ORIENTED_EDGE('',*,*,#11615,.T.);
#17116=ORIENTED_EDGE('',*,*,#11539,.F.);
#17117=ORIENTED_EDGE('',*,*,#11616,.T.);
#17118=ORIENTED_EDGE('',*,*,#11608,.T.);
#17119=ORIENTED_EDGE('',*,*,#11470,.T.);
#17120=ORIENTED_EDGE('',*,*,#11494,.F.);
#17121=ORIENTED_EDGE('',*,*,#11617,.T.);
#17122=ORIENTED_EDGE('',*,*,#11499,.F.);
#17123=ORIENTED_EDGE('',*,*,#11618,.T.);
#17124=ORIENTED_EDGE('',*,*,#11619,.F.);
#17125=ORIENTED_EDGE('',*,*,#11598,.F.);
#17126=ORIENTED_EDGE('',*,*,#11599,.F.);
#17127=ORIENTED_EDGE('',*,*,#11620,.T.);
#17128=ORIENTED_EDGE('',*,*,#11621,.F.);
#17129=ORIENTED_EDGE('',*,*,#11622,.F.);
#17130=ORIENTED_EDGE('',*,*,#11620,.F.);
#17131=ORIENTED_EDGE('',*,*,#11623,.T.);
#17132=ORIENTED_EDGE('',*,*,#11624,.T.);
#17133=ORIENTED_EDGE('',*,*,#11625,.T.);
#17134=ORIENTED_EDGE('',*,*,#11626,.T.);
#17135=ORIENTED_EDGE('',*,*,#11624,.F.);
#17136=ORIENTED_EDGE('',*,*,#11626,.F.);
#17137=ORIENTED_EDGE('',*,*,#11627,.T.);
#17138=ORIENTED_EDGE('',*,*,#11628,.F.);
#17139=ORIENTED_EDGE('',*,*,#11629,.F.);
#17140=ORIENTED_EDGE('',*,*,#11627,.F.);
#17141=ORIENTED_EDGE('',*,*,#11625,.F.);
#17142=ORIENTED_EDGE('',*,*,#11623,.F.);
#17143=ORIENTED_EDGE('',*,*,#11630,.F.);
#17144=ORIENTED_EDGE('',*,*,#11631,.F.);
#17145=ORIENTED_EDGE('',*,*,#11595,.F.);
#17146=ORIENTED_EDGE('',*,*,#11632,.F.);
#17147=ORIENTED_EDGE('',*,*,#11633,.T.);
#17148=ORIENTED_EDGE('',*,*,#11567,.T.);
#17149=ORIENTED_EDGE('',*,*,#11632,.T.);
#17150=ORIENTED_EDGE('',*,*,#11634,.T.);
#17151=ORIENTED_EDGE('',*,*,#11557,.F.);
#17152=ORIENTED_EDGE('',*,*,#11592,.T.);
#17153=ORIENTED_EDGE('',*,*,#11631,.T.);
#17154=ORIENTED_EDGE('',*,*,#11566,.T.);
#17155=ORIENTED_EDGE('',*,*,#11633,.F.);
#17156=ORIENTED_EDGE('',*,*,#11586,.T.);
#17157=ORIENTED_EDGE('',*,*,#11564,.F.);
#17158=ORIENTED_EDGE('',*,*,#11569,.F.);
#17159=ORIENTED_EDGE('',*,*,#11601,.F.);
#17160=ORIENTED_EDGE('',*,*,#11581,.F.);
#17161=ORIENTED_EDGE('',*,*,#11575,.F.);
#17162=ORIENTED_EDGE('',*,*,#11634,.F.);
#17163=ORIENTED_EDGE('',*,*,#11594,.F.);
#17164=ORIENTED_EDGE('',*,*,#11614,.F.);
#17165=ORIENTED_EDGE('',*,*,#11587,.F.);
#17166=ORIENTED_EDGE('',*,*,#11635,.T.);
#17167=ORIENTED_EDGE('',*,*,#11636,.T.);
#17168=ORIENTED_EDGE('',*,*,#11637,.T.);
#17169=ORIENTED_EDGE('',*,*,#11638,.T.);
#17170=ORIENTED_EDGE('',*,*,#11603,.F.);
#17171=ORIENTED_EDGE('',*,*,#11613,.T.);
#17172=ORIENTED_EDGE('',*,*,#11639,.T.);
#17173=ORIENTED_EDGE('',*,*,#11640,.T.);
#17174=ORIENTED_EDGE('',*,*,#11641,.T.);
#17175=ORIENTED_EDGE('',*,*,#11642,.T.);
#17176=ORIENTED_EDGE('',*,*,#11643,.T.);
#17177=ORIENTED_EDGE('',*,*,#11644,.T.);
#17178=ORIENTED_EDGE('',*,*,#11645,.T.);
#17179=ORIENTED_EDGE('',*,*,#11646,.T.);
#17180=ORIENTED_EDGE('',*,*,#11645,.F.);
#17181=ORIENTED_EDGE('',*,*,#11647,.T.);
#17182=ORIENTED_EDGE('',*,*,#11648,.T.);
#17183=ORIENTED_EDGE('',*,*,#11643,.F.);
#17184=ORIENTED_EDGE('',*,*,#11649,.T.);
#17185=ORIENTED_EDGE('',*,*,#11641,.F.);
#17186=ORIENTED_EDGE('',*,*,#11639,.F.);
#17187=ORIENTED_EDGE('',*,*,#11650,.T.);
#17188=ORIENTED_EDGE('',*,*,#11637,.F.);
#17189=ORIENTED_EDGE('',*,*,#11638,.F.);
#17190=ORIENTED_EDGE('',*,*,#11651,.F.);
#17191=ORIENTED_EDGE('',*,*,#11652,.F.);
#17192=ORIENTED_EDGE('',*,*,#11604,.F.);
#17193=ORIENTED_EDGE('',*,*,#11650,.F.);
#17194=ORIENTED_EDGE('',*,*,#11653,.T.);
#17195=ORIENTED_EDGE('',*,*,#11654,.T.);
#17196=ORIENTED_EDGE('',*,*,#11651,.T.);
#17197=ORIENTED_EDGE('',*,*,#11642,.F.);
#17198=ORIENTED_EDGE('',*,*,#11655,.F.);
#17199=ORIENTED_EDGE('',*,*,#11656,.F.);
#17200=ORIENTED_EDGE('',*,*,#11653,.F.);
#17201=ORIENTED_EDGE('',*,*,#11649,.F.);
#17202=ORIENTED_EDGE('',*,*,#11657,.T.);
#17203=ORIENTED_EDGE('',*,*,#11658,.F.);
#17204=ORIENTED_EDGE('',*,*,#11655,.T.);
#17205=ORIENTED_EDGE('',*,*,#11646,.F.);
#17206=ORIENTED_EDGE('',*,*,#11659,.F.);
#17207=ORIENTED_EDGE('',*,*,#11660,.F.);
#17208=ORIENTED_EDGE('',*,*,#11657,.F.);
#17209=ORIENTED_EDGE('',*,*,#11628,.T.);
#17210=ORIENTED_EDGE('',*,*,#11629,.T.);
#17211=ORIENTED_EDGE('',*,*,#11661,.T.);
#17212=ORIENTED_EDGE('',*,*,#11662,.T.);
#17213=ORIENTED_EDGE('',*,*,#11663,.T.);
#17214=ORIENTED_EDGE('',*,*,#11661,.F.);
#17215=ORIENTED_EDGE('',*,*,#11663,.F.);
#17216=ORIENTED_EDGE('',*,*,#11664,.T.);
#17217=ORIENTED_EDGE('',*,*,#11665,.F.);
#17218=ORIENTED_EDGE('',*,*,#11666,.F.);
#17219=ORIENTED_EDGE('',*,*,#11664,.F.);
#17220=ORIENTED_EDGE('',*,*,#11662,.F.);
#17221=ORIENTED_EDGE('',*,*,#11621,.T.);
#17222=ORIENTED_EDGE('',*,*,#11622,.T.);
#17223=ORIENTED_EDGE('',*,*,#11667,.T.);
#17224=ORIENTED_EDGE('',*,*,#11668,.T.);
#17225=ORIENTED_EDGE('',*,*,#11669,.T.);
#17226=ORIENTED_EDGE('',*,*,#11667,.F.);
#17227=ORIENTED_EDGE('',*,*,#11669,.F.);
#17228=ORIENTED_EDGE('',*,*,#11670,.T.);
#17229=ORIENTED_EDGE('',*,*,#11630,.T.);
#17230=ORIENTED_EDGE('',*,*,#11670,.F.);
#17231=ORIENTED_EDGE('',*,*,#11668,.F.);
#17232=ORIENTED_EDGE('',*,*,#11671,.F.);
#17233=ORIENTED_EDGE('',*,*,#11672,.T.);
#17234=ORIENTED_EDGE('',*,*,#11619,.T.);
#17235=ORIENTED_EDGE('',*,*,#11672,.F.);
#17236=ORIENTED_EDGE('',*,*,#11665,.T.);
#17237=ORIENTED_EDGE('',*,*,#11666,.T.);
#17238=ORIENTED_EDGE('',*,*,#11673,.T.);
#17239=ORIENTED_EDGE('',*,*,#11674,.T.);
#17240=ORIENTED_EDGE('',*,*,#11673,.F.);
#17241=ORIENTED_EDGE('',*,*,#11674,.F.);
#17242=ORIENTED_EDGE('',*,*,#11675,.F.);
#17243=ORIENTED_EDGE('',*,*,#11652,.T.);
#17244=ORIENTED_EDGE('',*,*,#11676,.T.);
#17245=ORIENTED_EDGE('',*,*,#11677,.T.);
#17246=ORIENTED_EDGE('',*,*,#11678,.T.);
#17247=ORIENTED_EDGE('',*,*,#11609,.F.);
#17248=ORIENTED_EDGE('',*,*,#11605,.T.);
#17249=ORIENTED_EDGE('',*,*,#11654,.F.);
#17250=ORIENTED_EDGE('',*,*,#11679,.T.);
#17251=ORIENTED_EDGE('',*,*,#11676,.F.);
#17252=ORIENTED_EDGE('',*,*,#11678,.F.);
#17253=ORIENTED_EDGE('',*,*,#11680,.T.);
#17254=ORIENTED_EDGE('',*,*,#11681,.T.);
#17255=ORIENTED_EDGE('',*,*,#11682,.T.);
#17256=ORIENTED_EDGE('',*,*,#11610,.T.);
#17257=ORIENTED_EDGE('',*,*,#11677,.F.);
#17258=ORIENTED_EDGE('',*,*,#11683,.F.);
#17259=ORIENTED_EDGE('',*,*,#11684,.F.);
#17260=ORIENTED_EDGE('',*,*,#11680,.F.);
#17261=ORIENTED_EDGE('',*,*,#11679,.F.);
#17262=ORIENTED_EDGE('',*,*,#11656,.T.);
#17263=ORIENTED_EDGE('',*,*,#11685,.F.);
#17264=ORIENTED_EDGE('',*,*,#11683,.T.);
#17265=ORIENTED_EDGE('',*,*,#11636,.F.);
#17266=ORIENTED_EDGE('',*,*,#11686,.F.);
#17267=ORIENTED_EDGE('',*,*,#11644,.F.);
#17268=ORIENTED_EDGE('',*,*,#11640,.F.);
#17269=ORIENTED_EDGE('',*,*,#11658,.T.);
#17270=ORIENTED_EDGE('',*,*,#11687,.T.);
#17271=ORIENTED_EDGE('',*,*,#11685,.T.);
#17272=ORIENTED_EDGE('',*,*,#11635,.F.);
#17273=ORIENTED_EDGE('',*,*,#11612,.T.);
#17274=ORIENTED_EDGE('',*,*,#11688,.T.);
#17275=ORIENTED_EDGE('',*,*,#11647,.F.);
#17276=ORIENTED_EDGE('',*,*,#11686,.T.);
#17277=ORIENTED_EDGE('',*,*,#11689,.F.);
#17278=ORIENTED_EDGE('',*,*,#11681,.F.);
#17279=ORIENTED_EDGE('',*,*,#11690,.F.);
#17280=ORIENTED_EDGE('',*,*,#11687,.F.);
#17281=ORIENTED_EDGE('',*,*,#11660,.T.);
#17282=ORIENTED_EDGE('',*,*,#11690,.T.);
#17283=ORIENTED_EDGE('',*,*,#11684,.T.);
#17284=ORIENTED_EDGE('',*,*,#11648,.F.);
#17285=ORIENTED_EDGE('',*,*,#11691,.T.);
#17286=ORIENTED_EDGE('',*,*,#11689,.T.);
#17287=ORIENTED_EDGE('',*,*,#11659,.T.);
#17288=ORIENTED_EDGE('',*,*,#11675,.T.);
#17289=ORIENTED_EDGE('',*,*,#11692,.T.);
#17290=ORIENTED_EDGE('',*,*,#11693,.T.);
#17291=ORIENTED_EDGE('',*,*,#11694,.T.);
#17292=ORIENTED_EDGE('',*,*,#11692,.F.);
#17293=ORIENTED_EDGE('',*,*,#11695,.F.);
#17294=ORIENTED_EDGE('',*,*,#11696,.T.);
#17295=ORIENTED_EDGE('',*,*,#11693,.F.);
#17296=ORIENTED_EDGE('',*,*,#11694,.F.);
#17297=ORIENTED_EDGE('',*,*,#11696,.F.);
#17298=ORIENTED_EDGE('',*,*,#11697,.F.);
#17299=ORIENTED_EDGE('',*,*,#11695,.T.);
#17300=ORIENTED_EDGE('',*,*,#11698,.T.);
#17301=ORIENTED_EDGE('',*,*,#11699,.T.);
#17302=ORIENTED_EDGE('',*,*,#11698,.F.);
#17303=ORIENTED_EDGE('',*,*,#11697,.T.);
#17304=ORIENTED_EDGE('',*,*,#11700,.T.);
#17305=ORIENTED_EDGE('',*,*,#11699,.F.);
#17306=ORIENTED_EDGE('',*,*,#11700,.F.);
#17307=ORIENTED_EDGE('',*,*,#11701,.T.);
#17308=ORIENTED_EDGE('',*,*,#11671,.T.);
#17309=ORIENTED_EDGE('',*,*,#11701,.F.);
#17310=ORIENTED_EDGE('',*,*,#11688,.F.);
#17311=ORIENTED_EDGE('',*,*,#11611,.F.);
#17312=ORIENTED_EDGE('',*,*,#11682,.F.);
#17313=ORIENTED_EDGE('',*,*,#11691,.F.);
#17314=ORIENTED_EDGE('',*,*,#11540,.F.);
#17315=ORIENTED_EDGE('',*,*,#11615,.F.);
#17316=ORIENTED_EDGE('',*,*,#11531,.F.);
#17317=ORIENTED_EDGE('',*,*,#11546,.F.);
#17318=ORIENTED_EDGE('',*,*,#11524,.F.);
#17319=ORIENTED_EDGE('',*,*,#11551,.F.);
#17320=ORIENTED_EDGE('',*,*,#11596,.T.);
#17321=ORIENTED_EDGE('',*,*,#11616,.F.);
#17322=ORIENTED_EDGE('',*,*,#11541,.F.);
#17323=ORIENTED_EDGE('',*,*,#11547,.F.);
#17324=ORIENTED_EDGE('',*,*,#11517,.F.);
#17325=ORIENTED_EDGE('',*,*,#11535,.F.);
#17326=ORIENTED_EDGE('',*,*,#11520,.F.);
#17327=ORIENTED_EDGE('',*,*,#11526,.F.);
#17328=ORIENTED_EDGE('',*,*,#11500,.F.);
#17329=ORIENTED_EDGE('',*,*,#11617,.F.);
#17330=ORIENTED_EDGE('',*,*,#11493,.F.);
#17331=ORIENTED_EDGE('',*,*,#11504,.F.);
#17332=ORIENTED_EDGE('',*,*,#11478,.F.);
#17333=ORIENTED_EDGE('',*,*,#11507,.F.);
#17334=ORIENTED_EDGE('',*,*,#11607,.T.);
#17335=ORIENTED_EDGE('',*,*,#11618,.F.);
#17336=ORIENTED_EDGE('',*,*,#11498,.F.);
#17337=ORIENTED_EDGE('',*,*,#11482,.F.);
#17338=ORIENTED_EDGE('',*,*,#11702,.F.);
#17339=ORIENTED_EDGE('',*,*,#11703,.F.);
#17340=ORIENTED_EDGE('',*,*,#11704,.F.);
#17341=ORIENTED_EDGE('',*,*,#11705,.F.);
#17342=ORIENTED_EDGE('',*,*,#11706,.F.);
#17343=ORIENTED_EDGE('',*,*,#11707,.F.);
#17344=ORIENTED_EDGE('',*,*,#11708,.F.);
#17345=ORIENTED_EDGE('',*,*,#11709,.F.);
#17346=ORIENTED_EDGE('',*,*,#11710,.F.);
#17347=ORIENTED_EDGE('',*,*,#11711,.F.);
#17348=ORIENTED_EDGE('',*,*,#11712,.F.);
#17349=ORIENTED_EDGE('',*,*,#11713,.F.);
#17350=ORIENTED_EDGE('',*,*,#11703,.T.);
#17351=ORIENTED_EDGE('',*,*,#11714,.T.);
#17352=ORIENTED_EDGE('',*,*,#11712,.T.);
#17353=ORIENTED_EDGE('',*,*,#11715,.T.);
#17354=ORIENTED_EDGE('',*,*,#11716,.F.);
#17355=ORIENTED_EDGE('',*,*,#11717,.F.);
#17356=ORIENTED_EDGE('',*,*,#11718,.F.);
#17357=ORIENTED_EDGE('',*,*,#11719,.F.);
#17358=ORIENTED_EDGE('',*,*,#11720,.F.);
#17359=ORIENTED_EDGE('',*,*,#11721,.F.);
#17360=ORIENTED_EDGE('',*,*,#11706,.T.);
#17361=ORIENTED_EDGE('',*,*,#11722,.T.);
#17362=ORIENTED_EDGE('',*,*,#11720,.T.);
#17363=ORIENTED_EDGE('',*,*,#11723,.T.);
#17364=ORIENTED_EDGE('',*,*,#11724,.F.);
#17365=ORIENTED_EDGE('',*,*,#11725,.F.);
#17366=ORIENTED_EDGE('',*,*,#11726,.F.);
#17367=ORIENTED_EDGE('',*,*,#11725,.T.);
#17368=ORIENTED_EDGE('',*,*,#11727,.T.);
#17369=ORIENTED_EDGE('',*,*,#11709,.T.);
#17370=ORIENTED_EDGE('',*,*,#11728,.T.);
#17371=ORIENTED_EDGE('',*,*,#11711,.T.);
#17372=ORIENTED_EDGE('',*,*,#11729,.T.);
#17373=ORIENTED_EDGE('',*,*,#11726,.T.);
#17374=ORIENTED_EDGE('',*,*,#11730,.T.);
#17375=ORIENTED_EDGE('',*,*,#11731,.F.);
#17376=ORIENTED_EDGE('',*,*,#11732,.F.);
#17377=ORIENTED_EDGE('',*,*,#11733,.F.);
#17378=ORIENTED_EDGE('',*,*,#11717,.T.);
#17379=ORIENTED_EDGE('',*,*,#11734,.T.);
#17380=ORIENTED_EDGE('',*,*,#11732,.T.);
#17381=ORIENTED_EDGE('',*,*,#11735,.T.);
#17382=ORIENTED_EDGE('',*,*,#11724,.T.);
#17383=ORIENTED_EDGE('',*,*,#11736,.T.);
#17384=ORIENTED_EDGE('',*,*,#11733,.T.);
#17385=ORIENTED_EDGE('',*,*,#11737,.T.);
#17386=ORIENTED_EDGE('',*,*,#11731,.T.);
#17387=ORIENTED_EDGE('',*,*,#11738,.T.);
#17388=ORIENTED_EDGE('',*,*,#11721,.T.);
#17389=ORIENTED_EDGE('',*,*,#11739,.T.);
#17390=ORIENTED_EDGE('',*,*,#11719,.T.);
#17391=ORIENTED_EDGE('',*,*,#11740,.T.);
#17392=ORIENTED_EDGE('',*,*,#11713,.T.);
#17393=ORIENTED_EDGE('',*,*,#11741,.T.);
#17394=ORIENTED_EDGE('',*,*,#11705,.T.);
#17395=ORIENTED_EDGE('',*,*,#11742,.T.);
#17396=ORIENTED_EDGE('',*,*,#11718,.T.);
#17397=ORIENTED_EDGE('',*,*,#11743,.T.);
#17398=ORIENTED_EDGE('',*,*,#11716,.T.);
#17399=ORIENTED_EDGE('',*,*,#11744,.T.);
#17400=ORIENTED_EDGE('',*,*,#11710,.T.);
#17401=ORIENTED_EDGE('',*,*,#11745,.T.);
#17402=ORIENTED_EDGE('',*,*,#11708,.T.);
#17403=ORIENTED_EDGE('',*,*,#11746,.T.);
#17404=ORIENTED_EDGE('',*,*,#11704,.T.);
#17405=ORIENTED_EDGE('',*,*,#11747,.T.);
#17406=ORIENTED_EDGE('',*,*,#11702,.T.);
#17407=ORIENTED_EDGE('',*,*,#11748,.T.);
#17408=ORIENTED_EDGE('',*,*,#11707,.T.);
#17409=ORIENTED_EDGE('',*,*,#11749,.T.);
#17410=ORIENTED_EDGE('',*,*,#11723,.F.);
#17411=ORIENTED_EDGE('',*,*,#11741,.F.);
#17412=ORIENTED_EDGE('',*,*,#11714,.F.);
#17413=ORIENTED_EDGE('',*,*,#11749,.F.);
#17414=ORIENTED_EDGE('',*,*,#11728,.F.);
#17415=ORIENTED_EDGE('',*,*,#11747,.F.);
#17416=ORIENTED_EDGE('',*,*,#11715,.F.);
#17417=ORIENTED_EDGE('',*,*,#11730,.F.);
#17418=ORIENTED_EDGE('',*,*,#11729,.F.);
#17419=ORIENTED_EDGE('',*,*,#11740,.F.);
#17420=ORIENTED_EDGE('',*,*,#11738,.F.);
#17421=ORIENTED_EDGE('',*,*,#11736,.F.);
#17422=ORIENTED_EDGE('',*,*,#11735,.F.);
#17423=ORIENTED_EDGE('',*,*,#11739,.F.);
#17424=ORIENTED_EDGE('',*,*,#11722,.F.);
#17425=ORIENTED_EDGE('',*,*,#11743,.F.);
#17426=ORIENTED_EDGE('',*,*,#11734,.F.);
#17427=ORIENTED_EDGE('',*,*,#11745,.F.);
#17428=ORIENTED_EDGE('',*,*,#11727,.F.);
#17429=ORIENTED_EDGE('',*,*,#11737,.F.);
#17430=ORIENTED_EDGE('',*,*,#11742,.F.);
#17431=ORIENTED_EDGE('',*,*,#11748,.F.);
#17432=ORIENTED_EDGE('',*,*,#11746,.F.);
#17433=ORIENTED_EDGE('',*,*,#11744,.F.);
#17434=ORIENTED_EDGE('',*,*,#11750,.T.);
#17435=ORIENTED_EDGE('',*,*,#11751,.T.);
#17436=ORIENTED_EDGE('',*,*,#11752,.F.);
#17437=ORIENTED_EDGE('',*,*,#11751,.F.);
#17438=ORIENTED_EDGE('',*,*,#11752,.T.);
#17439=ORIENTED_EDGE('',*,*,#11750,.F.);
#17440=ORIENTED_EDGE('',*,*,#11753,.T.);
#17441=ORIENTED_EDGE('',*,*,#11754,.T.);
#17442=ORIENTED_EDGE('',*,*,#11755,.T.);
#17443=ORIENTED_EDGE('',*,*,#11756,.T.);
#17444=ORIENTED_EDGE('',*,*,#11754,.F.);
#17445=ORIENTED_EDGE('',*,*,#11757,.F.);
#17446=ORIENTED_EDGE('',*,*,#11758,.F.);
#17447=ORIENTED_EDGE('',*,*,#11759,.T.);
#17448=ORIENTED_EDGE('',*,*,#11755,.F.);
#17449=ORIENTED_EDGE('',*,*,#11756,.F.);
#17450=ORIENTED_EDGE('',*,*,#11759,.F.);
#17451=ORIENTED_EDGE('',*,*,#11760,.T.);
#17452=ORIENTED_EDGE('',*,*,#11761,.F.);
#17453=ORIENTED_EDGE('',*,*,#11762,.F.);
#17454=ORIENTED_EDGE('',*,*,#11763,.F.);
#17455=ORIENTED_EDGE('',*,*,#11764,.T.);
#17456=ORIENTED_EDGE('',*,*,#11765,.F.);
#17457=ORIENTED_EDGE('',*,*,#11766,.T.);
#17458=ORIENTED_EDGE('',*,*,#11767,.F.);
#17459=ORIENTED_EDGE('',*,*,#11768,.F.);
#17460=ORIENTED_EDGE('',*,*,#11769,.F.);
#17461=ORIENTED_EDGE('',*,*,#11770,.F.);
#17462=ORIENTED_EDGE('',*,*,#11771,.T.);
#17463=ORIENTED_EDGE('',*,*,#11772,.F.);
#17464=ORIENTED_EDGE('',*,*,#11773,.T.);
#17465=ORIENTED_EDGE('',*,*,#11774,.F.);
#17466=ORIENTED_EDGE('',*,*,#11775,.F.);
#17467=ORIENTED_EDGE('',*,*,#11776,.F.);
#17468=ORIENTED_EDGE('',*,*,#11777,.T.);
#17469=ORIENTED_EDGE('',*,*,#11778,.F.);
#17470=ORIENTED_EDGE('',*,*,#11779,.T.);
#17471=ORIENTED_EDGE('',*,*,#11780,.F.);
#17472=ORIENTED_EDGE('',*,*,#11781,.F.);
#17473=ORIENTED_EDGE('',*,*,#11782,.F.);
#17474=ORIENTED_EDGE('',*,*,#11783,.T.);
#17475=ORIENTED_EDGE('',*,*,#11784,.F.);
#17476=ORIENTED_EDGE('',*,*,#11753,.F.);
#17477=ORIENTED_EDGE('',*,*,#11757,.T.);
#17478=ORIENTED_EDGE('',*,*,#11758,.T.);
#17479=ORIENTED_EDGE('',*,*,#11785,.T.);
#17480=ORIENTED_EDGE('',*,*,#11786,.T.);
#17481=ORIENTED_EDGE('',*,*,#11785,.F.);
#17482=ORIENTED_EDGE('',*,*,#11787,.T.);
#17483=ORIENTED_EDGE('',*,*,#11788,.T.);
#17484=ORIENTED_EDGE('',*,*,#11789,.T.);
#17485=ORIENTED_EDGE('',*,*,#11790,.F.);
#17486=ORIENTED_EDGE('',*,*,#11791,.T.);
#17487=ORIENTED_EDGE('',*,*,#11792,.T.);
#17488=ORIENTED_EDGE('',*,*,#11793,.T.);
#17489=ORIENTED_EDGE('',*,*,#11794,.F.);
#17490=ORIENTED_EDGE('',*,*,#11795,.T.);
#17491=ORIENTED_EDGE('',*,*,#11796,.T.);
#17492=ORIENTED_EDGE('',*,*,#11797,.F.);
#17493=ORIENTED_EDGE('',*,*,#11798,.T.);
#17494=ORIENTED_EDGE('',*,*,#11799,.F.);
#17495=ORIENTED_EDGE('',*,*,#11800,.T.);
#17496=ORIENTED_EDGE('',*,*,#11801,.F.);
#17497=ORIENTED_EDGE('',*,*,#11802,.T.);
#17498=ORIENTED_EDGE('',*,*,#11803,.T.);
#17499=ORIENTED_EDGE('',*,*,#11804,.F.);
#17500=ORIENTED_EDGE('',*,*,#11786,.F.);
#17501=ORIENTED_EDGE('',*,*,#11805,.T.);
#17502=ORIENTED_EDGE('',*,*,#11806,.T.);
#17503=ORIENTED_EDGE('',*,*,#11807,.T.);
#17504=ORIENTED_EDGE('',*,*,#11784,.T.);
#17505=ORIENTED_EDGE('',*,*,#11806,.F.);
#17506=ORIENTED_EDGE('',*,*,#11808,.T.);
#17507=ORIENTED_EDGE('',*,*,#11809,.F.);
#17508=ORIENTED_EDGE('',*,*,#11810,.F.);
#17509=ORIENTED_EDGE('',*,*,#11811,.T.);
#17510=ORIENTED_EDGE('',*,*,#11809,.T.);
#17511=ORIENTED_EDGE('',*,*,#11812,.T.);
#17512=ORIENTED_EDGE('',*,*,#11804,.T.);
#17513=ORIENTED_EDGE('',*,*,#11813,.T.);
#17514=ORIENTED_EDGE('',*,*,#11814,.T.);
#17515=ORIENTED_EDGE('',*,*,#11815,.T.);
#17516=ORIENTED_EDGE('',*,*,#11778,.T.);
#17517=ORIENTED_EDGE('',*,*,#11814,.F.);
#17518=ORIENTED_EDGE('',*,*,#11816,.T.);
#17519=ORIENTED_EDGE('',*,*,#11817,.F.);
#17520=ORIENTED_EDGE('',*,*,#11818,.F.);
#17521=ORIENTED_EDGE('',*,*,#11819,.T.);
#17522=ORIENTED_EDGE('',*,*,#11817,.T.);
#17523=ORIENTED_EDGE('',*,*,#11820,.T.);
#17524=ORIENTED_EDGE('',*,*,#11790,.T.);
#17525=ORIENTED_EDGE('',*,*,#11821,.T.);
#17526=ORIENTED_EDGE('',*,*,#11822,.T.);
#17527=ORIENTED_EDGE('',*,*,#11823,.T.);
#17528=ORIENTED_EDGE('',*,*,#11772,.T.);
#17529=ORIENTED_EDGE('',*,*,#11822,.F.);
#17530=ORIENTED_EDGE('',*,*,#11824,.T.);
#17531=ORIENTED_EDGE('',*,*,#11825,.F.);
#17532=ORIENTED_EDGE('',*,*,#11826,.F.);
#17533=ORIENTED_EDGE('',*,*,#11827,.T.);
#17534=ORIENTED_EDGE('',*,*,#11825,.T.);
#17535=ORIENTED_EDGE('',*,*,#11828,.T.);
#17536=ORIENTED_EDGE('',*,*,#11794,.T.);
#17537=ORIENTED_EDGE('',*,*,#11829,.T.);
#17538=ORIENTED_EDGE('',*,*,#11830,.T.);
#17539=ORIENTED_EDGE('',*,*,#11831,.T.);
#17540=ORIENTED_EDGE('',*,*,#11832,.T.);
#17541=ORIENTED_EDGE('',*,*,#11831,.F.);
#17542=ORIENTED_EDGE('',*,*,#11833,.T.);
#17543=ORIENTED_EDGE('',*,*,#11834,.T.);
#17544=ORIENTED_EDGE('',*,*,#11835,.T.);
#17545=ORIENTED_EDGE('',*,*,#11836,.T.);
#17546=ORIENTED_EDGE('',*,*,#11837,.T.);
#17547=ORIENTED_EDGE('',*,*,#11838,.T.);
#17548=ORIENTED_EDGE('',*,*,#11837,.F.);
#17549=ORIENTED_EDGE('',*,*,#11839,.T.);
#17550=ORIENTED_EDGE('',*,*,#11840,.T.);
#17551=ORIENTED_EDGE('',*,*,#11835,.F.);
#17552=ORIENTED_EDGE('',*,*,#11841,.T.);
#17553=ORIENTED_EDGE('',*,*,#11829,.F.);
#17554=ORIENTED_EDGE('',*,*,#11834,.F.);
#17555=ORIENTED_EDGE('',*,*,#11842,.T.);
#17556=ORIENTED_EDGE('',*,*,#11843,.T.);
#17557=ORIENTED_EDGE('',*,*,#11844,.T.);
#17558=ORIENTED_EDGE('',*,*,#11833,.F.);
#17559=ORIENTED_EDGE('',*,*,#11845,.T.);
#17560=ORIENTED_EDGE('',*,*,#11846,.F.);
#17561=ORIENTED_EDGE('',*,*,#11847,.T.);
#17562=ORIENTED_EDGE('',*,*,#11830,.F.);
#17563=ORIENTED_EDGE('',*,*,#11848,.F.);
#17564=ORIENTED_EDGE('',*,*,#11849,.F.);
#17565=ORIENTED_EDGE('',*,*,#11845,.F.);
#17566=ORIENTED_EDGE('',*,*,#11841,.F.);
#17567=ORIENTED_EDGE('',*,*,#11850,.T.);
#17568=ORIENTED_EDGE('',*,*,#11851,.T.);
#17569=ORIENTED_EDGE('',*,*,#11848,.T.);
#17570=ORIENTED_EDGE('',*,*,#11838,.F.);
#17571=ORIENTED_EDGE('',*,*,#11852,.F.);
#17572=ORIENTED_EDGE('',*,*,#11853,.F.);
#17573=ORIENTED_EDGE('',*,*,#11854,.T.);
#17574=ORIENTED_EDGE('',*,*,#11855,.F.);
#17575=ORIENTED_EDGE('',*,*,#11850,.F.);
#17576=ORIENTED_EDGE('',*,*,#11856,.F.);
#17577=ORIENTED_EDGE('',*,*,#11857,.T.);
#17578=ORIENTED_EDGE('',*,*,#11858,.T.);
#17579=ORIENTED_EDGE('',*,*,#11855,.T.);
#17580=ORIENTED_EDGE('',*,*,#11859,.F.);
#17581=ORIENTED_EDGE('',*,*,#11858,.F.);
#17582=ORIENTED_EDGE('',*,*,#11860,.T.);
#17583=ORIENTED_EDGE('',*,*,#11851,.F.);
#17584=ORIENTED_EDGE('',*,*,#11832,.F.);
#17585=ORIENTED_EDGE('',*,*,#11844,.F.);
#17586=ORIENTED_EDGE('',*,*,#11861,.F.);
#17587=ORIENTED_EDGE('',*,*,#11836,.F.);
#17588=ORIENTED_EDGE('',*,*,#11860,.F.);
#17589=ORIENTED_EDGE('',*,*,#11862,.T.);
#17590=ORIENTED_EDGE('',*,*,#11863,.F.);
#17591=ORIENTED_EDGE('',*,*,#11849,.T.);
#17592=ORIENTED_EDGE('',*,*,#11864,.F.);
#17593=ORIENTED_EDGE('',*,*,#11865,.T.);
#17594=ORIENTED_EDGE('',*,*,#11866,.T.);
#17595=ORIENTED_EDGE('',*,*,#11867,.F.);
#17596=ORIENTED_EDGE('',*,*,#11868,.T.);
#17597=ORIENTED_EDGE('',*,*,#11869,.F.);
#17598=ORIENTED_EDGE('',*,*,#11870,.F.);
#17599=ORIENTED_EDGE('',*,*,#11871,.F.);
#17600=ORIENTED_EDGE('',*,*,#11872,.F.);
#17601=ORIENTED_EDGE('',*,*,#11873,.F.);
#17602=ORIENTED_EDGE('',*,*,#11874,.T.);
#17603=ORIENTED_EDGE('',*,*,#11875,.F.);
#17604=ORIENTED_EDGE('',*,*,#11876,.F.);
#17605=ORIENTED_EDGE('',*,*,#11877,.F.);
#17606=ORIENTED_EDGE('',*,*,#11878,.F.);
#17607=ORIENTED_EDGE('',*,*,#11879,.F.);
#17608=ORIENTED_EDGE('',*,*,#11862,.F.);
#17609=ORIENTED_EDGE('',*,*,#11857,.F.);
#17610=ORIENTED_EDGE('',*,*,#11880,.T.);
#17611=ORIENTED_EDGE('',*,*,#11865,.F.);
#17612=ORIENTED_EDGE('',*,*,#11881,.F.);
#17613=ORIENTED_EDGE('',*,*,#11882,.T.);
#17614=ORIENTED_EDGE('',*,*,#11883,.T.);
#17615=ORIENTED_EDGE('',*,*,#11884,.T.);
#17616=ORIENTED_EDGE('',*,*,#11875,.T.);
#17617=ORIENTED_EDGE('',*,*,#11885,.T.);
#17618=ORIENTED_EDGE('',*,*,#11886,.T.);
#17619=ORIENTED_EDGE('',*,*,#11887,.T.);
#17620=ORIENTED_EDGE('',*,*,#11884,.F.);
#17621=ORIENTED_EDGE('',*,*,#11888,.T.);
#17622=ORIENTED_EDGE('',*,*,#11889,.T.);
#17623=ORIENTED_EDGE('',*,*,#11890,.T.);
#17624=ORIENTED_EDGE('',*,*,#11888,.F.);
#17625=ORIENTED_EDGE('',*,*,#11891,.T.);
#17626=ORIENTED_EDGE('',*,*,#11886,.F.);
#17627=ORIENTED_EDGE('',*,*,#11892,.T.);
#17628=ORIENTED_EDGE('',*,*,#11887,.F.);
#17629=ORIENTED_EDGE('',*,*,#11893,.T.);
#17630=ORIENTED_EDGE('',*,*,#11894,.F.);
#17631=ORIENTED_EDGE('',*,*,#11876,.T.);
#17632=ORIENTED_EDGE('',*,*,#11891,.F.);
#17633=ORIENTED_EDGE('',*,*,#11895,.F.);
#17634=ORIENTED_EDGE('',*,*,#11896,.F.);
#17635=ORIENTED_EDGE('',*,*,#11893,.F.);
#17636=ORIENTED_EDGE('',*,*,#11890,.F.);
#17637=ORIENTED_EDGE('',*,*,#11897,.T.);
#17638=ORIENTED_EDGE('',*,*,#11898,.T.);
#17639=ORIENTED_EDGE('',*,*,#11895,.T.);
#17640=ORIENTED_EDGE('',*,*,#11899,.T.);
#17641=ORIENTED_EDGE('',*,*,#11900,.T.);
#17642=ORIENTED_EDGE('',*,*,#11885,.F.);
#17643=ORIENTED_EDGE('',*,*,#11874,.F.);
#17644=ORIENTED_EDGE('',*,*,#11900,.F.);
#17645=ORIENTED_EDGE('',*,*,#11901,.F.);
#17646=ORIENTED_EDGE('',*,*,#11902,.F.);
#17647=ORIENTED_EDGE('',*,*,#11903,.F.);
#17648=ORIENTED_EDGE('',*,*,#11904,.F.);
#17649=ORIENTED_EDGE('',*,*,#11882,.F.);
#17650=ORIENTED_EDGE('',*,*,#11905,.T.);
#17651=ORIENTED_EDGE('',*,*,#11906,.T.);
#17652=ORIENTED_EDGE('',*,*,#11907,.T.);
#17653=ORIENTED_EDGE('',*,*,#11908,.T.);
#17654=ORIENTED_EDGE('',*,*,#11909,.T.);
#17655=ORIENTED_EDGE('',*,*,#11910,.T.);
#17656=ORIENTED_EDGE('',*,*,#11872,.T.);
#17657=ORIENTED_EDGE('',*,*,#11911,.T.);
#17658=ORIENTED_EDGE('',*,*,#11908,.F.);
#17659=ORIENTED_EDGE('',*,*,#11912,.T.);
#17660=ORIENTED_EDGE('',*,*,#11913,.T.);
#17661=ORIENTED_EDGE('',*,*,#11914,.T.);
#17662=ORIENTED_EDGE('',*,*,#11910,.F.);
#17663=ORIENTED_EDGE('',*,*,#11915,.T.);
#17664=ORIENTED_EDGE('',*,*,#11916,.T.);
#17665=ORIENTED_EDGE('',*,*,#11917,.T.);
#17666=ORIENTED_EDGE('',*,*,#11915,.F.);
#17667=ORIENTED_EDGE('',*,*,#11918,.T.);
#17668=ORIENTED_EDGE('',*,*,#11913,.F.);
#17669=ORIENTED_EDGE('',*,*,#11919,.T.);
#17670=ORIENTED_EDGE('',*,*,#11911,.F.);
#17671=ORIENTED_EDGE('',*,*,#11920,.T.);
#17672=ORIENTED_EDGE('',*,*,#11905,.F.);
#17673=ORIENTED_EDGE('',*,*,#11921,.T.);
#17674=ORIENTED_EDGE('',*,*,#11912,.F.);
#17675=ORIENTED_EDGE('',*,*,#11871,.T.);
#17676=ORIENTED_EDGE('',*,*,#11922,.F.);
#17677=ORIENTED_EDGE('',*,*,#11923,.T.);
#17678=ORIENTED_EDGE('',*,*,#11924,.T.);
#17679=ORIENTED_EDGE('',*,*,#11914,.F.);
#17680=ORIENTED_EDGE('',*,*,#11925,.T.);
#17681=ORIENTED_EDGE('',*,*,#11901,.T.);
#17682=ORIENTED_EDGE('',*,*,#11899,.F.);
#17683=ORIENTED_EDGE('',*,*,#11873,.T.);
#17684=ORIENTED_EDGE('',*,*,#11918,.F.);
#17685=ORIENTED_EDGE('',*,*,#11926,.F.);
#17686=ORIENTED_EDGE('',*,*,#11927,.F.);
#17687=ORIENTED_EDGE('',*,*,#11928,.T.);
#17688=ORIENTED_EDGE('',*,*,#11902,.T.);
#17689=ORIENTED_EDGE('',*,*,#11925,.F.);
#17690=ORIENTED_EDGE('',*,*,#11917,.F.);
#17691=ORIENTED_EDGE('',*,*,#11929,.T.);
#17692=ORIENTED_EDGE('',*,*,#11930,.T.);
#17693=ORIENTED_EDGE('',*,*,#11926,.T.);
#17694=ORIENTED_EDGE('',*,*,#11931,.T.);
#17695=ORIENTED_EDGE('',*,*,#11932,.T.);
#17696=ORIENTED_EDGE('',*,*,#11866,.F.);
#17697=ORIENTED_EDGE('',*,*,#11880,.F.);
#17698=ORIENTED_EDGE('',*,*,#11856,.T.);
#17699=ORIENTED_EDGE('',*,*,#11931,.F.);
#17700=ORIENTED_EDGE('',*,*,#11859,.T.);
#17701=ORIENTED_EDGE('',*,*,#11854,.F.);
#17702=ORIENTED_EDGE('',*,*,#11933,.F.);
#17703=ORIENTED_EDGE('',*,*,#11934,.F.);
#17704=ORIENTED_EDGE('',*,*,#11935,.F.);
#17705=ORIENTED_EDGE('',*,*,#11846,.T.);
#17706=ORIENTED_EDGE('',*,*,#11863,.T.);
#17707=ORIENTED_EDGE('',*,*,#11936,.T.);
#17708=ORIENTED_EDGE('',*,*,#11843,.F.);
#17709=ORIENTED_EDGE('',*,*,#11937,.T.);
#17710=ORIENTED_EDGE('',*,*,#11938,.T.);
#17711=ORIENTED_EDGE('',*,*,#11937,.F.);
#17712=ORIENTED_EDGE('',*,*,#11939,.T.);
#17713=ORIENTED_EDGE('',*,*,#11940,.T.);
#17714=ORIENTED_EDGE('',*,*,#11941,.T.);
#17715=ORIENTED_EDGE('',*,*,#11847,.F.);
#17716=ORIENTED_EDGE('',*,*,#11942,.F.);
#17717=ORIENTED_EDGE('',*,*,#11943,.T.);
#17718=ORIENTED_EDGE('',*,*,#11944,.F.);
#17719=ORIENTED_EDGE('',*,*,#11939,.F.);
#17720=ORIENTED_EDGE('',*,*,#11842,.F.);
#17721=ORIENTED_EDGE('',*,*,#11936,.F.);
#17722=ORIENTED_EDGE('',*,*,#11879,.T.);
#17723=ORIENTED_EDGE('',*,*,#11945,.T.);
#17724=ORIENTED_EDGE('',*,*,#11946,.T.);
#17725=ORIENTED_EDGE('',*,*,#11942,.T.);
#17726=ORIENTED_EDGE('',*,*,#11947,.T.);
#17727=ORIENTED_EDGE('',*,*,#11898,.F.);
#17728=ORIENTED_EDGE('',*,*,#11948,.T.);
#17729=ORIENTED_EDGE('',*,*,#11949,.T.);
#17730=ORIENTED_EDGE('',*,*,#11896,.T.);
#17731=ORIENTED_EDGE('',*,*,#11947,.F.);
#17732=ORIENTED_EDGE('',*,*,#11950,.T.);
#17733=ORIENTED_EDGE('',*,*,#11877,.T.);
#17734=ORIENTED_EDGE('',*,*,#11951,.T.);
#17735=ORIENTED_EDGE('',*,*,#11952,.T.);
#17736=ORIENTED_EDGE('',*,*,#11953,.T.);
#17737=ORIENTED_EDGE('',*,*,#11954,.T.);
#17738=ORIENTED_EDGE('',*,*,#11878,.T.);
#17739=ORIENTED_EDGE('',*,*,#11954,.F.);
#17740=ORIENTED_EDGE('',*,*,#11955,.T.);
#17741=ORIENTED_EDGE('',*,*,#11945,.F.);
#17742=ORIENTED_EDGE('',*,*,#11951,.F.);
#17743=ORIENTED_EDGE('',*,*,#11894,.T.);
#17744=ORIENTED_EDGE('',*,*,#11949,.F.);
#17745=ORIENTED_EDGE('',*,*,#11952,.F.);
#17746=ORIENTED_EDGE('',*,*,#11950,.F.);
#17747=ORIENTED_EDGE('',*,*,#11956,.F.);
#17748=ORIENTED_EDGE('',*,*,#11957,.F.);
#17749=ORIENTED_EDGE('',*,*,#11958,.F.);
#17750=ORIENTED_EDGE('',*,*,#11959,.T.);
#17751=ORIENTED_EDGE('',*,*,#11948,.F.);
#17752=ORIENTED_EDGE('',*,*,#11960,.T.);
#17753=ORIENTED_EDGE('',*,*,#11961,.T.);
#17754=ORIENTED_EDGE('',*,*,#11956,.T.);
#17755=ORIENTED_EDGE('',*,*,#11897,.F.);
#17756=ORIENTED_EDGE('',*,*,#11962,.F.);
#17757=ORIENTED_EDGE('',*,*,#11963,.F.);
#17758=ORIENTED_EDGE('',*,*,#11960,.F.);
#17759=ORIENTED_EDGE('',*,*,#11889,.F.);
#17760=ORIENTED_EDGE('',*,*,#11964,.T.);
#17761=ORIENTED_EDGE('',*,*,#11965,.T.);
#17762=ORIENTED_EDGE('',*,*,#11962,.T.);
#17763=ORIENTED_EDGE('',*,*,#11965,.F.);
#17764=ORIENTED_EDGE('',*,*,#11966,.T.);
#17765=ORIENTED_EDGE('',*,*,#11967,.T.);
#17766=ORIENTED_EDGE('',*,*,#11968,.T.);
#17767=ORIENTED_EDGE('',*,*,#11969,.T.);
#17768=ORIENTED_EDGE('',*,*,#11922,.T.);
#17769=ORIENTED_EDGE('',*,*,#11870,.T.);
#17770=ORIENTED_EDGE('',*,*,#11969,.F.);
#17771=ORIENTED_EDGE('',*,*,#11970,.F.);
#17772=ORIENTED_EDGE('',*,*,#11971,.F.);
#17773=ORIENTED_EDGE('',*,*,#11972,.F.);
#17774=ORIENTED_EDGE('',*,*,#11973,.F.);
#17775=ORIENTED_EDGE('',*,*,#11923,.F.);
#17776=ORIENTED_EDGE('',*,*,#11974,.F.);
#17777=ORIENTED_EDGE('',*,*,#11975,.T.);
#17778=ORIENTED_EDGE('',*,*,#11976,.T.);
#17779=ORIENTED_EDGE('',*,*,#11977,.T.);
#17780=ORIENTED_EDGE('',*,*,#11972,.T.);
#17781=ORIENTED_EDGE('',*,*,#11978,.F.);
#17782=ORIENTED_EDGE('',*,*,#11967,.F.);
#17783=ORIENTED_EDGE('',*,*,#11979,.T.);
#17784=ORIENTED_EDGE('',*,*,#11980,.T.);
#17785=ORIENTED_EDGE('',*,*,#11963,.T.);
#17786=ORIENTED_EDGE('',*,*,#11966,.F.);
#17787=ORIENTED_EDGE('',*,*,#11981,.T.);
#17788=ORIENTED_EDGE('',*,*,#11982,.T.);
#17789=ORIENTED_EDGE('',*,*,#11983,.T.);
#17790=ORIENTED_EDGE('',*,*,#11903,.T.);
#17791=ORIENTED_EDGE('',*,*,#11928,.F.);
#17792=ORIENTED_EDGE('',*,*,#11984,.F.);
#17793=ORIENTED_EDGE('',*,*,#11985,.T.);
#17794=ORIENTED_EDGE('',*,*,#11982,.F.);
#17795=ORIENTED_EDGE('',*,*,#11986,.T.);
#17796=ORIENTED_EDGE('',*,*,#11980,.F.);
#17797=ORIENTED_EDGE('',*,*,#11987,.T.);
#17798=ORIENTED_EDGE('',*,*,#11961,.F.);
#17799=ORIENTED_EDGE('',*,*,#11987,.F.);
#17800=ORIENTED_EDGE('',*,*,#11988,.T.);
#17801=ORIENTED_EDGE('',*,*,#11989,.T.);
#17802=ORIENTED_EDGE('',*,*,#11957,.T.);
#17803=ORIENTED_EDGE('',*,*,#11990,.F.);
#17804=ORIENTED_EDGE('',*,*,#11781,.T.);
#17805=ORIENTED_EDGE('',*,*,#11991,.T.);
#17806=ORIENTED_EDGE('',*,*,#11992,.F.);
#17807=ORIENTED_EDGE('',*,*,#11993,.F.);
#17808=ORIENTED_EDGE('',*,*,#11775,.T.);
#17809=ORIENTED_EDGE('',*,*,#11994,.T.);
#17810=ORIENTED_EDGE('',*,*,#11995,.F.);
#17811=ORIENTED_EDGE('',*,*,#11996,.F.);
#17812=ORIENTED_EDGE('',*,*,#11769,.T.);
#17813=ORIENTED_EDGE('',*,*,#11997,.T.);
#17814=ORIENTED_EDGE('',*,*,#11998,.F.);
#17815=ORIENTED_EDGE('',*,*,#11999,.F.);
#17816=ORIENTED_EDGE('',*,*,#12000,.F.);
#17817=ORIENTED_EDGE('',*,*,#11941,.F.);
#17818=ORIENTED_EDGE('',*,*,#12001,.F.);
#17819=ORIENTED_EDGE('',*,*,#11988,.F.);
#17820=ORIENTED_EDGE('',*,*,#11979,.F.);
#17821=ORIENTED_EDGE('',*,*,#11983,.F.);
#17822=ORIENTED_EDGE('',*,*,#11985,.F.);
#17823=ORIENTED_EDGE('',*,*,#12002,.T.);
#17824=ORIENTED_EDGE('',*,*,#12003,.F.);
#17825=ORIENTED_EDGE('',*,*,#12004,.T.);
#17826=ORIENTED_EDGE('',*,*,#11975,.F.);
#17827=ORIENTED_EDGE('',*,*,#12005,.T.);
#17828=ORIENTED_EDGE('',*,*,#12006,.F.);
#17829=ORIENTED_EDGE('',*,*,#12007,.F.);
#17830=ORIENTED_EDGE('',*,*,#12008,.F.);
#17831=ORIENTED_EDGE('',*,*,#11997,.F.);
#17832=ORIENTED_EDGE('',*,*,#11768,.T.);
#17833=ORIENTED_EDGE('',*,*,#12009,.F.);
#17834=ORIENTED_EDGE('',*,*,#12010,.F.);
#17835=ORIENTED_EDGE('',*,*,#12011,.F.);
#17836=ORIENTED_EDGE('',*,*,#11762,.T.);
#17837=ORIENTED_EDGE('',*,*,#12012,.T.);
#17838=ORIENTED_EDGE('',*,*,#12013,.F.);
#17839=ORIENTED_EDGE('',*,*,#12014,.T.);
#17840=ORIENTED_EDGE('',*,*,#11782,.T.);
#17841=ORIENTED_EDGE('',*,*,#11990,.T.);
#17842=ORIENTED_EDGE('',*,*,#12015,.T.);
#17843=ORIENTED_EDGE('',*,*,#12013,.T.);
#17844=ORIENTED_EDGE('',*,*,#12016,.T.);
#17845=ORIENTED_EDGE('',*,*,#12017,.T.);
#17846=ORIENTED_EDGE('',*,*,#12018,.T.);
#17847=ORIENTED_EDGE('',*,*,#12019,.T.);
#17848=ORIENTED_EDGE('',*,*,#12015,.F.);
#17849=ORIENTED_EDGE('',*,*,#12018,.F.);
#17850=ORIENTED_EDGE('',*,*,#12020,.T.);
#17851=ORIENTED_EDGE('',*,*,#12021,.T.);
#17852=ORIENTED_EDGE('',*,*,#12022,.T.);
#17853=ORIENTED_EDGE('',*,*,#12023,.T.);
#17854=ORIENTED_EDGE('',*,*,#11770,.T.);
#17855=ORIENTED_EDGE('',*,*,#11996,.T.);
#17856=ORIENTED_EDGE('',*,*,#12024,.T.);
#17857=ORIENTED_EDGE('',*,*,#11995,.T.);
#17858=ORIENTED_EDGE('',*,*,#12025,.T.);
#17859=ORIENTED_EDGE('',*,*,#12026,.T.);
#17860=ORIENTED_EDGE('',*,*,#12027,.T.);
#17861=ORIENTED_EDGE('',*,*,#12028,.T.);
#17862=ORIENTED_EDGE('',*,*,#12024,.F.);
#17863=ORIENTED_EDGE('',*,*,#12027,.F.);
#17864=ORIENTED_EDGE('',*,*,#12029,.T.);
#17865=ORIENTED_EDGE('',*,*,#12030,.T.);
#17866=ORIENTED_EDGE('',*,*,#12031,.T.);
#17867=ORIENTED_EDGE('',*,*,#11840,.F.);
#17868=ORIENTED_EDGE('',*,*,#11999,.T.);
#17869=ORIENTED_EDGE('',*,*,#12032,.T.);
#17870=ORIENTED_EDGE('',*,*,#11852,.T.);
#17871=ORIENTED_EDGE('',*,*,#12006,.T.);
#17872=ORIENTED_EDGE('',*,*,#12033,.T.);
#17873=ORIENTED_EDGE('',*,*,#12034,.T.);
#17874=ORIENTED_EDGE('',*,*,#12035,.T.);
#17875=ORIENTED_EDGE('',*,*,#12036,.T.);
#17876=ORIENTED_EDGE('',*,*,#12033,.F.);
#17877=ORIENTED_EDGE('',*,*,#12037,.T.);
#17878=ORIENTED_EDGE('',*,*,#12038,.T.);
#17879=ORIENTED_EDGE('',*,*,#12007,.T.);
#17880=ORIENTED_EDGE('',*,*,#12036,.F.);
#17881=ORIENTED_EDGE('',*,*,#12039,.T.);
#17882=ORIENTED_EDGE('',*,*,#12040,.T.);
#17883=ORIENTED_EDGE('',*,*,#11998,.T.);
#17884=ORIENTED_EDGE('',*,*,#12008,.T.);
#17885=ORIENTED_EDGE('',*,*,#12040,.F.);
#17886=ORIENTED_EDGE('',*,*,#12041,.T.);
#17887=ORIENTED_EDGE('',*,*,#11933,.T.);
#17888=ORIENTED_EDGE('',*,*,#11853,.T.);
#17889=ORIENTED_EDGE('',*,*,#12032,.F.);
#17890=ORIENTED_EDGE('',*,*,#11839,.F.);
#17891=ORIENTED_EDGE('',*,*,#11861,.T.);
#17892=ORIENTED_EDGE('',*,*,#11938,.F.);
#17893=ORIENTED_EDGE('',*,*,#12000,.T.);
#17894=ORIENTED_EDGE('',*,*,#12001,.T.);
#17895=ORIENTED_EDGE('',*,*,#11940,.F.);
#17896=ORIENTED_EDGE('',*,*,#11944,.T.);
#17897=ORIENTED_EDGE('',*,*,#12042,.T.);
#17898=ORIENTED_EDGE('',*,*,#11958,.T.);
#17899=ORIENTED_EDGE('',*,*,#11989,.F.);
#17900=ORIENTED_EDGE('',*,*,#11955,.F.);
#17901=ORIENTED_EDGE('',*,*,#11953,.F.);
#17902=ORIENTED_EDGE('',*,*,#11959,.F.);
#17903=ORIENTED_EDGE('',*,*,#12042,.F.);
#17904=ORIENTED_EDGE('',*,*,#11943,.F.);
#17905=ORIENTED_EDGE('',*,*,#11946,.F.);
#17906=ORIENTED_EDGE('',*,*,#12037,.F.);
#17907=ORIENTED_EDGE('',*,*,#12005,.F.);
#17908=ORIENTED_EDGE('',*,*,#11974,.T.);
#17909=ORIENTED_EDGE('',*,*,#12043,.T.);
#17910=ORIENTED_EDGE('',*,*,#12038,.F.);
#17911=ORIENTED_EDGE('',*,*,#12044,.T.);
#17912=ORIENTED_EDGE('',*,*,#12045,.T.);
#17913=ORIENTED_EDGE('',*,*,#12046,.T.);
#17914=ORIENTED_EDGE('',*,*,#12047,.T.);
#17915=ORIENTED_EDGE('',*,*,#12045,.F.);
#17916=ORIENTED_EDGE('',*,*,#12048,.T.);
#17917=ORIENTED_EDGE('',*,*,#12048,.F.);
#17918=ORIENTED_EDGE('',*,*,#12049,.T.);
#17919=ORIENTED_EDGE('',*,*,#11970,.T.);
#17920=ORIENTED_EDGE('',*,*,#11968,.F.);
#17921=ORIENTED_EDGE('',*,*,#11869,.T.);
#17922=ORIENTED_EDGE('',*,*,#12044,.F.);
#17923=ORIENTED_EDGE('',*,*,#12043,.F.);
#17924=ORIENTED_EDGE('',*,*,#11978,.T.);
#17925=ORIENTED_EDGE('',*,*,#11971,.T.);
#17926=ORIENTED_EDGE('',*,*,#12049,.F.);
#17927=ORIENTED_EDGE('',*,*,#11907,.F.);
#17928=ORIENTED_EDGE('',*,*,#12050,.T.);
#17929=ORIENTED_EDGE('',*,*,#11916,.F.);
#17930=ORIENTED_EDGE('',*,*,#12051,.T.);
#17931=ORIENTED_EDGE('',*,*,#12050,.F.);
#17932=ORIENTED_EDGE('',*,*,#12052,.F.);
#17933=ORIENTED_EDGE('',*,*,#12053,.F.);
#17934=ORIENTED_EDGE('',*,*,#11929,.F.);
#17935=ORIENTED_EDGE('',*,*,#11906,.F.);
#17936=ORIENTED_EDGE('',*,*,#12054,.T.);
#17937=ORIENTED_EDGE('',*,*,#12055,.T.);
#17938=ORIENTED_EDGE('',*,*,#12052,.T.);
#17939=ORIENTED_EDGE('',*,*,#12056,.F.);
#17940=ORIENTED_EDGE('',*,*,#12057,.F.);
#17941=ORIENTED_EDGE('',*,*,#12055,.F.);
#17942=ORIENTED_EDGE('',*,*,#12058,.F.);
#17943=ORIENTED_EDGE('',*,*,#12059,.F.);
#17944=ORIENTED_EDGE('',*,*,#11930,.F.);
#17945=ORIENTED_EDGE('',*,*,#11927,.T.);
#17946=ORIENTED_EDGE('',*,*,#12059,.T.);
#17947=ORIENTED_EDGE('',*,*,#12002,.F.);
#17948=ORIENTED_EDGE('',*,*,#11984,.T.);
#17949=ORIENTED_EDGE('',*,*,#12058,.T.);
#17950=ORIENTED_EDGE('',*,*,#12053,.T.);
#17951=ORIENTED_EDGE('',*,*,#12057,.T.);
#17952=ORIENTED_EDGE('',*,*,#12003,.T.);
#17953=ORIENTED_EDGE('',*,*,#12004,.F.);
#17954=ORIENTED_EDGE('',*,*,#12056,.T.);
#17955=ORIENTED_EDGE('',*,*,#12060,.T.);
#17956=ORIENTED_EDGE('',*,*,#11976,.F.);
#17957=ORIENTED_EDGE('',*,*,#11920,.F.);
#17958=ORIENTED_EDGE('',*,*,#11924,.F.);
#17959=ORIENTED_EDGE('',*,*,#11973,.T.);
#17960=ORIENTED_EDGE('',*,*,#11977,.F.);
#17961=ORIENTED_EDGE('',*,*,#12060,.F.);
#17962=ORIENTED_EDGE('',*,*,#12054,.F.);
#17963=ORIENTED_EDGE('',*,*,#12034,.F.);
#17964=ORIENTED_EDGE('',*,*,#12046,.F.);
#17965=ORIENTED_EDGE('',*,*,#12061,.F.);
#17966=ORIENTED_EDGE('',*,*,#12062,.F.);
#17967=ORIENTED_EDGE('',*,*,#12063,.T.);
#17968=ORIENTED_EDGE('',*,*,#12064,.T.);
#17969=ORIENTED_EDGE('',*,*,#11867,.T.);
#17970=ORIENTED_EDGE('',*,*,#11932,.F.);
#17971=ORIENTED_EDGE('',*,*,#11935,.T.);
#17972=ORIENTED_EDGE('',*,*,#12065,.T.);
#17973=ORIENTED_EDGE('',*,*,#12062,.T.);
#17974=ORIENTED_EDGE('',*,*,#12035,.F.);
#17975=ORIENTED_EDGE('',*,*,#12063,.F.);
#17976=ORIENTED_EDGE('',*,*,#12065,.F.);
#17977=ORIENTED_EDGE('',*,*,#11934,.T.);
#17978=ORIENTED_EDGE('',*,*,#12041,.F.);
#17979=ORIENTED_EDGE('',*,*,#12039,.F.);
#17980=ORIENTED_EDGE('',*,*,#12066,.T.);
#17981=ORIENTED_EDGE('',*,*,#12067,.T.);
#17982=ORIENTED_EDGE('',*,*,#11776,.T.);
#17983=ORIENTED_EDGE('',*,*,#11993,.T.);
#17984=ORIENTED_EDGE('',*,*,#11777,.F.);
#17985=ORIENTED_EDGE('',*,*,#12067,.F.);
#17986=ORIENTED_EDGE('',*,*,#12068,.F.);
#17987=ORIENTED_EDGE('',*,*,#12069,.F.);
#17988=ORIENTED_EDGE('',*,*,#12070,.T.);
#17989=ORIENTED_EDGE('',*,*,#12071,.F.);
#17990=ORIENTED_EDGE('',*,*,#12072,.T.);
#17991=ORIENTED_EDGE('',*,*,#12073,.T.);
#17992=ORIENTED_EDGE('',*,*,#12074,.F.);
#17993=ORIENTED_EDGE('',*,*,#12075,.F.);
#17994=ORIENTED_EDGE('',*,*,#12076,.F.);
#17995=ORIENTED_EDGE('',*,*,#11791,.F.);
#17996=ORIENTED_EDGE('',*,*,#11820,.F.);
#17997=ORIENTED_EDGE('',*,*,#11816,.F.);
#17998=ORIENTED_EDGE('',*,*,#11813,.F.);
#17999=ORIENTED_EDGE('',*,*,#12077,.T.);
#18000=ORIENTED_EDGE('',*,*,#12078,.T.);
#18001=ORIENTED_EDGE('',*,*,#12068,.T.);
#18002=ORIENTED_EDGE('',*,*,#12066,.F.);
#18003=ORIENTED_EDGE('',*,*,#11992,.T.);
#18004=ORIENTED_EDGE('',*,*,#12079,.T.);
#18005=ORIENTED_EDGE('',*,*,#12078,.F.);
#18006=ORIENTED_EDGE('',*,*,#12080,.T.);
#18007=ORIENTED_EDGE('',*,*,#12081,.T.);
#18008=ORIENTED_EDGE('',*,*,#12069,.T.);
#18009=ORIENTED_EDGE('',*,*,#12082,.T.);
#18010=ORIENTED_EDGE('',*,*,#12083,.T.);
#18011=ORIENTED_EDGE('',*,*,#12084,.T.);
#18012=ORIENTED_EDGE('',*,*,#11881,.T.);
#18013=ORIENTED_EDGE('',*,*,#11864,.T.);
#18014=ORIENTED_EDGE('',*,*,#12084,.F.);
#18015=ORIENTED_EDGE('',*,*,#12085,.F.);
#18016=ORIENTED_EDGE('',*,*,#12086,.F.);
#18017=ORIENTED_EDGE('',*,*,#12087,.T.);
#18018=ORIENTED_EDGE('',*,*,#12082,.F.);
#18019=ORIENTED_EDGE('',*,*,#12083,.F.);
#18020=ORIENTED_EDGE('',*,*,#12087,.F.);
#18021=ORIENTED_EDGE('',*,*,#12088,.F.);
#18022=ORIENTED_EDGE('',*,*,#12089,.F.);
#18023=ORIENTED_EDGE('',*,*,#12090,.F.);
#18024=ORIENTED_EDGE('',*,*,#12091,.F.);
#18025=ORIENTED_EDGE('',*,*,#12092,.F.);
#18026=ORIENTED_EDGE('',*,*,#12072,.F.);
#18027=ORIENTED_EDGE('',*,*,#12093,.F.);
#18028=ORIENTED_EDGE('',*,*,#12094,.F.);
#18029=ORIENTED_EDGE('',*,*,#12095,.F.);
#18030=ORIENTED_EDGE('',*,*,#12096,.F.);
#18031=ORIENTED_EDGE('',*,*,#12097,.F.);
#18032=ORIENTED_EDGE('',*,*,#11774,.T.);
#18033=ORIENTED_EDGE('',*,*,#12098,.T.);
#18034=ORIENTED_EDGE('',*,*,#12025,.F.);
#18035=ORIENTED_EDGE('',*,*,#11994,.F.);
#18036=ORIENTED_EDGE('',*,*,#12098,.F.);
#18037=ORIENTED_EDGE('',*,*,#11773,.F.);
#18038=ORIENTED_EDGE('',*,*,#11823,.F.);
#18039=ORIENTED_EDGE('',*,*,#11826,.T.);
#18040=ORIENTED_EDGE('',*,*,#11827,.F.);
#18041=ORIENTED_EDGE('',*,*,#11793,.F.);
#18042=ORIENTED_EDGE('',*,*,#12099,.F.);
#18043=ORIENTED_EDGE('',*,*,#12100,.F.);
#18044=ORIENTED_EDGE('',*,*,#12101,.T.);
#18045=ORIENTED_EDGE('',*,*,#12102,.T.);
#18046=ORIENTED_EDGE('',*,*,#12091,.T.);
#18047=ORIENTED_EDGE('',*,*,#12103,.T.);
#18048=ORIENTED_EDGE('',*,*,#12104,.F.);
#18049=ORIENTED_EDGE('',*,*,#12029,.F.);
#18050=ORIENTED_EDGE('',*,*,#12026,.F.);
#18051=ORIENTED_EDGE('',*,*,#11780,.T.);
#18052=ORIENTED_EDGE('',*,*,#12105,.T.);
#18053=ORIENTED_EDGE('',*,*,#12079,.F.);
#18054=ORIENTED_EDGE('',*,*,#11991,.F.);
#18055=ORIENTED_EDGE('',*,*,#12105,.F.);
#18056=ORIENTED_EDGE('',*,*,#11779,.F.);
#18057=ORIENTED_EDGE('',*,*,#11815,.F.);
#18058=ORIENTED_EDGE('',*,*,#11818,.T.);
#18059=ORIENTED_EDGE('',*,*,#11819,.F.);
#18060=ORIENTED_EDGE('',*,*,#11789,.F.);
#18061=ORIENTED_EDGE('',*,*,#12106,.F.);
#18062=ORIENTED_EDGE('',*,*,#12107,.F.);
#18063=ORIENTED_EDGE('',*,*,#12108,.T.);
#18064=ORIENTED_EDGE('',*,*,#12109,.T.);
#18065=ORIENTED_EDGE('',*,*,#12094,.T.);
#18066=ORIENTED_EDGE('',*,*,#12110,.T.);
#18067=ORIENTED_EDGE('',*,*,#12111,.F.);
#18068=ORIENTED_EDGE('',*,*,#12080,.F.);
#18069=ORIENTED_EDGE('',*,*,#12077,.F.);
#18070=ORIENTED_EDGE('',*,*,#11761,.T.);
#18071=ORIENTED_EDGE('',*,*,#12112,.T.);
#18072=ORIENTED_EDGE('',*,*,#12016,.F.);
#18073=ORIENTED_EDGE('',*,*,#12012,.F.);
#18074=ORIENTED_EDGE('',*,*,#12112,.F.);
#18075=ORIENTED_EDGE('',*,*,#11760,.F.);
#18076=ORIENTED_EDGE('',*,*,#11807,.F.);
#18077=ORIENTED_EDGE('',*,*,#11810,.T.);
#18078=ORIENTED_EDGE('',*,*,#11811,.F.);
#18079=ORIENTED_EDGE('',*,*,#11803,.F.);
#18080=ORIENTED_EDGE('',*,*,#12113,.F.);
#18081=ORIENTED_EDGE('',*,*,#12114,.F.);
#18082=ORIENTED_EDGE('',*,*,#12115,.T.);
#18083=ORIENTED_EDGE('',*,*,#12116,.T.);
#18084=ORIENTED_EDGE('',*,*,#12085,.T.);
#18085=ORIENTED_EDGE('',*,*,#12117,.T.);
#18086=ORIENTED_EDGE('',*,*,#12118,.F.);
#18087=ORIENTED_EDGE('',*,*,#12020,.F.);
#18088=ORIENTED_EDGE('',*,*,#12017,.F.);
#18089=ORIENTED_EDGE('',*,*,#12119,.T.);
#18090=ORIENTED_EDGE('',*,*,#12120,.T.);
#18091=ORIENTED_EDGE('',*,*,#12121,.T.);
#18092=ORIENTED_EDGE('',*,*,#12122,.T.);
#18093=ORIENTED_EDGE('',*,*,#12123,.T.);
#18094=ORIENTED_EDGE('',*,*,#12114,.T.);
#18095=ORIENTED_EDGE('',*,*,#12124,.T.);
#18096=ORIENTED_EDGE('',*,*,#12125,.T.);
#18097=ORIENTED_EDGE('',*,*,#12126,.T.);
#18098=ORIENTED_EDGE('',*,*,#12125,.F.);
#18099=ORIENTED_EDGE('',*,*,#12127,.T.);
#18100=ORIENTED_EDGE('',*,*,#12121,.F.);
#18101=ORIENTED_EDGE('',*,*,#12127,.F.);
#18102=ORIENTED_EDGE('',*,*,#12128,.T.);
#18103=ORIENTED_EDGE('',*,*,#11801,.T.);
#18104=ORIENTED_EDGE('',*,*,#12129,.T.);
#18105=ORIENTED_EDGE('',*,*,#12124,.F.);
#18106=ORIENTED_EDGE('',*,*,#12113,.T.);
#18107=ORIENTED_EDGE('',*,*,#11802,.F.);
#18108=ORIENTED_EDGE('',*,*,#12128,.F.);
#18109=ORIENTED_EDGE('',*,*,#12126,.F.);
#18110=ORIENTED_EDGE('',*,*,#12120,.F.);
#18111=ORIENTED_EDGE('',*,*,#12130,.F.);
#18112=ORIENTED_EDGE('',*,*,#12115,.F.);
#18113=ORIENTED_EDGE('',*,*,#12117,.F.);
#18114=ORIENTED_EDGE('',*,*,#12097,.T.);
#18115=ORIENTED_EDGE('',*,*,#12131,.T.);
#18116=ORIENTED_EDGE('',*,*,#12132,.T.);
#18117=ORIENTED_EDGE('',*,*,#12132,.F.);
#18118=ORIENTED_EDGE('',*,*,#12133,.F.);
#18119=ORIENTED_EDGE('',*,*,#12021,.F.);
#18120=ORIENTED_EDGE('',*,*,#12118,.T.);
#18121=ORIENTED_EDGE('',*,*,#12134,.F.);
#18122=ORIENTED_EDGE('',*,*,#12095,.T.);
#18123=ORIENTED_EDGE('',*,*,#12109,.F.);
#18124=ORIENTED_EDGE('',*,*,#12135,.T.);
#18125=ORIENTED_EDGE('',*,*,#12136,.T.);
#18126=ORIENTED_EDGE('',*,*,#12135,.F.);
#18127=ORIENTED_EDGE('',*,*,#12108,.F.);
#18128=ORIENTED_EDGE('',*,*,#12137,.F.);
#18129=ORIENTED_EDGE('',*,*,#12107,.T.);
#18130=ORIENTED_EDGE('',*,*,#12138,.T.);
#18131=ORIENTED_EDGE('',*,*,#12139,.T.);
#18132=ORIENTED_EDGE('',*,*,#12137,.T.);
#18133=ORIENTED_EDGE('',*,*,#12110,.F.);
#18134=ORIENTED_EDGE('',*,*,#12093,.T.);
#18135=ORIENTED_EDGE('',*,*,#12071,.T.);
#18136=ORIENTED_EDGE('',*,*,#12140,.T.);
#18137=ORIENTED_EDGE('',*,*,#12140,.F.);
#18138=ORIENTED_EDGE('',*,*,#12070,.F.);
#18139=ORIENTED_EDGE('',*,*,#12081,.F.);
#18140=ORIENTED_EDGE('',*,*,#12111,.T.);
#18141=ORIENTED_EDGE('',*,*,#12073,.F.);
#18142=ORIENTED_EDGE('',*,*,#12092,.T.);
#18143=ORIENTED_EDGE('',*,*,#12102,.F.);
#18144=ORIENTED_EDGE('',*,*,#12141,.T.);
#18145=ORIENTED_EDGE('',*,*,#12074,.T.);
#18146=ORIENTED_EDGE('',*,*,#12141,.F.);
#18147=ORIENTED_EDGE('',*,*,#12101,.F.);
#18148=ORIENTED_EDGE('',*,*,#12142,.F.);
#18149=ORIENTED_EDGE('',*,*,#12100,.T.);
#18150=ORIENTED_EDGE('',*,*,#12143,.T.);
#18151=ORIENTED_EDGE('',*,*,#12075,.T.);
#18152=ORIENTED_EDGE('',*,*,#12142,.T.);
#18153=ORIENTED_EDGE('',*,*,#12103,.F.);
#18154=ORIENTED_EDGE('',*,*,#12090,.T.);
#18155=ORIENTED_EDGE('',*,*,#12144,.T.);
#18156=ORIENTED_EDGE('',*,*,#12145,.T.);
#18157=ORIENTED_EDGE('',*,*,#12145,.F.);
#18158=ORIENTED_EDGE('',*,*,#12146,.F.);
#18159=ORIENTED_EDGE('',*,*,#12030,.F.);
#18160=ORIENTED_EDGE('',*,*,#12104,.T.);
#18161=ORIENTED_EDGE('',*,*,#12147,.T.);
#18162=ORIENTED_EDGE('',*,*,#12148,.F.);
#18163=ORIENTED_EDGE('',*,*,#12149,.F.);
#18164=ORIENTED_EDGE('',*,*,#12150,.F.);
#18165=ORIENTED_EDGE('',*,*,#12151,.T.);
#18166=ORIENTED_EDGE('',*,*,#12150,.T.);
#18167=ORIENTED_EDGE('',*,*,#12152,.T.);
#18168=ORIENTED_EDGE('',*,*,#12153,.T.);
#18169=ORIENTED_EDGE('',*,*,#12154,.T.);
#18170=ORIENTED_EDGE('',*,*,#12155,.F.);
#18171=ORIENTED_EDGE('',*,*,#12156,.T.);
#18172=ORIENTED_EDGE('',*,*,#12157,.T.);
#18173=ORIENTED_EDGE('',*,*,#12149,.T.);
#18174=ORIENTED_EDGE('',*,*,#12157,.F.);
#18175=ORIENTED_EDGE('',*,*,#12158,.T.);
#18176=ORIENTED_EDGE('',*,*,#12152,.F.);
#18177=ORIENTED_EDGE('',*,*,#12153,.F.);
#18178=ORIENTED_EDGE('',*,*,#12159,.F.);
#18179=ORIENTED_EDGE('',*,*,#11796,.F.);
#18180=ORIENTED_EDGE('',*,*,#12160,.T.);
#18181=ORIENTED_EDGE('',*,*,#12158,.F.);
#18182=ORIENTED_EDGE('',*,*,#12161,.T.);
#18183=ORIENTED_EDGE('',*,*,#11797,.T.);
#18184=ORIENTED_EDGE('',*,*,#12159,.T.);
#18185=ORIENTED_EDGE('',*,*,#12156,.F.);
#18186=ORIENTED_EDGE('',*,*,#12162,.F.);
#18187=ORIENTED_EDGE('',*,*,#12163,.F.);
#18188=ORIENTED_EDGE('',*,*,#12164,.F.);
#18189=ORIENTED_EDGE('',*,*,#12165,.F.);
#18190=ORIENTED_EDGE('',*,*,#11766,.F.);
#18191=ORIENTED_EDGE('',*,*,#12166,.F.);
#18192=ORIENTED_EDGE('',*,*,#12167,.T.);
#18193=ORIENTED_EDGE('',*,*,#12168,.F.);
#18194=ORIENTED_EDGE('',*,*,#11798,.F.);
#18195=ORIENTED_EDGE('',*,*,#12161,.F.);
#18196=ORIENTED_EDGE('',*,*,#12169,.F.);
#18197=ORIENTED_EDGE('',*,*,#12170,.T.);
#18198=ORIENTED_EDGE('',*,*,#12171,.F.);
#18199=ORIENTED_EDGE('',*,*,#12154,.F.);
#18200=ORIENTED_EDGE('',*,*,#12148,.T.);
#18201=ORIENTED_EDGE('',*,*,#12172,.F.);
#18202=ORIENTED_EDGE('',*,*,#12088,.T.);
#18203=ORIENTED_EDGE('',*,*,#12086,.T.);
#18204=ORIENTED_EDGE('',*,*,#12116,.F.);
#18205=ORIENTED_EDGE('',*,*,#12130,.T.);
#18206=ORIENTED_EDGE('',*,*,#12119,.F.);
#18207=ORIENTED_EDGE('',*,*,#12170,.F.);
#18208=ORIENTED_EDGE('',*,*,#12169,.T.);
#18209=ORIENTED_EDGE('',*,*,#12123,.F.);
#18210=ORIENTED_EDGE('',*,*,#12173,.T.);
#18211=ORIENTED_EDGE('',*,*,#12155,.T.);
#18212=ORIENTED_EDGE('',*,*,#12171,.T.);
#18213=ORIENTED_EDGE('',*,*,#12122,.F.);
#18214=ORIENTED_EDGE('',*,*,#12129,.F.);
#18215=ORIENTED_EDGE('',*,*,#11800,.F.);
#18216=ORIENTED_EDGE('',*,*,#12174,.F.);
#18217=ORIENTED_EDGE('',*,*,#12175,.F.);
#18218=ORIENTED_EDGE('',*,*,#12176,.F.);
#18219=ORIENTED_EDGE('',*,*,#11764,.F.);
#18220=ORIENTED_EDGE('',*,*,#12177,.F.);
#18221=ORIENTED_EDGE('',*,*,#12178,.F.);
#18222=ORIENTED_EDGE('',*,*,#12179,.F.);
#18223=ORIENTED_EDGE('',*,*,#12180,.T.);
#18224=ORIENTED_EDGE('',*,*,#12173,.F.);
#18225=ORIENTED_EDGE('',*,*,#12180,.F.);
#18226=ORIENTED_EDGE('',*,*,#12181,.F.);
#18227=ORIENTED_EDGE('',*,*,#12162,.T.);
#18228=ORIENTED_EDGE('',*,*,#12176,.T.);
#18229=ORIENTED_EDGE('',*,*,#12182,.T.);
#18230=ORIENTED_EDGE('',*,*,#12166,.T.);
#18231=ORIENTED_EDGE('',*,*,#11765,.T.);
#18232=ORIENTED_EDGE('',*,*,#12182,.F.);
#18233=ORIENTED_EDGE('',*,*,#12175,.T.);
#18234=ORIENTED_EDGE('',*,*,#12183,.F.);
#18235=ORIENTED_EDGE('',*,*,#12167,.F.);
#18236=ORIENTED_EDGE('',*,*,#12168,.T.);
#18237=ORIENTED_EDGE('',*,*,#12183,.T.);
#18238=ORIENTED_EDGE('',*,*,#12174,.T.);
#18239=ORIENTED_EDGE('',*,*,#11799,.T.);
#18240=ORIENTED_EDGE('',*,*,#12009,.T.);
#18241=ORIENTED_EDGE('',*,*,#11767,.T.);
#18242=ORIENTED_EDGE('',*,*,#12165,.T.);
#18243=ORIENTED_EDGE('',*,*,#12184,.T.);
#18244=ORIENTED_EDGE('',*,*,#12177,.T.);
#18245=ORIENTED_EDGE('',*,*,#11763,.T.);
#18246=ORIENTED_EDGE('',*,*,#12011,.T.);
#18247=ORIENTED_EDGE('',*,*,#12185,.T.);
#18248=ORIENTED_EDGE('',*,*,#12186,.T.);
#18249=ORIENTED_EDGE('',*,*,#12178,.T.);
#18250=ORIENTED_EDGE('',*,*,#12185,.F.);
#18251=ORIENTED_EDGE('',*,*,#12010,.T.);
#18252=ORIENTED_EDGE('',*,*,#12184,.F.);
#18253=ORIENTED_EDGE('',*,*,#12164,.T.);
#18254=ORIENTED_EDGE('',*,*,#12186,.F.);
#18255=ORIENTED_EDGE('',*,*,#12163,.T.);
#18256=ORIENTED_EDGE('',*,*,#12181,.T.);
#18257=ORIENTED_EDGE('',*,*,#12179,.T.);
#18258=ORIENTED_EDGE('',*,*,#12023,.F.);
#18259=ORIENTED_EDGE('',*,*,#12028,.F.);
#18260=ORIENTED_EDGE('',*,*,#12031,.F.);
#18261=ORIENTED_EDGE('',*,*,#12146,.T.);
#18262=ORIENTED_EDGE('',*,*,#12144,.F.);
#18263=ORIENTED_EDGE('',*,*,#12089,.T.);
#18264=ORIENTED_EDGE('',*,*,#12172,.T.);
#18265=ORIENTED_EDGE('',*,*,#12147,.F.);
#18266=ORIENTED_EDGE('',*,*,#12151,.F.);
#18267=ORIENTED_EDGE('',*,*,#12160,.F.);
#18268=ORIENTED_EDGE('',*,*,#11795,.F.);
#18269=ORIENTED_EDGE('',*,*,#11828,.F.);
#18270=ORIENTED_EDGE('',*,*,#11824,.F.);
#18271=ORIENTED_EDGE('',*,*,#11821,.F.);
#18272=ORIENTED_EDGE('',*,*,#11771,.F.);
#18273=ORIENTED_EDGE('',*,*,#12014,.F.);
#18274=ORIENTED_EDGE('',*,*,#12019,.F.);
#18275=ORIENTED_EDGE('',*,*,#12022,.F.);
#18276=ORIENTED_EDGE('',*,*,#12133,.T.);
#18277=ORIENTED_EDGE('',*,*,#12131,.F.);
#18278=ORIENTED_EDGE('',*,*,#12096,.T.);
#18279=ORIENTED_EDGE('',*,*,#12134,.T.);
#18280=ORIENTED_EDGE('',*,*,#12136,.F.);
#18281=ORIENTED_EDGE('',*,*,#12139,.F.);
#18282=ORIENTED_EDGE('',*,*,#12187,.F.);
#18283=ORIENTED_EDGE('',*,*,#11787,.F.);
#18284=ORIENTED_EDGE('',*,*,#11812,.F.);
#18285=ORIENTED_EDGE('',*,*,#11808,.F.);
#18286=ORIENTED_EDGE('',*,*,#11805,.F.);
#18287=ORIENTED_EDGE('',*,*,#11783,.F.);
#18288=ORIENTED_EDGE('',*,*,#12138,.F.);
#18289=ORIENTED_EDGE('',*,*,#12106,.T.);
#18290=ORIENTED_EDGE('',*,*,#11788,.F.);
#18291=ORIENTED_EDGE('',*,*,#12187,.T.);
#18292=ORIENTED_EDGE('',*,*,#12143,.F.);
#18293=ORIENTED_EDGE('',*,*,#12099,.T.);
#18294=ORIENTED_EDGE('',*,*,#11792,.F.);
#18295=ORIENTED_EDGE('',*,*,#12076,.T.);
#18296=ORIENTED_EDGE('',*,*,#11883,.F.);
#18297=ORIENTED_EDGE('',*,*,#11904,.T.);
#18298=ORIENTED_EDGE('',*,*,#11986,.F.);
#18299=ORIENTED_EDGE('',*,*,#11981,.F.);
#18300=ORIENTED_EDGE('',*,*,#11964,.F.);
#18301=ORIENTED_EDGE('',*,*,#11892,.F.);
#18302=ORIENTED_EDGE('',*,*,#11921,.F.);
#18303=ORIENTED_EDGE('',*,*,#12051,.F.);
#18304=ORIENTED_EDGE('',*,*,#11919,.F.);
#18305=ORIENTED_EDGE('',*,*,#11909,.F.);
#18306=ORIENTED_EDGE('',*,*,#12047,.F.);
#18307=ORIENTED_EDGE('',*,*,#11868,.F.);
#18308=ORIENTED_EDGE('',*,*,#12064,.F.);
#18309=ORIENTED_EDGE('',*,*,#12061,.T.);
#18310=CYLINDRICAL_SURFACE('',#20143,6.933);
#18311=CYLINDRICAL_SURFACE('',#20153,6.933);
#18312=CYLINDRICAL_SURFACE('',#20154,6.933);
#18313=CYLINDRICAL_SURFACE('',#20155,6.933);
#18314=CYLINDRICAL_SURFACE('',#20156,6.933);
#18315=CYLINDRICAL_SURFACE('',#20157,6.933);
#18316=CYLINDRICAL_SURFACE('',#20158,6.933);
#18317=CYLINDRICAL_SURFACE('',#20159,6.933);
#18318=CYLINDRICAL_SURFACE('',#20160,6.933);
#18319=CYLINDRICAL_SURFACE('',#20161,6.933);
#18320=CYLINDRICAL_SURFACE('',#20162,6.933);
#18321=CYLINDRICAL_SURFACE('',#20163,6.933);
#18322=CYLINDRICAL_SURFACE('',#20164,6.933);
#18323=CYLINDRICAL_SURFACE('',#20165,6.933);
#18324=CYLINDRICAL_SURFACE('',#20166,6.933);
#18325=CYLINDRICAL_SURFACE('',#20167,6.933);
#18326=CYLINDRICAL_SURFACE('',#20168,6.933);
#18327=CYLINDRICAL_SURFACE('',#20169,6.933);
#18328=CYLINDRICAL_SURFACE('',#20170,6.933);
#18329=CYLINDRICAL_SURFACE('',#20171,6.933);
#18330=CYLINDRICAL_SURFACE('',#20172,6.933);
#18331=CYLINDRICAL_SURFACE('',#20173,6.933);
#18332=CYLINDRICAL_SURFACE('',#20174,6.933);
#18333=CYLINDRICAL_SURFACE('',#20175,6.933);
#18334=CYLINDRICAL_SURFACE('',#20176,6.933);
#18335=CYLINDRICAL_SURFACE('',#20177,6.933);
#18336=CYLINDRICAL_SURFACE('',#20178,6.933);
#18337=CYLINDRICAL_SURFACE('',#20179,6.933);
#18338=CYLINDRICAL_SURFACE('',#20180,6.933);
#18339=CYLINDRICAL_SURFACE('',#20181,6.933);
#18340=CYLINDRICAL_SURFACE('',#20182,6.933);
#18341=CYLINDRICAL_SURFACE('',#20183,6.933);
#18342=CYLINDRICAL_SURFACE('',#20184,6.933);
#18343=CYLINDRICAL_SURFACE('',#20185,6.933);
#18344=CYLINDRICAL_SURFACE('',#20186,6.933);
#18345=CYLINDRICAL_SURFACE('',#20187,6.933);
#18346=CYLINDRICAL_SURFACE('',#20188,6.933);
#18347=CYLINDRICAL_SURFACE('',#20189,6.933);
#18348=CYLINDRICAL_SURFACE('',#20190,6.933);
#18349=CYLINDRICAL_SURFACE('',#20191,6.933);
#18350=CYLINDRICAL_SURFACE('',#20192,6.933);
#18351=CYLINDRICAL_SURFACE('',#20193,6.933);
#18352=CYLINDRICAL_SURFACE('',#20194,6.933);
#18353=CYLINDRICAL_SURFACE('',#20195,6.933);
#18354=CYLINDRICAL_SURFACE('',#20196,6.933);
#18355=CYLINDRICAL_SURFACE('',#20197,6.933);
#18356=CYLINDRICAL_SURFACE('',#20198,6.933);
#18357=CYLINDRICAL_SURFACE('',#20199,6.933);
#18358=CYLINDRICAL_SURFACE('',#20200,6.933);
#18359=CYLINDRICAL_SURFACE('',#20201,6.933);
#18360=CYLINDRICAL_SURFACE('',#20202,6.933);
#18361=CYLINDRICAL_SURFACE('',#20203,6.933);
#18362=CYLINDRICAL_SURFACE('',#20204,6.933);
#18363=CYLINDRICAL_SURFACE('',#20205,6.933);
#18364=CYLINDRICAL_SURFACE('',#20206,6.933);
#18365=CYLINDRICAL_SURFACE('',#20207,6.933);
#18366=CYLINDRICAL_SURFACE('',#20208,6.933);
#18367=CYLINDRICAL_SURFACE('',#20209,6.933);
#18368=CYLINDRICAL_SURFACE('',#20210,6.933);
#18369=CYLINDRICAL_SURFACE('',#20211,6.933);
#18370=CYLINDRICAL_SURFACE('',#20212,6.933);
#18371=CYLINDRICAL_SURFACE('',#20213,6.933);
#18372=CYLINDRICAL_SURFACE('',#20214,6.933);
#18373=CYLINDRICAL_SURFACE('',#20218,6.933);
#18374=CYLINDRICAL_SURFACE('',#20219,6.933);
#18375=CYLINDRICAL_SURFACE('',#20220,6.933);
#18376=CYLINDRICAL_SURFACE('',#20221,6.933);
#18377=CYLINDRICAL_SURFACE('',#20222,6.933);
#18378=CYLINDRICAL_SURFACE('',#20223,6.933);
#18379=CYLINDRICAL_SURFACE('',#20224,6.933);
#18380=CYLINDRICAL_SURFACE('',#20225,6.933);
#18381=CYLINDRICAL_SURFACE('',#20226,6.933);
#18382=CYLINDRICAL_SURFACE('',#20227,6.933);
#18383=CYLINDRICAL_SURFACE('',#20228,6.933);
#18384=CYLINDRICAL_SURFACE('',#20229,6.933);
#18385=CYLINDRICAL_SURFACE('',#20230,6.933);
#18386=CYLINDRICAL_SURFACE('',#20231,6.933);
#18387=CYLINDRICAL_SURFACE('',#20232,6.933);
#18388=CYLINDRICAL_SURFACE('',#20233,6.21925);
#18389=CYLINDRICAL_SURFACE('',#20235,6.21925);
#18390=CYLINDRICAL_SURFACE('',#20236,6.21925);
#18391=CYLINDRICAL_SURFACE('',#20237,6.21925);
#18392=CYLINDRICAL_SURFACE('',#20238,6.21925);
#18393=CYLINDRICAL_SURFACE('',#20239,6.21925);
#18394=CYLINDRICAL_SURFACE('',#20240,6.21925);
#18395=CYLINDRICAL_SURFACE('',#20241,6.21925);
#18396=CYLINDRICAL_SURFACE('',#20242,6.21925);
#18397=CYLINDRICAL_SURFACE('',#20243,6.21925);
#18398=CYLINDRICAL_SURFACE('',#20244,6.21925);
#18399=CYLINDRICAL_SURFACE('',#20245,6.21925);
#18400=CYLINDRICAL_SURFACE('',#20246,6.21925);
#18401=CYLINDRICAL_SURFACE('',#20247,6.21925);
#18402=CYLINDRICAL_SURFACE('',#20248,6.21925);
#18403=CYLINDRICAL_SURFACE('',#20249,6.21925);
#18404=CYLINDRICAL_SURFACE('',#20250,6.21925);
#18405=CYLINDRICAL_SURFACE('',#20252,6.21925);
#18406=CYLINDRICAL_SURFACE('',#20254,6.21925);
#18407=CYLINDRICAL_SURFACE('',#20255,6.21925);
#18408=CYLINDRICAL_SURFACE('',#20256,6.21925);
#18409=CYLINDRICAL_SURFACE('',#20257,6.21925);
#18410=CYLINDRICAL_SURFACE('',#20258,6.21925);
#18411=CYLINDRICAL_SURFACE('',#20259,6.21925);
#18412=CYLINDRICAL_SURFACE('',#20260,6.21925);
#18413=CYLINDRICAL_SURFACE('',#20261,6.21925);
#18414=CYLINDRICAL_SURFACE('',#20262,6.21925);
#18415=CYLINDRICAL_SURFACE('',#20263,6.21925);
#18416=CYLINDRICAL_SURFACE('',#20264,6.21925);
#18417=CYLINDRICAL_SURFACE('',#20265,6.21925);
#18418=CYLINDRICAL_SURFACE('',#20266,6.21925);
#18419=CYLINDRICAL_SURFACE('',#20267,6.21925);
#18420=CYLINDRICAL_SURFACE('',#20268,6.21925);
#18421=CYLINDRICAL_SURFACE('',#20269,6.21925);
#18422=CYLINDRICAL_SURFACE('',#20270,6.21925);
#18423=CYLINDRICAL_SURFACE('',#20271,6.21925);
#18424=CYLINDRICAL_SURFACE('',#20272,6.21925);
#18425=CYLINDRICAL_SURFACE('',#20273,6.21925);
#18426=CYLINDRICAL_SURFACE('',#20274,6.21925);
#18427=CYLINDRICAL_SURFACE('',#20275,6.21925);
#18428=CYLINDRICAL_SURFACE('',#20276,6.21925);
#18429=CYLINDRICAL_SURFACE('',#20277,6.21925);
#18430=CYLINDRICAL_SURFACE('',#20278,6.21925);
#18431=CYLINDRICAL_SURFACE('',#20279,6.21925);
#18432=CYLINDRICAL_SURFACE('',#20280,6.21925);
#18433=CYLINDRICAL_SURFACE('',#20281,6.21925);
#18434=CYLINDRICAL_SURFACE('',#20282,6.21925);
#18435=CYLINDRICAL_SURFACE('',#20283,6.21925);
#18436=CYLINDRICAL_SURFACE('',#20284,6.21925);
#18437=CYLINDRICAL_SURFACE('',#20285,6.21925);
#18438=CYLINDRICAL_SURFACE('',#20286,6.21925);
#18439=CYLINDRICAL_SURFACE('',#20287,6.21925);
#18440=CYLINDRICAL_SURFACE('',#20288,6.21925);
#18441=CYLINDRICAL_SURFACE('',#20289,6.21925);
#18442=CYLINDRICAL_SURFACE('',#20290,6.21925);
#18443=CYLINDRICAL_SURFACE('',#20291,6.21925);
#18444=CYLINDRICAL_SURFACE('',#20292,6.21925);
#18445=CYLINDRICAL_SURFACE('',#20293,6.21925);
#18446=CYLINDRICAL_SURFACE('',#20294,6.21925);
#18447=CYLINDRICAL_SURFACE('',#20295,6.21925);
#18448=CYLINDRICAL_SURFACE('',#20296,6.21925);
#18449=CYLINDRICAL_SURFACE('',#20297,6.21925);
#18450=CYLINDRICAL_SURFACE('',#20298,6.21925);
#18451=CYLINDRICAL_SURFACE('',#20299,6.21925);
#18452=CYLINDRICAL_SURFACE('',#20300,6.21925);
#18453=CYLINDRICAL_SURFACE('',#20301,6.21925);
#18454=CYLINDRICAL_SURFACE('',#20302,6.21925);
#18455=CYLINDRICAL_SURFACE('',#20303,6.21925);
#18456=CYLINDRICAL_SURFACE('',#20304,6.21925);
#18457=CYLINDRICAL_SURFACE('',#20305,6.21925);
#18458=CYLINDRICAL_SURFACE('',#20306,6.21925);
#18459=CYLINDRICAL_SURFACE('',#20307,6.21925);
#18460=CYLINDRICAL_SURFACE('',#20308,6.21925);
#18461=CYLINDRICAL_SURFACE('',#20309,6.21925);
#18462=CYLINDRICAL_SURFACE('',#20310,6.21925);
#18463=CYLINDRICAL_SURFACE('',#20311,6.21925);
#18464=CYLINDRICAL_SURFACE('',#20312,6.21925);
#18465=CYLINDRICAL_SURFACE('',#20313,6.21925);
#18466=CYLINDRICAL_SURFACE('',#20314,6.21925);
#18467=CYLINDRICAL_SURFACE('',#20324,6.21925);
#18468=CYLINDRICAL_SURFACE('',#20330,6.21925);
#18469=CYLINDRICAL_SURFACE('',#20331,6.933);
#18470=CYLINDRICAL_SURFACE('',#20336,7.8125);
#18471=CYLINDRICAL_SURFACE('',#20346,10.625);
#18472=CYLINDRICAL_SURFACE('',#20353,7.8125);
#18473=CYLINDRICAL_SURFACE('',#20360,10.625);
#18474=CYLINDRICAL_SURFACE('',#20367,7.8125);
#18475=CYLINDRICAL_SURFACE('',#20374,10.625);
#18476=CYLINDRICAL_SURFACE('',#20381,7.8125);
#18477=CYLINDRICAL_SURFACE('',#20388,10.625);
#18478=CYLINDRICAL_SURFACE('',#20395,7.8125);
#18479=CYLINDRICAL_SURFACE('',#20402,10.625);
#18480=CYLINDRICAL_SURFACE('',#20409,7.8125);
#18481=CYLINDRICAL_SURFACE('',#20416,10.625);
#18482=CYLINDRICAL_SURFACE('',#20423,7.8125);
#18483=CYLINDRICAL_SURFACE('',#20430,10.625);
#18484=CYLINDRICAL_SURFACE('',#20438,7.8125);
#18485=CYLINDRICAL_SURFACE('',#20446,10.625);
#18486=CYLINDRICAL_SURFACE('',#20453,7.8125);
#18487=CYLINDRICAL_SURFACE('',#20460,10.625);
#18488=CYLINDRICAL_SURFACE('',#20467,7.8125);
#18489=CYLINDRICAL_SURFACE('',#20474,10.625);
#18490=CYLINDRICAL_SURFACE('',#20481,7.8125);
#18491=CYLINDRICAL_SURFACE('',#20488,10.625);
#18492=CYLINDRICAL_SURFACE('',#20495,7.8125);
#18493=CYLINDRICAL_SURFACE('',#20502,10.625);
#18494=CYLINDRICAL_SURFACE('',#20509,7.8125);
#18495=CYLINDRICAL_SURFACE('',#20516,10.625);
#18496=CYLINDRICAL_SURFACE('',#20523,7.8125);
#18497=CYLINDRICAL_SURFACE('',#20530,10.625);
#18498=CYLINDRICAL_SURFACE('',#20537,7.8125);
#18499=CYLINDRICAL_SURFACE('',#20544,10.625);
#18500=CYLINDRICAL_SURFACE('',#20550,6.933);
#18501=CYLINDRICAL_SURFACE('',#20556,0.5);
#18502=CYLINDRICAL_SURFACE('',#20563,0.5);
#18503=CYLINDRICAL_SURFACE('',#20566,0.5);
#18504=CYLINDRICAL_SURFACE('',#20576,0.5);
#18505=CYLINDRICAL_SURFACE('',#20578,0.5);
#18506=CYLINDRICAL_SURFACE('',#20583,0.5);
#18507=CYLINDRICAL_SURFACE('',#20586,0.5);
#18508=CYLINDRICAL_SURFACE('',#20589,0.5);
#18509=CYLINDRICAL_SURFACE('',#20592,0.5);
#18510=CYLINDRICAL_SURFACE('',#20593,0.5);
#18511=CYLINDRICAL_SURFACE('',#20598,0.5);
#18512=CYLINDRICAL_SURFACE('',#20601,0.5);
#18513=CYLINDRICAL_SURFACE('',#20610,0.5);
#18514=CYLINDRICAL_SURFACE('',#20614,0.5);
#18515=CYLINDRICAL_SURFACE('',#20622,0.5);
#18516=CYLINDRICAL_SURFACE('',#20623,0.5);
#18517=CYLINDRICAL_SURFACE('',#20625,0.5);
#18518=CYLINDRICAL_SURFACE('',#20627,0.5);
#18519=CYLINDRICAL_SURFACE('',#20629,0.5);
#18520=CYLINDRICAL_SURFACE('',#20634,0.5);
#18521=CYLINDRICAL_SURFACE('',#20638,0.5);
#18522=CYLINDRICAL_SURFACE('',#20641,0.5);
#18523=CYLINDRICAL_SURFACE('',#20644,0.5);
#18524=CYLINDRICAL_SURFACE('',#20648,0.5);
#18525=CYLINDRICAL_SURFACE('',#20652,0.5);
#18526=CYLINDRICAL_SURFACE('',#20656,0.5);
#18527=CYLINDRICAL_SURFACE('',#20659,0.5);
#18528=CYLINDRICAL_SURFACE('',#20662,0.5);
#18529=CYLINDRICAL_SURFACE('',#20671,0.5);
#18530=CYLINDRICAL_SURFACE('',#20676,0.5);
#18531=CYLINDRICAL_SURFACE('',#20681,0.5);
#18532=CYLINDRICAL_SURFACE('',#20685,0.5);
#18533=CYLINDRICAL_SURFACE('',#20688,0.5);
#18534=CYLINDRICAL_SURFACE('',#20691,0.5);
#18535=CYLINDRICAL_SURFACE('',#20694,0.5);
#18536=CYLINDRICAL_SURFACE('',#20696,0.5);
#18537=CYLINDRICAL_SURFACE('',#20699,0.5);
#18538=CYLINDRICAL_SURFACE('',#20705,0.5);
#18539=CYLINDRICAL_SURFACE('',#20712,0.5);
#18540=CYLINDRICAL_SURFACE('',#20714,0.5);
#18541=CYLINDRICAL_SURFACE('',#20716,0.5);
#18542=CYLINDRICAL_SURFACE('',#20719,0.5);
#18543=CYLINDRICAL_SURFACE('',#20724,0.5);
#18544=CYLINDRICAL_SURFACE('',#20729,0.5);
#18545=CYLINDRICAL_SURFACE('',#20730,0.5);
#18546=CYLINDRICAL_SURFACE('',#20734,0.5);
#18547=CYLINDRICAL_SURFACE('',#20739,0.5);
#18548=CYLINDRICAL_SURFACE('',#20741,0.5);
#18549=CYLINDRICAL_SURFACE('',#20744,0.5);
#18550=CYLINDRICAL_SURFACE('',#20751,0.5);
#18551=CYLINDRICAL_SURFACE('',#20755,0.5);
#18552=CYLINDRICAL_SURFACE('',#20758,0.5);
#18553=CYLINDRICAL_SURFACE('',#20761,0.5);
#18554=CYLINDRICAL_SURFACE('',#20772,0.5);
#18555=CYLINDRICAL_SURFACE('',#20774,0.5);
#18556=CYLINDRICAL_SURFACE('',#20776,0.5);
#18557=CYLINDRICAL_SURFACE('',#20779,0.5);
#18558=CYLINDRICAL_SURFACE('',#20781,0.5);
#18559=CYLINDRICAL_SURFACE('',#20789,0.499999999999999);
#18560=CYLINDRICAL_SURFACE('',#20792,0.5);
#18561=CYLINDRICAL_SURFACE('',#20795,0.5);
#18562=CYLINDRICAL_SURFACE('',#20798,0.499999999999999);
#18563=CYLINDRICAL_SURFACE('',#20801,0.5);
#18564=CYLINDRICAL_SURFACE('',#20803,0.5);
#18565=CYLINDRICAL_SURFACE('',#20806,0.5);
#18566=CYLINDRICAL_SURFACE('',#20811,0.5);
#18567=CYLINDRICAL_SURFACE('',#20817,0.5);
#18568=CYLINDRICAL_SURFACE('',#20821,0.499999999999999);
#18569=CYLINDRICAL_SURFACE('',#20826,0.5);
#18570=CYLINDRICAL_SURFACE('',#20829,0.5);
#18571=CYLINDRICAL_SURFACE('',#20833,0.5);
#18572=CYLINDRICAL_SURFACE('',#20838,0.5);
#18573=CYLINDRICAL_SURFACE('',#20839,0.5);
#18574=CYLINDRICAL_SURFACE('',#20848,44.);
#18575=CYLINDRICAL_SURFACE('',#20860,0.5);
#18576=CYLINDRICAL_SURFACE('',#20866,0.5);
#18577=CYLINDRICAL_SURFACE('',#20893,0.5);
#18578=CYLINDRICAL_SURFACE('',#20895,0.5);
#18579=CYLINDRICAL_SURFACE('',#20900,0.5);
#18580=CYLINDRICAL_SURFACE('',#20910,0.5);
#18581=CYLINDRICAL_SURFACE('',#20916,0.5);
#18582=CYLINDRICAL_SURFACE('',#20927,0.5);
#18583=CYLINDRICAL_SURFACE('',#20930,0.5);
#18584=CYLINDRICAL_SURFACE('',#20938,0.5);
#18585=CYLINDRICAL_SURFACE('',#20941,0.5);
#18586=CYLINDRICAL_SURFACE('',#20942,0.5);
#18587=CYLINDRICAL_SURFACE('',#20965,0.5);
#18588=CYLINDRICAL_SURFACE('',#20969,0.5);
#18589=CYLINDRICAL_SURFACE('',#20974,0.5);
#18590=CYLINDRICAL_SURFACE('',#20979,0.5);
#18591=CYLINDRICAL_SURFACE('',#20983,3.);
#18592=CYLINDRICAL_SURFACE('',#20988,1.25);
#18593=CYLINDRICAL_SURFACE('',#20995,0.5);
#18594=CYLINDRICAL_SURFACE('',#20998,0.5);
#18595=CYLINDRICAL_SURFACE('',#21000,0.5);
#18596=CYLINDRICAL_SURFACE('',#21005,0.499999999999997);
#18597=CYLINDRICAL_SURFACE('',#21009,0.499999999999999);
#18598=CYLINDRICAL_SURFACE('',#21012,0.5);
#18599=CYLINDRICAL_SURFACE('',#21018,0.5);
#18600=CYLINDRICAL_SURFACE('',#21028,1.25);
#18601=CYLINDRICAL_SURFACE('',#21031,0.5);
#18602=CYLINDRICAL_SURFACE('',#21036,0.5);
#18603=CYLINDRICAL_SURFACE('',#21040,0.5);
#18604=CYLINDRICAL_SURFACE('',#21046,0.5);
#18605=CYLINDRICAL_SURFACE('',#21049,0.5);
#18606=CYLINDRICAL_SURFACE('',#21051,0.5);
#18607=CYLINDRICAL_SURFACE('',#21056,0.5);
#18608=CYLINDRICAL_SURFACE('',#21064,44.);
#18609=CYLINDRICAL_SURFACE('',#21085,0.499999999999997);
#18610=CYLINDRICAL_SURFACE('',#21088,0.5);
#18611=CYLINDRICAL_SURFACE('',#21090,0.5);
#18612=CYLINDRICAL_SURFACE('',#21095,0.5);
#18613=CYLINDRICAL_SURFACE('',#21100,1.25);
#18614=CYLINDRICAL_SURFACE('',#21106,1.25);
#18615=CYLINDRICAL_SURFACE('',#21126,3.);
#18616=CYLINDRICAL_SURFACE('',#21132,3.);
#18617=CYLINDRICAL_SURFACE('',#21144,3.);
#18618=CYLINDRICAL_SURFACE('',#21154,3.);
#18619=CYLINDRICAL_SURFACE('',#21162,3.);
#18620=CYLINDRICAL_SURFACE('',#21170,3.);
#18621=CYLINDRICAL_SURFACE('',#21174,0.5);
#18622=CYLINDRICAL_SURFACE('',#21176,0.5);
#18623=CYLINDRICAL_SURFACE('',#21181,0.5);
#18624=CYLINDRICAL_SURFACE('',#21192,44.);
#18625=CYLINDRICAL_SURFACE('',#21216,7.05);
#18626=CYLINDRICAL_SURFACE('',#21232,12.);
#18627=CYLINDRICAL_SURFACE('',#21260,5.);
#18628=CYLINDRICAL_SURFACE('',#21265,5.);
#18629=CYLINDRICAL_SURFACE('',#21270,5.);
#18630=CYLINDRICAL_SURFACE('',#21281,3.);
#18631=CYLINDRICAL_SURFACE('',#21282,3.);
#18632=CYLINDRICAL_SURFACE('',#21283,3.);
#18633=CYLINDRICAL_SURFACE('',#21294,42.4);
#18634=CYLINDRICAL_SURFACE('',#21295,4.5);
#18635=CYLINDRICAL_SURFACE('',#21296,4.5);
#18636=CYLINDRICAL_SURFACE('',#21297,4.5);
#18637=CYLINDRICAL_SURFACE('',#21303,3.03);
#18638=CYLINDRICAL_SURFACE('',#21388,7.1875);
#18639=CYLINDRICAL_SURFACE('',#21392,10.);
#18640=CYLINDRICAL_SURFACE('',#21394,7.1875);
#18641=CYLINDRICAL_SURFACE('',#21472,10.);
#18642=CYLINDRICAL_SURFACE('',#21475,7.1875);
#18643=CYLINDRICAL_SURFACE('',#21478,10.);
#18644=CYLINDRICAL_SURFACE('',#21479,7.1875);
#18645=CYLINDRICAL_SURFACE('',#21480,10.);
#18646=CYLINDRICAL_SURFACE('',#21483,7.1875);
#18647=CYLINDRICAL_SURFACE('',#21486,10.);
#18648=CYLINDRICAL_SURFACE('',#21487,7.1875);
#18649=CYLINDRICAL_SURFACE('',#21488,10.);
#18650=CYLINDRICAL_SURFACE('',#21491,7.1875);
#18651=CYLINDRICAL_SURFACE('',#21494,10.);
#18652=CYLINDRICAL_SURFACE('',#21495,7.1875);
#18653=CYLINDRICAL_SURFACE('',#21496,10.);
#18654=CYLINDRICAL_SURFACE('',#21499,7.1875);
#18655=CYLINDRICAL_SURFACE('',#21502,10.);
#18656=CYLINDRICAL_SURFACE('',#21503,7.1875);
#18657=CYLINDRICAL_SURFACE('',#21504,10.);
#18658=CYLINDRICAL_SURFACE('',#21507,7.1875);
#18659=CYLINDRICAL_SURFACE('',#21510,10.);
#18660=CYLINDRICAL_SURFACE('',#21511,7.1875);
#18661=CYLINDRICAL_SURFACE('',#21512,10.);
#18662=CYLINDRICAL_SURFACE('',#21515,7.1875);
#18663=CYLINDRICAL_SURFACE('',#21518,10.);
#18664=CYLINDRICAL_SURFACE('',#21519,7.1875);
#18665=CYLINDRICAL_SURFACE('',#21520,14.0625);
#18666=CYLINDRICAL_SURFACE('',#21523,16.875);
#18667=CYLINDRICAL_SURFACE('',#21526,14.0625);
#18668=CYLINDRICAL_SURFACE('',#21529,16.875);
#18669=CYLINDRICAL_SURFACE('',#21532,14.0625);
#18670=CYLINDRICAL_SURFACE('',#21535,16.875);
#18671=CYLINDRICAL_SURFACE('',#21538,14.0625);
#18672=CYLINDRICAL_SURFACE('',#21541,16.875);
#18673=CYLINDRICAL_SURFACE('',#21544,14.0625);
#18674=CYLINDRICAL_SURFACE('',#21547,16.875);
#18675=CYLINDRICAL_SURFACE('',#21550,14.0625);
#18676=CYLINDRICAL_SURFACE('',#21553,16.875);
#18677=CYLINDRICAL_SURFACE('',#21556,14.0625);
#18678=CYLINDRICAL_SURFACE('',#21559,16.875);
#18679=CYLINDRICAL_SURFACE('',#21562,14.0625);
#18680=CYLINDRICAL_SURFACE('',#21565,16.875);
#18681=CYLINDRICAL_SURFACE('',#21568,14.0625);
#18682=CYLINDRICAL_SURFACE('',#21571,16.875);
#18683=CYLINDRICAL_SURFACE('',#21574,14.0625);
#18684=CYLINDRICAL_SURFACE('',#21577,16.875);
#18685=CYLINDRICAL_SURFACE('',#21580,14.0625);
#18686=CYLINDRICAL_SURFACE('',#21583,16.875);
#18687=CYLINDRICAL_SURFACE('',#21586,14.0625);
#18688=CYLINDRICAL_SURFACE('',#21589,16.875);
#18689=CYLINDRICAL_SURFACE('',#21592,14.0625);
#18690=CYLINDRICAL_SURFACE('',#21595,16.875);
#18691=CYLINDRICAL_SURFACE('',#21598,14.0625);
#18692=CYLINDRICAL_SURFACE('',#21601,16.875);
#18693=CYLINDRICAL_SURFACE('',#21604,14.0625);
#18694=CYLINDRICAL_SURFACE('',#21607,16.875);
#18695=CYLINDRICAL_SURFACE('',#21610,14.0625);
#18696=CYLINDRICAL_SURFACE('',#21613,16.875);
#18697=CYLINDRICAL_SURFACE('',#21616,14.0625);
#18698=CYLINDRICAL_SURFACE('',#21619,16.875);
#18699=CYLINDRICAL_SURFACE('',#21622,14.0625);
#18700=CYLINDRICAL_SURFACE('',#21625,16.875);
#18701=CYLINDRICAL_SURFACE('',#21628,14.0625);
#18702=CYLINDRICAL_SURFACE('',#21631,16.875);
#18703=CYLINDRICAL_SURFACE('',#21634,14.0625);
#18704=CYLINDRICAL_SURFACE('',#21637,16.875);
#18705=CYLINDRICAL_SURFACE('',#21640,14.0625);
#18706=CYLINDRICAL_SURFACE('',#21643,16.875);
#18707=CYLINDRICAL_SURFACE('',#21646,14.0625);
#18708=CYLINDRICAL_SURFACE('',#21649,16.875);
#18709=CYLINDRICAL_SURFACE('',#21652,14.0625);
#18710=CYLINDRICAL_SURFACE('',#21655,16.875);
#18711=CYLINDRICAL_SURFACE('',#21658,14.0625);
#18712=CYLINDRICAL_SURFACE('',#21661,16.875);
#18713=CYLINDRICAL_SURFACE('',#21664,14.0625);
#18714=CYLINDRICAL_SURFACE('',#21667,16.875);
#18715=CYLINDRICAL_SURFACE('',#21670,10.);
#18716=CYLINDRICAL_SURFACE('',#21687,3.);
#18717=CYLINDRICAL_SURFACE('',#21702,0.3);
#18718=CYLINDRICAL_SURFACE('',#21709,0.3);
#18719=CYLINDRICAL_SURFACE('',#21714,2.5);
#18720=CYLINDRICAL_SURFACE('',#21719,0.3);
#18721=CYLINDRICAL_SURFACE('',#21726,0.3);
#18722=CYLINDRICAL_SURFACE('',#21730,2.5);
#18723=CYLINDRICAL_SURFACE('',#21736,1.275);
#18724=CYLINDRICAL_SURFACE('',#21756,1.25);
#18725=CYLINDRICAL_SURFACE('',#21778,0.4);
#18726=CYLINDRICAL_SURFACE('',#21781,0.4);
#18727=CYLINDRICAL_SURFACE('',#21788,0.4);
#18728=CYLINDRICAL_SURFACE('',#21789,0.4);
#18729=CYLINDRICAL_SURFACE('',#21798,0.4);
#18730=CYLINDRICAL_SURFACE('',#21801,0.4);
#18731=CYLINDRICAL_SURFACE('',#21806,0.4);
#18732=CYLINDRICAL_SURFACE('',#21807,0.4);
#18733=CYLINDRICAL_SURFACE('',#21812,0.4);
#18734=CYLINDRICAL_SURFACE('',#21813,0.4);
#18735=CYLINDRICAL_SURFACE('',#21817,0.4);
#18736=CYLINDRICAL_SURFACE('',#21820,0.4);
#18737=CYLINDRICAL_SURFACE('',#21826,0.4);
#18738=CYLINDRICAL_SURFACE('',#21829,0.4);
#18739=CYLINDRICAL_SURFACE('',#21835,0.4);
#18740=CYLINDRICAL_SURFACE('',#21839,0.4);
#18741=CYLINDRICAL_SURFACE('',#21844,0.4);
#18742=CYLINDRICAL_SURFACE('',#21849,0.4);
#18743=CYLINDRICAL_SURFACE('',#21850,0.4);
#18744=CYLINDRICAL_SURFACE('',#21851,0.4);
#18745=CYLINDRICAL_SURFACE('',#21856,0.4);
#18746=CYLINDRICAL_SURFACE('',#21865,0.4);
#18747=CYLINDRICAL_SURFACE('',#21867,0.4);
#18748=CYLINDRICAL_SURFACE('',#21870,0.4);
#18749=CYLINDRICAL_SURFACE('',#21873,0.4);
#18750=CYLINDRICAL_SURFACE('',#21876,0.4);
#18751=CYLINDRICAL_SURFACE('',#21882,0.4);
#18752=CYLINDRICAL_SURFACE('',#21887,0.4);
#18753=CYLINDRICAL_SURFACE('',#21889,0.4);
#18754=CYLINDRICAL_SURFACE('',#21914,23.);
#18755=CYLINDRICAL_SURFACE('',#21922,0.4);
#18756=CYLINDRICAL_SURFACE('',#21924,0.4);
#18757=CYLINDRICAL_SURFACE('',#21928,0.4);
#18758=CYLINDRICAL_SURFACE('',#21931,0.4);
#18759=CYLINDRICAL_SURFACE('',#21934,0.4);
#18760=CYLINDRICAL_SURFACE('',#21945,0.4);
#18761=CYLINDRICAL_SURFACE('',#21948,0.4);
#18762=CYLINDRICAL_SURFACE('',#21962,21.8);
#18763=CYLINDRICAL_SURFACE('',#21971,0.4);
#18764=CYLINDRICAL_SURFACE('',#21976,0.4);
#18765=CYLINDRICAL_SURFACE('',#21979,0.4);
#18766=CYLINDRICAL_SURFACE('',#21984,0.4);
#18767=CYLINDRICAL_SURFACE('',#21988,0.4);
#18768=CYLINDRICAL_SURFACE('',#21989,0.4);
#18769=CYLINDRICAL_SURFACE('',#21994,7.05);
#18770=CYLINDRICAL_SURFACE('',#22002,10.4);
#18771=CYLINDRICAL_SURFACE('',#22047,9.);
#18772=CYLINDRICAL_SURFACE('',#22074,0.5);
#18773=CYLINDRICAL_SURFACE('',#22078,0.5);
#18774=CYLINDRICAL_SURFACE('',#22081,0.5);
#18775=CYLINDRICAL_SURFACE('',#22085,0.5);
#18776=CYLINDRICAL_SURFACE('',#22088,0.5);
#18777=CYLINDRICAL_SURFACE('',#22092,0.5);
#18778=CYLINDRICAL_SURFACE('',#22103,0.5);
#18779=CYLINDRICAL_SURFACE('',#22111,0.5);
#18780=CYLINDRICAL_SURFACE('',#22118,0.5);
#18781=CYLINDRICAL_SURFACE('',#22128,21.);
#18782=CYLINDRICAL_SURFACE('',#22139,0.5);
#18783=CYLINDRICAL_SURFACE('',#22180,0.5);
#18784=CYLINDRICAL_SURFACE('',#22182,0.5);
#18785=CYLINDRICAL_SURFACE('',#22184,0.5);
#18786=CYLINDRICAL_SURFACE('',#22196,0.5);
#18787=CYLINDRICAL_SURFACE('',#22198,0.5);
#18788=CYLINDRICAL_SURFACE('',#22204,0.5);
#18789=CYLINDRICAL_SURFACE('',#22211,0.5);
#18790=CYLINDRICAL_SURFACE('',#22215,0.5);
#18791=CYLINDRICAL_SURFACE('',#22230,0.5);
#18792=CYLINDRICAL_SURFACE('',#22235,0.5);
#18793=CYLINDRICAL_SURFACE('',#22236,18.5);
#18794=CYLINDRICAL_SURFACE('',#22247,0.5);
#18795=CYLINDRICAL_SURFACE('',#22251,0.5);
#18796=CYLINDRICAL_SURFACE('',#22255,0.5);
#18797=CYLINDRICAL_SURFACE('',#22262,0.5);
#18798=CYLINDRICAL_SURFACE('',#22268,0.5);
#18799=CYLINDRICAL_SURFACE('',#22269,0.5);
#18800=CYLINDRICAL_SURFACE('',#22273,0.5);
#18801=CYLINDRICAL_SURFACE('',#22280,0.5);
#18802=CYLINDRICAL_SURFACE('',#22288,0.5);
#18803=CYLINDRICAL_SURFACE('',#22290,0.5);
#18804=CYLINDRICAL_SURFACE('',#22295,0.5);
#18805=CYLINDRICAL_SURFACE('',#22297,0.5);
#18806=CYLINDRICAL_SURFACE('',#22311,0.5);
#18807=CYLINDRICAL_SURFACE('',#22313,0.5);
#18808=CYLINDRICAL_SURFACE('',#22315,0.5);
#18809=CYLINDRICAL_SURFACE('',#22317,0.5);
#18810=CYLINDRICAL_SURFACE('',#22326,0.5);
#18811=CYLINDRICAL_SURFACE('',#22327,18.5);
#18812=CYLINDRICAL_SURFACE('',#22351,0.5);
#18813=CYLINDRICAL_SURFACE('',#22356,18.5);
#18814=CYLINDRICAL_SURFACE('',#22357,0.5);
#18815=CYLINDRICAL_SURFACE('',#22362,0.5);
#18816=CYLINDRICAL_SURFACE('',#22367,0.5);
#18817=CYLINDRICAL_SURFACE('',#22369,0.5);
#18818=CYLINDRICAL_SURFACE('',#22370,0.5);
#18819=CYLINDRICAL_SURFACE('',#22371,0.5);
#18820=CYLINDRICAL_SURFACE('',#22377,18.5);
#18821=CYLINDRICAL_SURFACE('',#22378,18.5);
#18822=ADVANCED_FACE('',(#1126,#1082),#18310,.T.);
#18823=ADVANCED_FACE('',(#1127),#18311,.T.);
#18824=ADVANCED_FACE('',(#1128),#18312,.T.);
#18825=ADVANCED_FACE('',(#1129),#18313,.T.);
#18826=ADVANCED_FACE('',(#1130),#18314,.T.);
#18827=ADVANCED_FACE('',(#1131),#18315,.T.);
#18828=ADVANCED_FACE('',(#1132),#18316,.T.);
#18829=ADVANCED_FACE('',(#1133),#18317,.T.);
#18830=ADVANCED_FACE('',(#1134),#18318,.T.);
#18831=ADVANCED_FACE('',(#1135),#18319,.T.);
#18832=ADVANCED_FACE('',(#1136),#18320,.T.);
#18833=ADVANCED_FACE('',(#1137),#18321,.T.);
#18834=ADVANCED_FACE('',(#1138),#18322,.T.);
#18835=ADVANCED_FACE('',(#1139),#18323,.T.);
#18836=ADVANCED_FACE('',(#1140),#18324,.T.);
#18837=ADVANCED_FACE('',(#1141),#18325,.T.);
#18838=ADVANCED_FACE('',(#1142),#18326,.T.);
#18839=ADVANCED_FACE('',(#1143),#18327,.T.);
#18840=ADVANCED_FACE('',(#1144),#18328,.T.);
#18841=ADVANCED_FACE('',(#1145),#18329,.T.);
#18842=ADVANCED_FACE('',(#1146),#18330,.T.);
#18843=ADVANCED_FACE('',(#1147),#18331,.T.);
#18844=ADVANCED_FACE('',(#1148),#18332,.T.);
#18845=ADVANCED_FACE('',(#1149),#18333,.T.);
#18846=ADVANCED_FACE('',(#1150),#18334,.T.);
#18847=ADVANCED_FACE('',(#1151),#18335,.T.);
#18848=ADVANCED_FACE('',(#1152),#18336,.T.);
#18849=ADVANCED_FACE('',(#1153),#18337,.T.);
#18850=ADVANCED_FACE('',(#1154),#18338,.T.);
#18851=ADVANCED_FACE('',(#1155),#18339,.T.);
#18852=ADVANCED_FACE('',(#1156),#18340,.T.);
#18853=ADVANCED_FACE('',(#1157),#18341,.T.);
#18854=ADVANCED_FACE('',(#1158),#18342,.T.);
#18855=ADVANCED_FACE('',(#1159),#18343,.T.);
#18856=ADVANCED_FACE('',(#1160),#18344,.T.);
#18857=ADVANCED_FACE('',(#1161),#18345,.T.);
#18858=ADVANCED_FACE('',(#1162),#18346,.T.);
#18859=ADVANCED_FACE('',(#1163),#18347,.T.);
#18860=ADVANCED_FACE('',(#1164),#18348,.T.);
#18861=ADVANCED_FACE('',(#1165),#18349,.T.);
#18862=ADVANCED_FACE('',(#1166),#18350,.T.);
#18863=ADVANCED_FACE('',(#1167),#18351,.T.);
#18864=ADVANCED_FACE('',(#1168),#18352,.T.);
#18865=ADVANCED_FACE('',(#1169),#18353,.T.);
#18866=ADVANCED_FACE('',(#1170),#18354,.T.);
#18867=ADVANCED_FACE('',(#1171),#18355,.T.);
#18868=ADVANCED_FACE('',(#1172),#18356,.T.);
#18869=ADVANCED_FACE('',(#1173),#18357,.T.);
#18870=ADVANCED_FACE('',(#1174),#18358,.T.);
#18871=ADVANCED_FACE('',(#1175),#18359,.T.);
#18872=ADVANCED_FACE('',(#1176),#18360,.T.);
#18873=ADVANCED_FACE('',(#1177),#18361,.T.);
#18874=ADVANCED_FACE('',(#1178),#18362,.T.);
#18875=ADVANCED_FACE('',(#1179),#18363,.T.);
#18876=ADVANCED_FACE('',(#1180),#18364,.T.);
#18877=ADVANCED_FACE('',(#1181),#18365,.T.);
#18878=ADVANCED_FACE('',(#1182),#18366,.T.);
#18879=ADVANCED_FACE('',(#1183),#18367,.T.);
#18880=ADVANCED_FACE('',(#1184),#18368,.T.);
#18881=ADVANCED_FACE('',(#1185),#18369,.T.);
#18882=ADVANCED_FACE('',(#1186),#18370,.T.);
#18883=ADVANCED_FACE('',(#1187),#18371,.T.);
#18884=ADVANCED_FACE('',(#1188),#18372,.T.);
#18885=ADVANCED_FACE('',(#1189),#18373,.T.);
#18886=ADVANCED_FACE('',(#1190),#18374,.T.);
#18887=ADVANCED_FACE('',(#1191),#18375,.T.);
#18888=ADVANCED_FACE('',(#1192),#18376,.T.);
#18889=ADVANCED_FACE('',(#1193),#18377,.T.);
#18890=ADVANCED_FACE('',(#1194),#18378,.T.);
#18891=ADVANCED_FACE('',(#1195),#18379,.T.);
#18892=ADVANCED_FACE('',(#1196),#18380,.T.);
#18893=ADVANCED_FACE('',(#1197),#18381,.T.);
#18894=ADVANCED_FACE('',(#1198),#18382,.T.);
#18895=ADVANCED_FACE('',(#1199),#18383,.T.);
#18896=ADVANCED_FACE('',(#1200),#18384,.T.);
#18897=ADVANCED_FACE('',(#1201),#18385,.T.);
#18898=ADVANCED_FACE('',(#1202),#18386,.T.);
#18899=ADVANCED_FACE('',(#1203),#18387,.T.);
#18900=ADVANCED_FACE('',(#1204),#18388,.T.);
#18901=ADVANCED_FACE('',(#1205),#18389,.T.);
#18902=ADVANCED_FACE('',(#1206),#18390,.T.);
#18903=ADVANCED_FACE('',(#1207),#18391,.T.);
#18904=ADVANCED_FACE('',(#1208),#18392,.T.);
#18905=ADVANCED_FACE('',(#1209),#18393,.T.);
#18906=ADVANCED_FACE('',(#1210),#18394,.T.);
#18907=ADVANCED_FACE('',(#1211),#18395,.T.);
#18908=ADVANCED_FACE('',(#1212),#18396,.T.);
#18909=ADVANCED_FACE('',(#1213),#18397,.T.);
#18910=ADVANCED_FACE('',(#1214),#18398,.T.);
#18911=ADVANCED_FACE('',(#1215),#18399,.T.);
#18912=ADVANCED_FACE('',(#1216),#18400,.T.);
#18913=ADVANCED_FACE('',(#1217),#18401,.T.);
#18914=ADVANCED_FACE('',(#1218),#18402,.T.);
#18915=ADVANCED_FACE('',(#1219),#18403,.T.);
#18916=ADVANCED_FACE('',(#1220),#18404,.T.);
#18917=ADVANCED_FACE('',(#1221),#18405,.T.);
#18918=ADVANCED_FACE('',(#1222),#18406,.T.);
#18919=ADVANCED_FACE('',(#1223),#18407,.T.);
#18920=ADVANCED_FACE('',(#1224),#18408,.T.);
#18921=ADVANCED_FACE('',(#1225),#18409,.T.);
#18922=ADVANCED_FACE('',(#1226),#18410,.T.);
#18923=ADVANCED_FACE('',(#1227),#18411,.T.);
#18924=ADVANCED_FACE('',(#1228),#18412,.T.);
#18925=ADVANCED_FACE('',(#1229),#18413,.T.);
#18926=ADVANCED_FACE('',(#1230),#18414,.T.);
#18927=ADVANCED_FACE('',(#1231),#18415,.T.);
#18928=ADVANCED_FACE('',(#1232),#18416,.T.);
#18929=ADVANCED_FACE('',(#1233),#18417,.T.);
#18930=ADVANCED_FACE('',(#1234),#18418,.T.);
#18931=ADVANCED_FACE('',(#1235),#18419,.T.);
#18932=ADVANCED_FACE('',(#1236),#18420,.T.);
#18933=ADVANCED_FACE('',(#1237),#18421,.T.);
#18934=ADVANCED_FACE('',(#1238),#18422,.T.);
#18935=ADVANCED_FACE('',(#1239),#18423,.T.);
#18936=ADVANCED_FACE('',(#1240),#18424,.T.);
#18937=ADVANCED_FACE('',(#1241),#18425,.T.);
#18938=ADVANCED_FACE('',(#1242),#18426,.T.);
#18939=ADVANCED_FACE('',(#1243),#18427,.T.);
#18940=ADVANCED_FACE('',(#1244),#18428,.T.);
#18941=ADVANCED_FACE('',(#1245),#18429,.T.);
#18942=ADVANCED_FACE('',(#1246),#18430,.T.);
#18943=ADVANCED_FACE('',(#1247),#18431,.T.);
#18944=ADVANCED_FACE('',(#1248),#18432,.T.);
#18945=ADVANCED_FACE('',(#1249),#18433,.T.);
#18946=ADVANCED_FACE('',(#1250),#18434,.T.);
#18947=ADVANCED_FACE('',(#1251),#18435,.T.);
#18948=ADVANCED_FACE('',(#1252),#18436,.T.);
#18949=ADVANCED_FACE('',(#1253),#18437,.T.);
#18950=ADVANCED_FACE('',(#1254),#18438,.T.);
#18951=ADVANCED_FACE('',(#1255),#18439,.T.);
#18952=ADVANCED_FACE('',(#1256),#18440,.T.);
#18953=ADVANCED_FACE('',(#1257),#18441,.T.);
#18954=ADVANCED_FACE('',(#1258),#18442,.T.);
#18955=ADVANCED_FACE('',(#1259),#18443,.T.);
#18956=ADVANCED_FACE('',(#1260),#18444,.T.);
#18957=ADVANCED_FACE('',(#1261),#18445,.T.);
#18958=ADVANCED_FACE('',(#1262),#18446,.T.);
#18959=ADVANCED_FACE('',(#1263),#18447,.T.);
#18960=ADVANCED_FACE('',(#1264),#18448,.T.);
#18961=ADVANCED_FACE('',(#1265),#18449,.T.);
#18962=ADVANCED_FACE('',(#1266),#18450,.T.);
#18963=ADVANCED_FACE('',(#1267),#18451,.T.);
#18964=ADVANCED_FACE('',(#1268),#18452,.T.);
#18965=ADVANCED_FACE('',(#1269),#18453,.T.);
#18966=ADVANCED_FACE('',(#1270),#18454,.T.);
#18967=ADVANCED_FACE('',(#1271),#18455,.T.);
#18968=ADVANCED_FACE('',(#1272),#18456,.T.);
#18969=ADVANCED_FACE('',(#1273),#18457,.T.);
#18970=ADVANCED_FACE('',(#1274),#18458,.T.);
#18971=ADVANCED_FACE('',(#1275),#18459,.T.);
#18972=ADVANCED_FACE('',(#1276),#18460,.T.);
#18973=ADVANCED_FACE('',(#1277),#18461,.T.);
#18974=ADVANCED_FACE('',(#1278),#18462,.T.);
#18975=ADVANCED_FACE('',(#1279),#18463,.T.);
#18976=ADVANCED_FACE('',(#1280),#18464,.T.);
#18977=ADVANCED_FACE('',(#1281),#18465,.T.);
#18978=ADVANCED_FACE('',(#1282),#18466,.T.);
#18979=ADVANCED_FACE('',(#1283),#853,.F.);
#18980=ADVANCED_FACE('',(#1284),#854,.F.);
#18981=ADVANCED_FACE('',(#1285),#855,.F.);
#18982=ADVANCED_FACE('',(#1286),#856,.F.);
#18983=ADVANCED_FACE('',(#1287),#857,.F.);
#18984=ADVANCED_FACE('',(#1288),#834,.F.);
#18985=ADVANCED_FACE('',(#1289),#858,.T.);
#18986=ADVANCED_FACE('',(#1290),#18467,.T.);
#18987=ADVANCED_FACE('',(#1291),#835,.F.);
#18988=ADVANCED_FACE('',(#1292),#859,.F.);
#18989=ADVANCED_FACE('',(#1293),#836,.F.);
#18990=ADVANCED_FACE('',(#1294),#860,.T.);
#18991=ADVANCED_FACE('',(#1295),#18468,.T.);
#18992=ADVANCED_FACE('',(#1296),#837,.F.);
#18993=ADVANCED_FACE('',(#1297),#18469,.T.);
#18994=ADVANCED_FACE('',(#1298),#861,.T.);
#18995=ADVANCED_FACE('',(#1299),#500,.F.);
#18996=ADVANCED_FACE('',(#1300),#18470,.T.);
#18997=ADVANCED_FACE('',(#1301),#501,.F.);
#18998=ADVANCED_FACE('',(#1302),#862,.F.);
#18999=ADVANCED_FACE('',(#1303),#380,.T.);
#19000=ADVANCED_FACE('',(#1304),#381,.T.);
#19001=ADVANCED_FACE('',(#1305),#18471,.T.);
#19002=ADVANCED_FACE('',(#1306),#382,.T.);
#19003=ADVANCED_FACE('',(#1307),#863,.T.);
#19004=ADVANCED_FACE('',(#1308),#502,.F.);
#19005=ADVANCED_FACE('',(#1309),#18472,.T.);
#19006=ADVANCED_FACE('',(#1310),#503,.F.);
#19007=ADVANCED_FACE('',(#1311),#864,.F.);
#19008=ADVANCED_FACE('',(#1312),#383,.T.);
#19009=ADVANCED_FACE('',(#1313),#18473,.T.);
#19010=ADVANCED_FACE('',(#1314),#384,.T.);
#19011=ADVANCED_FACE('',(#1315),#865,.T.);
#19012=ADVANCED_FACE('',(#1316),#504,.F.);
#19013=ADVANCED_FACE('',(#1317),#18474,.T.);
#19014=ADVANCED_FACE('',(#1318),#505,.F.);
#19015=ADVANCED_FACE('',(#1319),#866,.F.);
#19016=ADVANCED_FACE('',(#1320),#385,.T.);
#19017=ADVANCED_FACE('',(#1321),#18475,.T.);
#19018=ADVANCED_FACE('',(#1322),#386,.T.);
#19019=ADVANCED_FACE('',(#1323),#867,.T.);
#19020=ADVANCED_FACE('',(#1324),#506,.F.);
#19021=ADVANCED_FACE('',(#1325),#18476,.T.);
#19022=ADVANCED_FACE('',(#1326),#507,.F.);
#19023=ADVANCED_FACE('',(#1327),#868,.F.);
#19024=ADVANCED_FACE('',(#1328),#387,.T.);
#19025=ADVANCED_FACE('',(#1329),#18477,.T.);
#19026=ADVANCED_FACE('',(#1330),#388,.T.);
#19027=ADVANCED_FACE('',(#1331),#869,.T.);
#19028=ADVANCED_FACE('',(#1332),#508,.F.);
#19029=ADVANCED_FACE('',(#1333),#18478,.T.);
#19030=ADVANCED_FACE('',(#1334),#509,.F.);
#19031=ADVANCED_FACE('',(#1335),#870,.F.);
#19032=ADVANCED_FACE('',(#1336),#389,.T.);
#19033=ADVANCED_FACE('',(#1337),#18479,.T.);
#19034=ADVANCED_FACE('',(#1338),#390,.T.);
#19035=ADVANCED_FACE('',(#1339),#871,.T.);
#19036=ADVANCED_FACE('',(#1340),#510,.F.);
#19037=ADVANCED_FACE('',(#1341),#18480,.T.);
#19038=ADVANCED_FACE('',(#1342),#511,.F.);
#19039=ADVANCED_FACE('',(#1343),#872,.F.);
#19040=ADVANCED_FACE('',(#1344),#391,.T.);
#19041=ADVANCED_FACE('',(#1345),#18481,.T.);
#19042=ADVANCED_FACE('',(#1346),#392,.T.);
#19043=ADVANCED_FACE('',(#1347),#873,.T.);
#19044=ADVANCED_FACE('',(#1348),#512,.F.);
#19045=ADVANCED_FACE('',(#1349),#18482,.T.);
#19046=ADVANCED_FACE('',(#1350),#513,.F.);
#19047=ADVANCED_FACE('',(#1351),#874,.F.);
#19048=ADVANCED_FACE('',(#1352),#393,.T.);
#19049=ADVANCED_FACE('',(#1353),#18483,.T.);
#19050=ADVANCED_FACE('',(#1354),#394,.T.);
#19051=ADVANCED_FACE('',(#1355),#875,.T.);
#19052=ADVANCED_FACE('',(#1356),#514,.F.);
#19053=ADVANCED_FACE('',(#1357),#18484,.T.);
#19054=ADVANCED_FACE('',(#1358),#515,.F.);
#19055=ADVANCED_FACE('',(#1359),#876,.F.);
#19056=ADVANCED_FACE('',(#1360),#395,.T.);
#19057=ADVANCED_FACE('',(#1361),#18485,.T.);
#19058=ADVANCED_FACE('',(#1362),#396,.T.);
#19059=ADVANCED_FACE('',(#1363),#877,.T.);
#19060=ADVANCED_FACE('',(#1364),#516,.F.);
#19061=ADVANCED_FACE('',(#1365),#18486,.T.);
#19062=ADVANCED_FACE('',(#1366),#517,.F.);
#19063=ADVANCED_FACE('',(#1367),#878,.F.);
#19064=ADVANCED_FACE('',(#1368),#397,.T.);
#19065=ADVANCED_FACE('',(#1369),#18487,.T.);
#19066=ADVANCED_FACE('',(#1370),#398,.T.);
#19067=ADVANCED_FACE('',(#1371),#879,.T.);
#19068=ADVANCED_FACE('',(#1372),#518,.F.);
#19069=ADVANCED_FACE('',(#1373),#18488,.T.);
#19070=ADVANCED_FACE('',(#1374),#519,.F.);
#19071=ADVANCED_FACE('',(#1375),#880,.F.);
#19072=ADVANCED_FACE('',(#1376),#399,.T.);
#19073=ADVANCED_FACE('',(#1377),#18489,.T.);
#19074=ADVANCED_FACE('',(#1378),#400,.T.);
#19075=ADVANCED_FACE('',(#1379),#881,.T.);
#19076=ADVANCED_FACE('',(#1380),#520,.F.);
#19077=ADVANCED_FACE('',(#1381),#18490,.T.);
#19078=ADVANCED_FACE('',(#1382),#521,.F.);
#19079=ADVANCED_FACE('',(#1383),#882,.F.);
#19080=ADVANCED_FACE('',(#1384),#401,.T.);
#19081=ADVANCED_FACE('',(#1385),#18491,.T.);
#19082=ADVANCED_FACE('',(#1386),#402,.T.);
#19083=ADVANCED_FACE('',(#1387),#883,.T.);
#19084=ADVANCED_FACE('',(#1388),#522,.F.);
#19085=ADVANCED_FACE('',(#1389),#18492,.T.);
#19086=ADVANCED_FACE('',(#1390),#523,.F.);
#19087=ADVANCED_FACE('',(#1391),#884,.F.);
#19088=ADVANCED_FACE('',(#1392),#403,.T.);
#19089=ADVANCED_FACE('',(#1393),#18493,.T.);
#19090=ADVANCED_FACE('',(#1394),#404,.T.);
#19091=ADVANCED_FACE('',(#1395),#885,.T.);
#19092=ADVANCED_FACE('',(#1396),#524,.F.);
#19093=ADVANCED_FACE('',(#1397),#18494,.T.);
#19094=ADVANCED_FACE('',(#1398),#525,.F.);
#19095=ADVANCED_FACE('',(#1399),#886,.F.);
#19096=ADVANCED_FACE('',(#1400),#405,.T.);
#19097=ADVANCED_FACE('',(#1401),#18495,.T.);
#19098=ADVANCED_FACE('',(#1402),#406,.T.);
#19099=ADVANCED_FACE('',(#1403),#887,.T.);
#19100=ADVANCED_FACE('',(#1404),#526,.F.);
#19101=ADVANCED_FACE('',(#1405),#18496,.T.);
#19102=ADVANCED_FACE('',(#1406),#527,.F.);
#19103=ADVANCED_FACE('',(#1407),#888,.F.);
#19104=ADVANCED_FACE('',(#1408),#407,.T.);
#19105=ADVANCED_FACE('',(#1409),#18497,.T.);
#19106=ADVANCED_FACE('',(#1410),#408,.T.);
#19107=ADVANCED_FACE('',(#1411),#528,.F.);
#19108=ADVANCED_FACE('',(#1412),#889,.T.);
#19109=ADVANCED_FACE('',(#1413),#18498,.T.);
#19110=ADVANCED_FACE('',(#1414),#529,.F.);
#19111=ADVANCED_FACE('',(#1415),#890,.F.);
#19112=ADVANCED_FACE('',(#1416),#409,.T.);
#19113=ADVANCED_FACE('',(#1417),#18499,.T.);
#19114=ADVANCED_FACE('',(#1418),#891,.T.);
#19115=ADVANCED_FACE('',(#1419),#410,.T.);
#19116=ADVANCED_FACE('',(#1420),#411,.T.);
#19117=ADVANCED_FACE('',(#1421),#412,.T.);
#19118=ADVANCED_FACE('',(#1422),#18500,.T.);
#19119=ADVANCED_FACE('',(#1423),#413,.T.);
#19120=ADVANCED_FACE('',(#1424),#892,.T.);
#19121=ADVANCED_FACE('',(#1425),#18501,.T.);
#19122=ADVANCED_FACE('',(#1426),#243,.T.);
#19123=ADVANCED_FACE('',(#1427),#18502,.T.);
#19124=ADVANCED_FACE('',(#1428),#18503,.T.);
#19125=ADVANCED_FACE('',(#1429),#244,.T.);
#19126=ADVANCED_FACE('',(#1430),#245,.T.);
#19127=ADVANCED_FACE('',(#1431),#18504,.T.);
#19128=ADVANCED_FACE('',(#1432),#18505,.T.);
#19129=ADVANCED_FACE('',(#1433),#246,.T.);
#19130=ADVANCED_FACE('',(#1434),#18506,.T.);
#19131=ADVANCED_FACE('',(#1435),#893,.T.);
#19132=ADVANCED_FACE('',(#1436),#18507,.T.);
#19133=ADVANCED_FACE('',(#1437),#894,.T.);
#19134=ADVANCED_FACE('',(#1438),#18508,.T.);
#19135=ADVANCED_FACE('',(#1439),#895,.T.);
#19136=ADVANCED_FACE('',(#1440),#18509,.T.);
#19137=ADVANCED_FACE('',(#1441),#18510,.T.);
#19138=ADVANCED_FACE('',(#1442),#247,.T.);
#19139=ADVANCED_FACE('',(#1443),#896,.T.);
#19140=ADVANCED_FACE('',(#1444),#18511,.T.);
#19141=ADVANCED_FACE('',(#1445),#897,.T.);
#19142=ADVANCED_FACE('',(#1446),#18512,.T.);
#19143=ADVANCED_FACE('',(#1447),#248,.T.);
#19144=ADVANCED_FACE('',(#1448),#898,.T.);
#19145=ADVANCED_FACE('',(#1449),#18513,.T.);
#19146=ADVANCED_FACE('',(#1450),#249,.T.);
#19147=ADVANCED_FACE('',(#1451),#18514,.T.);
#19148=ADVANCED_FACE('',(#1452),#899,.T.);
#19149=ADVANCED_FACE('',(#1453),#250,.T.);
#19150=ADVANCED_FACE('',(#1454),#18515,.T.);
#19151=ADVANCED_FACE('',(#1455),#18516,.T.);
#19152=ADVANCED_FACE('',(#1456),#18517,.T.);
#19153=ADVANCED_FACE('',(#1457),#18518,.T.);
#19154=ADVANCED_FACE('',(#1458),#18519,.T.);
#19155=ADVANCED_FACE('',(#1459),#251,.T.);
#19156=ADVANCED_FACE('',(#1460),#900,.T.);
#19157=ADVANCED_FACE('',(#1461),#18520,.T.);
#19158=ADVANCED_FACE('',(#1462),#901,.T.);
#19159=ADVANCED_FACE('',(#1463),#252,.T.);
#19160=ADVANCED_FACE('',(#1464),#18521,.T.);
#19161=ADVANCED_FACE('',(#1465),#902,.T.);
#19162=ADVANCED_FACE('',(#1466),#18522,.T.);
#19163=ADVANCED_FACE('',(#1467),#18523,.T.);
#19164=ADVANCED_FACE('',(#1468),#253,.T.);
#19165=ADVANCED_FACE('',(#1469),#18524,.T.);
#19166=ADVANCED_FACE('',(#1470),#903,.T.);
#19167=ADVANCED_FACE('',(#1471),#904,.T.);
#19168=ADVANCED_FACE('',(#1472),#18525,.T.);
#19169=ADVANCED_FACE('',(#1473),#254,.T.);
#19170=ADVANCED_FACE('',(#1474),#18526,.T.);
#19171=ADVANCED_FACE('',(#1475),#905,.T.);
#19172=ADVANCED_FACE('',(#1476),#18527,.T.);
#19173=ADVANCED_FACE('',(#1477),#18528,.T.);
#19174=ADVANCED_FACE('',(#1478),#255,.T.);
#19175=ADVANCED_FACE('',(#1479),#906,.T.);
#19176=ADVANCED_FACE('',(#1480),#907,.T.);
#19177=ADVANCED_FACE('',(#1481),#18529,.T.);
#19178=ADVANCED_FACE('',(#1482),#256,.T.);
#19179=ADVANCED_FACE('',(#1483),#18530,.T.);
#19180=ADVANCED_FACE('',(#1484),#257,.T.);
#19181=ADVANCED_FACE('',(#1485),#18531,.T.);
#19182=ADVANCED_FACE('',(#1486),#258,.T.);
#19183=ADVANCED_FACE('',(#1487),#18532,.T.);
#19184=ADVANCED_FACE('',(#1488),#908,.T.);
#19185=ADVANCED_FACE('',(#1489),#18533,.T.);
#19186=ADVANCED_FACE('',(#1490),#909,.T.);
#19187=ADVANCED_FACE('',(#1491),#18534,.T.);
#19188=ADVANCED_FACE('',(#1492),#910,.T.);
#19189=ADVANCED_FACE('',(#1493),#18535,.T.);
#19190=ADVANCED_FACE('',(#1494),#18536,.T.);
#19191=ADVANCED_FACE('',(#1495),#18537,.T.);
#19192=ADVANCED_FACE('',(#1496),#259,.T.);
#19193=ADVANCED_FACE('',(#1497),#911,.T.);
#19194=ADVANCED_FACE('',(#1498),#18538,.T.);
#19195=ADVANCED_FACE('',(#1499),#912,.T.);
#19196=ADVANCED_FACE('',(#1500),#260,.T.);
#19197=ADVANCED_FACE('',(#1501),#913,.T.);
#19198=ADVANCED_FACE('',(#1502),#18539,.T.);
#19199=ADVANCED_FACE('',(#1503),#18540,.T.);
#19200=ADVANCED_FACE('',(#1504),#18541,.T.);
#19201=ADVANCED_FACE('',(#1505),#18542,.T.);
#19202=ADVANCED_FACE('',(#1506),#261,.T.);
#19203=ADVANCED_FACE('',(#1507),#18543,.T.);
#19204=ADVANCED_FACE('',(#1508),#262,.T.);
#19205=ADVANCED_FACE('',(#1509),#914,.T.);
#19206=ADVANCED_FACE('',(#1510),#915,.T.);
#19207=ADVANCED_FACE('',(#1511),#18544,.T.);
#19208=ADVANCED_FACE('',(#1512),#18545,.T.);
#19209=ADVANCED_FACE('',(#1513),#263,.T.);
#19210=ADVANCED_FACE('',(#1514),#18546,.T.);
#19211=ADVANCED_FACE('',(#1515),#916,.T.);
#19212=ADVANCED_FACE('',(#1516),#264,.T.);
#19213=ADVANCED_FACE('',(#1517),#18547,.T.);
#19214=ADVANCED_FACE('',(#1518),#18548,.T.);
#19215=ADVANCED_FACE('',(#1519),#18549,.T.);
#19216=ADVANCED_FACE('',(#1520),#265,.T.);
#19217=ADVANCED_FACE('',(#1521),#917,.T.);
#19218=ADVANCED_FACE('',(#1522),#18550,.T.);
#19219=ADVANCED_FACE('',(#1523),#918,.T.);
#19220=ADVANCED_FACE('',(#1524),#18551,.T.);
#19221=ADVANCED_FACE('',(#1525),#18552,.T.);
#19222=ADVANCED_FACE('',(#1526),#18553,.T.);
#19223=ADVANCED_FACE('',(#1527),#266,.T.);
#19224=ADVANCED_FACE('',(#1528),#267,.T.);
#19225=ADVANCED_FACE('',(#1529),#18554,.T.);
#19226=ADVANCED_FACE('',(#1530),#18555,.T.);
#19227=ADVANCED_FACE('',(#1531),#18556,.T.);
#19228=ADVANCED_FACE('',(#1532),#919,.T.);
#19229=ADVANCED_FACE('',(#1533),#18557,.T.);
#19230=ADVANCED_FACE('',(#1534),#18558,.T.);
#19231=ADVANCED_FACE('',(#1535),#268,.T.);
#19232=ADVANCED_FACE('',(#1536),#269,.T.);
#19233=ADVANCED_FACE('',(#1537),#18559,.T.);
#19234=ADVANCED_FACE('',(#1538),#18560,.T.);
#19235=ADVANCED_FACE('',(#1539),#920,.T.);
#19236=ADVANCED_FACE('',(#1540),#18561,.T.);
#19237=ADVANCED_FACE('',(#1541),#921,.T.);
#19238=ADVANCED_FACE('',(#1542),#18562,.T.);
#19239=ADVANCED_FACE('',(#1543),#18563,.T.);
#19240=ADVANCED_FACE('',(#1544),#922,.T.);
#19241=ADVANCED_FACE('',(#1545),#18564,.T.);
#19242=ADVANCED_FACE('',(#1546),#923,.T.);
#19243=ADVANCED_FACE('',(#1547),#18565,.T.);
#19244=ADVANCED_FACE('',(#1548),#270,.T.);
#19245=ADVANCED_FACE('',(#1549),#18566,.T.);
#19246=ADVANCED_FACE('',(#1550),#924,.T.);
#19247=ADVANCED_FACE('',(#1551),#925,.T.);
#19248=ADVANCED_FACE('',(#1552),#926,.T.);
#19249=ADVANCED_FACE('',(#1553),#18567,.T.);
#19250=ADVANCED_FACE('',(#1554),#927,.T.);
#19251=ADVANCED_FACE('',(#1555),#18568,.T.);
#19252=ADVANCED_FACE('',(#1556),#271,.T.);
#19253=ADVANCED_FACE('',(#1557),#18569,.T.);
#19254=ADVANCED_FACE('',(#1558),#272,.T.);
#19255=ADVANCED_FACE('',(#1559),#18570,.T.);
#19256=ADVANCED_FACE('',(#1560),#928,.T.);
#19257=ADVANCED_FACE('',(#1561),#18571,.T.);
#19258=ADVANCED_FACE('',(#1562),#273,.T.);
#19259=ADVANCED_FACE('',(#1563),#18572,.T.);
#19260=ADVANCED_FACE('',(#1564),#18573,.T.);
#19261=ADVANCED_FACE('',(#1565),#274,.T.);
#19262=ADVANCED_FACE('',(#1566),#929,.T.);
#19263=ADVANCED_FACE('',(#1567),#95,.T.);
#19264=ADVANCED_FACE('',(#1568),#18574,.T.);
#19265=ADVANCED_FACE('',(#1569,#1083),#930,.F.);
#19266=ADVANCED_FACE('',(#1570),#18575,.T.);
#19267=ADVANCED_FACE('',(#1571),#96,.T.);
#19268=ADVANCED_FACE('',(#1572),#18576,.T.);
#19269=ADVANCED_FACE('',(#1573),#275,.T.);
#19270=ADVANCED_FACE('',(#1574),#276,.T.);
#19271=ADVANCED_FACE('',(#1575),#838,.F.);
#19272=ADVANCED_FACE('',(#1576,#1084),#931,.T.);
#19273=ADVANCED_FACE('',(#1577),#97,.T.);
#19274=ADVANCED_FACE('',(#1578),#414,.T.);
#19275=ADVANCED_FACE('',(#1579),#98,.T.);
#19276=ADVANCED_FACE('',(#1580),#18577,.T.);
#19277=ADVANCED_FACE('',(#1581),#18578,.T.);
#19278=ADVANCED_FACE('',(#1582),#99,.T.);
#19279=ADVANCED_FACE('',(#1583),#18579,.T.);
#19280=ADVANCED_FACE('',(#1584),#100,.T.);
#19281=ADVANCED_FACE('',(#1585),#101,.T.);
#19282=ADVANCED_FACE('',(#1586),#932,.F.);
#19283=ADVANCED_FACE('',(#1587),#415,.T.);
#19284=ADVANCED_FACE('',(#1588),#18580,.T.);
#19285=ADVANCED_FACE('',(#1589),#839,.F.);
#19286=ADVANCED_FACE('',(#1590),#277,.T.);
#19287=ADVANCED_FACE('',(#1591),#18581,.T.);
#19288=ADVANCED_FACE('',(#1592),#278,.T.);
#19289=ADVANCED_FACE('',(#1593),#933,.F.);
#19290=ADVANCED_FACE('',(#1594),#416,.T.);
#19291=ADVANCED_FACE('',(#1595),#102,.T.);
#19292=ADVANCED_FACE('',(#1596),#18582,.T.);
#19293=ADVANCED_FACE('',(#1597),#934,.F.);
#19294=ADVANCED_FACE('',(#1598),#103,.T.);
#19295=ADVANCED_FACE('',(#1599),#18583,.T.);
#19296=ADVANCED_FACE('',(#1600),#935,.F.);
#19297=ADVANCED_FACE('',(#1601),#840,.F.);
#19298=ADVANCED_FACE('',(#1602),#279,.T.);
#19299=ADVANCED_FACE('',(#1603),#280,.T.);
#19300=ADVANCED_FACE('',(#1604),#18584,.T.);
#19301=ADVANCED_FACE('',(#1605),#936,.F.);
#19302=ADVANCED_FACE('',(#1606),#18585,.T.);
#19303=ADVANCED_FACE('',(#1607),#18586,.T.);
#19304=ADVANCED_FACE('',(#1608),#841,.F.);
#19305=ADVANCED_FACE('',(#1609),#281,.T.);
#19306=ADVANCED_FACE('',(#1610),#282,.T.);
#19307=ADVANCED_FACE('',(#1611),#104,.T.);
#19308=ADVANCED_FACE('',(#1612),#417,.T.);
#19309=ADVANCED_FACE('',(#1613),#105,.T.);
#19310=ADVANCED_FACE('',(#1614,#1085),#937,.F.);
#19311=ADVANCED_FACE('',(#1615),#283,.T.);
#19312=ADVANCED_FACE('',(#1616),#842,.F.);
#19313=ADVANCED_FACE('',(#1617),#18587,.T.);
#19314=ADVANCED_FACE('',(#1618),#106,.T.);
#19315=ADVANCED_FACE('',(#1619),#18588,.T.);
#19316=ADVANCED_FACE('',(#1620),#107,.T.);
#19317=ADVANCED_FACE('',(#1621),#18589,.T.);
#19318=ADVANCED_FACE('',(#1622),#284,.T.);
#19319=ADVANCED_FACE('',(#1623),#938,.F.);
#19320=ADVANCED_FACE('',(#1624),#939,.F.);
#19321=ADVANCED_FACE('',(#1625),#18590,.T.);
#19322=ADVANCED_FACE('',(#1626),#108,.T.);
#19323=ADVANCED_FACE('',(#1627),#18591,.F.);
#19324=ADVANCED_FACE('',(#1628),#109,.T.);
#19325=ADVANCED_FACE('',(#1629),#18592,.F.);
#19326=ADVANCED_FACE('',(#1630),#285,.T.);
#19327=ADVANCED_FACE('',(#1631),#18593,.T.);
#19328=ADVANCED_FACE('',(#1632),#940,.T.);
#19329=ADVANCED_FACE('',(#1633),#18594,.T.);
#19330=ADVANCED_FACE('',(#1634),#18595,.T.);
#19331=ADVANCED_FACE('',(#1635),#18596,.T.);
#19332=ADVANCED_FACE('',(#1636),#941,.T.);
#19333=ADVANCED_FACE('',(#1637),#18597,.T.);
#19334=ADVANCED_FACE('',(#1638),#18598,.T.);
#19335=ADVANCED_FACE('',(#1639),#942,.T.);
#19336=ADVANCED_FACE('',(#1640),#943,.T.);
#19337=ADVANCED_FACE('',(#1641),#18599,.T.);
#19338=ADVANCED_FACE('',(#1642),#110,.T.);
#19339=ADVANCED_FACE('',(#1643,#1086),#944,.F.);
#19340=ADVANCED_FACE('',(#1644),#111,.T.);
#19341=ADVANCED_FACE('',(#1645),#18600,.F.);
#19342=ADVANCED_FACE('',(#1646),#18601,.T.);
#19343=ADVANCED_FACE('',(#1647),#286,.T.);
#19344=ADVANCED_FACE('',(#1648),#18602,.T.);
#19345=ADVANCED_FACE('',(#1649),#287,.T.);
#19346=ADVANCED_FACE('',(#1650),#18603,.T.);
#19347=ADVANCED_FACE('',(#1651),#288,.T.);
#19348=ADVANCED_FACE('',(#1652),#18604,.T.);
#19349=ADVANCED_FACE('',(#1653),#945,.T.);
#19350=ADVANCED_FACE('',(#1654),#18605,.T.);
#19351=ADVANCED_FACE('',(#1655),#18606,.T.);
#19352=ADVANCED_FACE('',(#1656),#289,.T.);
#19353=ADVANCED_FACE('',(#1657),#946,.T.);
#19354=ADVANCED_FACE('',(#1658),#18607,.T.);
#19355=ADVANCED_FACE('',(#1659),#947,.T.);
#19356=ADVANCED_FACE('',(#1660),#112,.T.);
#19357=ADVANCED_FACE('',(#1661),#18608,.T.);
#19358=ADVANCED_FACE('',(#1662,#1087),#948,.F.);
#19359=ADVANCED_FACE('',(#1663),#113,.T.);
#19360=ADVANCED_FACE('',(#1664),#418,.T.);
#19361=ADVANCED_FACE('',(#1665),#114,.T.);
#19362=ADVANCED_FACE('',(#1666,#1088),#949,.F.);
#19363=ADVANCED_FACE('',(#1667),#115,.T.);
#19364=ADVANCED_FACE('',(#1668,#1089),#950,.F.);
#19365=ADVANCED_FACE('',(#1669),#18609,.T.);
#19366=ADVANCED_FACE('',(#1670),#18610,.T.);
#19367=ADVANCED_FACE('',(#1671),#951,.T.);
#19368=ADVANCED_FACE('',(#1672),#18611,.T.);
#19369=ADVANCED_FACE('',(#1673),#290,.T.);
#19370=ADVANCED_FACE('',(#1674),#952,.T.);
#19371=ADVANCED_FACE('',(#1675),#18612,.T.);
#19372=ADVANCED_FACE('',(#1676),#116,.T.);
#19373=ADVANCED_FACE('',(#1677),#18613,.F.);
#19374=ADVANCED_FACE('',(#1678),#117,.T.);
#19375=ADVANCED_FACE('',(#1679),#18614,.F.);
#19376=ADVANCED_FACE('',(#1680),#118,.T.);
#19377=ADVANCED_FACE('',(#1681,#1090,#1091,#1092,#1093,#1094,#1095,#1096,
#1097,#1098,#1099,#1100),#953,.T.);
#19378=ADVANCED_FACE('',(#1682),#18615,.F.);
#19379=ADVANCED_FACE('',(#1683),#119,.T.);
#19380=ADVANCED_FACE('',(#1684),#18616,.F.);
#19381=ADVANCED_FACE('',(#1685),#120,.T.);
#19382=ADVANCED_FACE('',(#1686),#121,.T.);
#19383=ADVANCED_FACE('',(#1687),#122,.T.);
#19384=ADVANCED_FACE('',(#1688),#123,.T.);
#19385=ADVANCED_FACE('',(#1689),#18617,.F.);
#19386=ADVANCED_FACE('',(#1690),#124,.T.);
#19387=ADVANCED_FACE('',(#1691),#125,.T.);
#19388=ADVANCED_FACE('',(#1692),#126,.T.);
#19389=ADVANCED_FACE('',(#1693),#18618,.F.);
#19390=ADVANCED_FACE('',(#1694,#1101),#954,.T.);
#19391=ADVANCED_FACE('',(#1695),#127,.T.);
#19392=ADVANCED_FACE('',(#1696),#18619,.F.);
#19393=ADVANCED_FACE('',(#1697,#1102),#955,.T.);
#19394=ADVANCED_FACE('',(#1698),#128,.T.);
#19395=ADVANCED_FACE('',(#1699),#18620,.F.);
#19396=ADVANCED_FACE('',(#1700,#1103),#956,.T.);
#19397=ADVANCED_FACE('',(#1701),#18621,.T.);
#19398=ADVANCED_FACE('',(#1702),#18622,.T.);
#19399=ADVANCED_FACE('',(#1703),#291,.T.);
#19400=ADVANCED_FACE('',(#1704),#957,.T.);
#19401=ADVANCED_FACE('',(#1705),#18623,.T.);
#19402=ADVANCED_FACE('',(#1706),#129,.T.);
#19403=ADVANCED_FACE('',(#1707),#419,.T.);
#19404=ADVANCED_FACE('',(#1708),#18624,.T.);
#19405=ADVANCED_FACE('',(#1709),#130,.T.);
#19406=ADVANCED_FACE('',(#1710,#1104,#1105,#1106,#1107,#1108,#1109,#1110),
#958,.T.);
#19407=ADVANCED_FACE('',(#1711),#131,.T.);
#19408=ADVANCED_FACE('',(#1712),#132,.T.);
#19409=ADVANCED_FACE('',(#1713),#133,.T.);
#19410=ADVANCED_FACE('',(#1714),#134,.T.);
#19411=ADVANCED_FACE('',(#1715),#18625,.F.);
#19412=ADVANCED_FACE('',(#1716),#135,.T.);
#19413=ADVANCED_FACE('',(#1717),#420,.F.);
#19414=ADVANCED_FACE('',(#1718),#136,.T.);
#19415=ADVANCED_FACE('',(#1719),#137,.T.);
#19416=ADVANCED_FACE('',(#1720),#18626,.F.);
#19417=ADVANCED_FACE('',(#1721),#138,.T.);
#19418=ADVANCED_FACE('',(#1722),#421,.T.);
#19419=ADVANCED_FACE('',(#1723),#139,.T.);
#19420=ADVANCED_FACE('',(#1724),#140,.T.);
#19421=ADVANCED_FACE('',(#1725,#1111,#1112,#1113,#1114),#959,.T.);
#19422=ADVANCED_FACE('',(#1726),#18627,.F.);
#19423=ADVANCED_FACE('',(#1727),#141,.T.);
#19424=ADVANCED_FACE('',(#1728),#18628,.F.);
#19425=ADVANCED_FACE('',(#1729),#142,.T.);
#19426=ADVANCED_FACE('',(#1730),#18629,.F.);
#19427=ADVANCED_FACE('',(#1731),#143,.T.);
#19428=ADVANCED_FACE('',(#1732),#422,.F.);
#19429=ADVANCED_FACE('',(#1733),#144,.T.);
#19430=ADVANCED_FACE('',(#1734),#960,.F.);
#19431=ADVANCED_FACE('',(#1735),#18630,.F.);
#19432=ADVANCED_FACE('',(#1736),#18631,.F.);
#19433=ADVANCED_FACE('',(#1737),#18632,.F.);
#19434=ADVANCED_FACE('',(#1738),#961,.T.);
#19435=ADVANCED_FACE('',(#1739),#962,.T.);
#19436=ADVANCED_FACE('',(#1740),#963,.T.);
#19437=ADVANCED_FACE('',(#1741),#964,.T.);
#19438=ADVANCED_FACE('',(#1742),#965,.T.);
#19439=ADVANCED_FACE('',(#1743),#966,.T.);
#19440=ADVANCED_FACE('',(#1744),#967,.T.);
#19441=ADVANCED_FACE('',(#1745),#968,.T.);
#19442=ADVANCED_FACE('',(#1746),#969,.T.);
#19443=ADVANCED_FACE('',(#1747),#970,.T.);
#19444=ADVANCED_FACE('',(#1748),#18633,.T.);
#19445=ADVANCED_FACE('',(#1749),#18634,.T.);
#19446=ADVANCED_FACE('',(#1750),#18635,.T.);
#19447=ADVANCED_FACE('',(#1751),#18636,.T.);
#19448=ADVANCED_FACE('',(#1752),#423,.F.);
#19449=ADVANCED_FACE('',(#1753),#18637,.F.);
#19450=ADVANCED_FACE('',(#1754,#1115),#971,.T.);
#19451=ADVANCED_FACE('',(#1755),#424,.F.);
#19452=ADVANCED_FACE('',(#1756,#1116),#972,.T.);
#19453=ADVANCED_FACE('',(#1757),#530,.F.);
#19454=ADVANCED_FACE('',(#1758),#18638,.T.);
#19455=ADVANCED_FACE('',(#1759),#531,.F.);
#19456=ADVANCED_FACE('',(#1760),#425,.T.);
#19457=ADVANCED_FACE('',(#1761),#18639,.T.);
#19458=ADVANCED_FACE('',(#1762),#532,.F.);
#19459=ADVANCED_FACE('',(#1763),#18640,.T.);
#19460=ADVANCED_FACE('',(#1764),#533,.F.);
#19461=ADVANCED_FACE('',(#1765,#1117),#973,.T.);
#19462=ADVANCED_FACE('',(#1766),#18641,.T.);
#19463=ADVANCED_FACE('',(#1767),#426,.T.);
#19464=ADVANCED_FACE('',(#1768),#534,.F.);
#19465=ADVANCED_FACE('',(#1769),#18642,.T.);
#19466=ADVANCED_FACE('',(#1770),#535,.F.);
#19467=ADVANCED_FACE('',(#1771),#427,.T.);
#19468=ADVANCED_FACE('',(#1772),#18643,.T.);
#19469=ADVANCED_FACE('',(#1773),#536,.F.);
#19470=ADVANCED_FACE('',(#1774),#18644,.T.);
#19471=ADVANCED_FACE('',(#1775),#537,.F.);
#19472=ADVANCED_FACE('',(#1776),#18645,.T.);
#19473=ADVANCED_FACE('',(#1777),#428,.T.);
#19474=ADVANCED_FACE('',(#1778),#538,.F.);
#19475=ADVANCED_FACE('',(#1779),#18646,.T.);
#19476=ADVANCED_FACE('',(#1780),#539,.F.);
#19477=ADVANCED_FACE('',(#1781),#429,.T.);
#19478=ADVANCED_FACE('',(#1782),#18647,.T.);
#19479=ADVANCED_FACE('',(#1783),#540,.F.);
#19480=ADVANCED_FACE('',(#1784),#18648,.T.);
#19481=ADVANCED_FACE('',(#1785),#541,.F.);
#19482=ADVANCED_FACE('',(#1786),#18649,.T.);
#19483=ADVANCED_FACE('',(#1787),#430,.T.);
#19484=ADVANCED_FACE('',(#1788),#542,.F.);
#19485=ADVANCED_FACE('',(#1789),#18650,.T.);
#19486=ADVANCED_FACE('',(#1790),#543,.F.);
#19487=ADVANCED_FACE('',(#1791),#431,.T.);
#19488=ADVANCED_FACE('',(#1792),#18651,.T.);
#19489=ADVANCED_FACE('',(#1793),#544,.F.);
#19490=ADVANCED_FACE('',(#1794),#18652,.T.);
#19491=ADVANCED_FACE('',(#1795),#545,.F.);
#19492=ADVANCED_FACE('',(#1796),#18653,.T.);
#19493=ADVANCED_FACE('',(#1797),#432,.T.);
#19494=ADVANCED_FACE('',(#1798),#546,.F.);
#19495=ADVANCED_FACE('',(#1799),#18654,.T.);
#19496=ADVANCED_FACE('',(#1800),#547,.F.);
#19497=ADVANCED_FACE('',(#1801),#433,.T.);
#19498=ADVANCED_FACE('',(#1802),#18655,.T.);
#19499=ADVANCED_FACE('',(#1803),#548,.F.);
#19500=ADVANCED_FACE('',(#1804),#18656,.T.);
#19501=ADVANCED_FACE('',(#1805),#549,.F.);
#19502=ADVANCED_FACE('',(#1806),#18657,.T.);
#19503=ADVANCED_FACE('',(#1807),#434,.T.);
#19504=ADVANCED_FACE('',(#1808),#550,.F.);
#19505=ADVANCED_FACE('',(#1809),#18658,.T.);
#19506=ADVANCED_FACE('',(#1810),#551,.F.);
#19507=ADVANCED_FACE('',(#1811),#435,.T.);
#19508=ADVANCED_FACE('',(#1812),#18659,.T.);
#19509=ADVANCED_FACE('',(#1813),#552,.F.);
#19510=ADVANCED_FACE('',(#1814),#18660,.T.);
#19511=ADVANCED_FACE('',(#1815),#553,.F.);
#19512=ADVANCED_FACE('',(#1816),#18661,.T.);
#19513=ADVANCED_FACE('',(#1817),#436,.T.);
#19514=ADVANCED_FACE('',(#1818),#554,.F.);
#19515=ADVANCED_FACE('',(#1819),#18662,.T.);
#19516=ADVANCED_FACE('',(#1820),#555,.F.);
#19517=ADVANCED_FACE('',(#1821),#437,.T.);
#19518=ADVANCED_FACE('',(#1822),#18663,.T.);
#19519=ADVANCED_FACE('',(#1823),#556,.F.);
#19520=ADVANCED_FACE('',(#1824),#18664,.T.);
#19521=ADVANCED_FACE('',(#1825),#557,.F.);
#19522=ADVANCED_FACE('',(#1826),#558,.F.);
#19523=ADVANCED_FACE('',(#1827),#18665,.T.);
#19524=ADVANCED_FACE('',(#1828),#559,.F.);
#19525=ADVANCED_FACE('',(#1829),#438,.T.);
#19526=ADVANCED_FACE('',(#1830),#18666,.T.);
#19527=ADVANCED_FACE('',(#1831),#439,.T.);
#19528=ADVANCED_FACE('',(#1832),#560,.F.);
#19529=ADVANCED_FACE('',(#1833),#18667,.T.);
#19530=ADVANCED_FACE('',(#1834),#561,.F.);
#19531=ADVANCED_FACE('',(#1835),#440,.T.);
#19532=ADVANCED_FACE('',(#1836),#18668,.T.);
#19533=ADVANCED_FACE('',(#1837),#441,.T.);
#19534=ADVANCED_FACE('',(#1838),#562,.F.);
#19535=ADVANCED_FACE('',(#1839),#18669,.T.);
#19536=ADVANCED_FACE('',(#1840),#563,.F.);
#19537=ADVANCED_FACE('',(#1841),#442,.T.);
#19538=ADVANCED_FACE('',(#1842),#18670,.T.);
#19539=ADVANCED_FACE('',(#1843),#443,.T.);
#19540=ADVANCED_FACE('',(#1844),#564,.F.);
#19541=ADVANCED_FACE('',(#1845),#18671,.T.);
#19542=ADVANCED_FACE('',(#1846),#565,.F.);
#19543=ADVANCED_FACE('',(#1847),#444,.T.);
#19544=ADVANCED_FACE('',(#1848),#18672,.T.);
#19545=ADVANCED_FACE('',(#1849),#445,.T.);
#19546=ADVANCED_FACE('',(#1850),#566,.F.);
#19547=ADVANCED_FACE('',(#1851),#18673,.T.);
#19548=ADVANCED_FACE('',(#1852),#567,.F.);
#19549=ADVANCED_FACE('',(#1853),#446,.T.);
#19550=ADVANCED_FACE('',(#1854),#18674,.T.);
#19551=ADVANCED_FACE('',(#1855),#447,.T.);
#19552=ADVANCED_FACE('',(#1856),#568,.F.);
#19553=ADVANCED_FACE('',(#1857),#18675,.T.);
#19554=ADVANCED_FACE('',(#1858),#569,.F.);
#19555=ADVANCED_FACE('',(#1859),#448,.T.);
#19556=ADVANCED_FACE('',(#1860),#18676,.T.);
#19557=ADVANCED_FACE('',(#1861),#449,.T.);
#19558=ADVANCED_FACE('',(#1862),#570,.F.);
#19559=ADVANCED_FACE('',(#1863),#18677,.T.);
#19560=ADVANCED_FACE('',(#1864),#571,.F.);
#19561=ADVANCED_FACE('',(#1865),#450,.T.);
#19562=ADVANCED_FACE('',(#1866),#18678,.T.);
#19563=ADVANCED_FACE('',(#1867),#451,.T.);
#19564=ADVANCED_FACE('',(#1868),#572,.F.);
#19565=ADVANCED_FACE('',(#1869),#18679,.T.);
#19566=ADVANCED_FACE('',(#1870),#573,.F.);
#19567=ADVANCED_FACE('',(#1871),#452,.T.);
#19568=ADVANCED_FACE('',(#1872),#18680,.T.);
#19569=ADVANCED_FACE('',(#1873),#453,.T.);
#19570=ADVANCED_FACE('',(#1874),#574,.F.);
#19571=ADVANCED_FACE('',(#1875),#18681,.T.);
#19572=ADVANCED_FACE('',(#1876),#575,.F.);
#19573=ADVANCED_FACE('',(#1877),#454,.T.);
#19574=ADVANCED_FACE('',(#1878),#18682,.T.);
#19575=ADVANCED_FACE('',(#1879),#455,.T.);
#19576=ADVANCED_FACE('',(#1880),#576,.F.);
#19577=ADVANCED_FACE('',(#1881),#18683,.T.);
#19578=ADVANCED_FACE('',(#1882),#577,.F.);
#19579=ADVANCED_FACE('',(#1883),#456,.T.);
#19580=ADVANCED_FACE('',(#1884),#18684,.T.);
#19581=ADVANCED_FACE('',(#1885),#457,.T.);
#19582=ADVANCED_FACE('',(#1886),#578,.F.);
#19583=ADVANCED_FACE('',(#1887),#18685,.T.);
#19584=ADVANCED_FACE('',(#1888),#579,.F.);
#19585=ADVANCED_FACE('',(#1889),#458,.T.);
#19586=ADVANCED_FACE('',(#1890),#18686,.T.);
#19587=ADVANCED_FACE('',(#1891),#459,.T.);
#19588=ADVANCED_FACE('',(#1892),#580,.F.);
#19589=ADVANCED_FACE('',(#1893),#18687,.T.);
#19590=ADVANCED_FACE('',(#1894),#581,.F.);
#19591=ADVANCED_FACE('',(#1895),#460,.T.);
#19592=ADVANCED_FACE('',(#1896),#18688,.T.);
#19593=ADVANCED_FACE('',(#1897),#461,.T.);
#19594=ADVANCED_FACE('',(#1898),#582,.F.);
#19595=ADVANCED_FACE('',(#1899),#18689,.T.);
#19596=ADVANCED_FACE('',(#1900),#583,.F.);
#19597=ADVANCED_FACE('',(#1901),#462,.T.);
#19598=ADVANCED_FACE('',(#1902),#18690,.T.);
#19599=ADVANCED_FACE('',(#1903),#463,.T.);
#19600=ADVANCED_FACE('',(#1904),#584,.F.);
#19601=ADVANCED_FACE('',(#1905),#18691,.T.);
#19602=ADVANCED_FACE('',(#1906),#585,.F.);
#19603=ADVANCED_FACE('',(#1907),#464,.T.);
#19604=ADVANCED_FACE('',(#1908),#18692,.T.);
#19605=ADVANCED_FACE('',(#1909),#465,.T.);
#19606=ADVANCED_FACE('',(#1910),#586,.F.);
#19607=ADVANCED_FACE('',(#1911),#18693,.T.);
#19608=ADVANCED_FACE('',(#1912),#587,.F.);
#19609=ADVANCED_FACE('',(#1913),#466,.T.);
#19610=ADVANCED_FACE('',(#1914),#18694,.T.);
#19611=ADVANCED_FACE('',(#1915),#467,.T.);
#19612=ADVANCED_FACE('',(#1916),#588,.F.);
#19613=ADVANCED_FACE('',(#1917),#18695,.T.);
#19614=ADVANCED_FACE('',(#1918),#589,.F.);
#19615=ADVANCED_FACE('',(#1919),#468,.T.);
#19616=ADVANCED_FACE('',(#1920),#18696,.T.);
#19617=ADVANCED_FACE('',(#1921),#469,.T.);
#19618=ADVANCED_FACE('',(#1922),#590,.F.);
#19619=ADVANCED_FACE('',(#1923),#18697,.T.);
#19620=ADVANCED_FACE('',(#1924),#591,.F.);
#19621=ADVANCED_FACE('',(#1925),#470,.T.);
#19622=ADVANCED_FACE('',(#1926),#18698,.T.);
#19623=ADVANCED_FACE('',(#1927),#471,.T.);
#19624=ADVANCED_FACE('',(#1928),#592,.F.);
#19625=ADVANCED_FACE('',(#1929),#18699,.T.);
#19626=ADVANCED_FACE('',(#1930),#593,.F.);
#19627=ADVANCED_FACE('',(#1931),#472,.T.);
#19628=ADVANCED_FACE('',(#1932),#18700,.T.);
#19629=ADVANCED_FACE('',(#1933),#473,.T.);
#19630=ADVANCED_FACE('',(#1934),#594,.F.);
#19631=ADVANCED_FACE('',(#1935),#18701,.T.);
#19632=ADVANCED_FACE('',(#1936),#595,.F.);
#19633=ADVANCED_FACE('',(#1937),#474,.T.);
#19634=ADVANCED_FACE('',(#1938),#18702,.T.);
#19635=ADVANCED_FACE('',(#1939),#475,.T.);
#19636=ADVANCED_FACE('',(#1940),#596,.F.);
#19637=ADVANCED_FACE('',(#1941),#18703,.T.);
#19638=ADVANCED_FACE('',(#1942),#597,.F.);
#19639=ADVANCED_FACE('',(#1943),#476,.T.);
#19640=ADVANCED_FACE('',(#1944),#18704,.T.);
#19641=ADVANCED_FACE('',(#1945),#477,.T.);
#19642=ADVANCED_FACE('',(#1946),#598,.F.);
#19643=ADVANCED_FACE('',(#1947),#18705,.T.);
#19644=ADVANCED_FACE('',(#1948),#599,.F.);
#19645=ADVANCED_FACE('',(#1949),#478,.T.);
#19646=ADVANCED_FACE('',(#1950),#18706,.T.);
#19647=ADVANCED_FACE('',(#1951),#479,.T.);
#19648=ADVANCED_FACE('',(#1952),#600,.F.);
#19649=ADVANCED_FACE('',(#1953),#18707,.T.);
#19650=ADVANCED_FACE('',(#1954),#601,.F.);
#19651=ADVANCED_FACE('',(#1955),#480,.T.);
#19652=ADVANCED_FACE('',(#1956),#18708,.T.);
#19653=ADVANCED_FACE('',(#1957),#481,.T.);
#19654=ADVANCED_FACE('',(#1958),#602,.F.);
#19655=ADVANCED_FACE('',(#1959),#18709,.T.);
#19656=ADVANCED_FACE('',(#1960),#603,.F.);
#19657=ADVANCED_FACE('',(#1961),#482,.T.);
#19658=ADVANCED_FACE('',(#1962),#18710,.T.);
#19659=ADVANCED_FACE('',(#1963),#483,.T.);
#19660=ADVANCED_FACE('',(#1964),#604,.F.);
#19661=ADVANCED_FACE('',(#1965),#18711,.T.);
#19662=ADVANCED_FACE('',(#1966),#605,.F.);
#19663=ADVANCED_FACE('',(#1967),#484,.T.);
#19664=ADVANCED_FACE('',(#1968),#18712,.T.);
#19665=ADVANCED_FACE('',(#1969),#485,.T.);
#19666=ADVANCED_FACE('',(#1970),#606,.F.);
#19667=ADVANCED_FACE('',(#1971),#18713,.T.);
#19668=ADVANCED_FACE('',(#1972),#607,.F.);
#19669=ADVANCED_FACE('',(#1973),#486,.T.);
#19670=ADVANCED_FACE('',(#1974),#18714,.T.);
#19671=ADVANCED_FACE('',(#1975),#487,.T.);
#19672=ADVANCED_FACE('',(#1976),#18715,.T.);
#19673=ADVANCED_FACE('',(#1977),#488,.T.);
#19674=ADVANCED_FACE('',(#1978),#145,.T.);
#19675=ADVANCED_FACE('',(#1979),#489,.T.);
#19676=ADVANCED_FACE('',(#1980),#974,.T.);
#19677=ADVANCED_FACE('',(#1981),#146,.T.);
#19678=ADVANCED_FACE('',(#1982),#18716,.T.);
#19679=ADVANCED_FACE('',(#1983),#147,.T.);
#19680=ADVANCED_FACE('',(#1984),#490,.T.);
#19681=ADVANCED_FACE('',(#1985),#148,.T.);
#19682=ADVANCED_FACE('',(#1986),#975,.T.);
#19683=ADVANCED_FACE('',(#1987),#18717,.T.);
#19684=ADVANCED_FACE('',(#1988),#149,.T.);
#19685=ADVANCED_FACE('',(#1989),#18718,.T.);
#19686=ADVANCED_FACE('',(#1990),#150,.T.);
#19687=ADVANCED_FACE('',(#1991),#18719,.T.);
#19688=ADVANCED_FACE('',(#1992),#976,.T.);
#19689=ADVANCED_FACE('',(#1993,#1118),#977,.T.);
#19690=ADVANCED_FACE('',(#1994),#18720,.T.);
#19691=ADVANCED_FACE('',(#1995),#151,.T.);
#19692=ADVANCED_FACE('',(#1996),#18721,.T.);
#19693=ADVANCED_FACE('',(#1997),#152,.T.);
#19694=ADVANCED_FACE('',(#1998),#18722,.T.);
#19695=ADVANCED_FACE('',(#1999,#1119),#978,.F.);
#19696=ADVANCED_FACE('',(#2000),#153,.T.);
#19697=ADVANCED_FACE('',(#2001),#18723,.F.);
#19698=ADVANCED_FACE('',(#2002),#154,.T.);
#19699=ADVANCED_FACE('',(#2003),#979,.T.);
#19700=ADVANCED_FACE('',(#2004),#155,.T.);
#19701=ADVANCED_FACE('',(#2005),#491,.T.);
#19702=ADVANCED_FACE('',(#2006),#980,.T.);
#19703=ADVANCED_FACE('',(#2007),#156,.T.);
#19704=ADVANCED_FACE('',(#2008),#18724,.T.);
#19705=ADVANCED_FACE('',(#2009),#157,.T.);
#19706=ADVANCED_FACE('',(#2010),#492,.T.);
#19707=ADVANCED_FACE('',(#2011),#158,.T.);
#19708=ADVANCED_FACE('',(#2012),#981,.T.);
#19709=ADVANCED_FACE('',(#2013),#159,.T.);
#19710=ADVANCED_FACE('',(#2014),#982,.T.);
#19711=ADVANCED_FACE('',(#2015),#983,.F.);
#19712=ADVANCED_FACE('',(#2016),#18725,.T.);
#19713=ADVANCED_FACE('',(#2017),#18726,.T.);
#19714=ADVANCED_FACE('',(#2018),#292,.T.);
#19715=ADVANCED_FACE('',(#2019),#18727,.T.);
#19716=ADVANCED_FACE('',(#2020),#18728,.T.);
#19717=ADVANCED_FACE('',(#2021),#293,.T.);
#19718=ADVANCED_FACE('',(#2022),#294,.T.);
#19719=ADVANCED_FACE('',(#2023),#18729,.T.);
#19720=ADVANCED_FACE('',(#2024),#295,.T.);
#19721=ADVANCED_FACE('',(#2025),#18730,.T.);
#19722=ADVANCED_FACE('',(#2026),#984,.T.);
#19723=ADVANCED_FACE('',(#2027),#985,.T.);
#19724=ADVANCED_FACE('',(#2028),#18731,.T.);
#19725=ADVANCED_FACE('',(#2029),#18732,.T.);
#19726=ADVANCED_FACE('',(#2030),#296,.T.);
#19727=ADVANCED_FACE('',(#2031),#18733,.T.);
#19728=ADVANCED_FACE('',(#2032),#18734,.T.);
#19729=ADVANCED_FACE('',(#2033),#986,.T.);
#19730=ADVANCED_FACE('',(#2034),#987,.F.);
#19731=ADVANCED_FACE('',(#2035),#18735,.T.);
#19732=ADVANCED_FACE('',(#2036),#18736,.T.);
#19733=ADVANCED_FACE('',(#2037),#297,.T.);
#19734=ADVANCED_FACE('',(#2038),#18737,.T.);
#19735=ADVANCED_FACE('',(#2039),#18738,.T.);
#19736=ADVANCED_FACE('',(#2040),#298,.T.);
#19737=ADVANCED_FACE('',(#2041),#299,.T.);
#19738=ADVANCED_FACE('',(#2042),#18739,.T.);
#19739=ADVANCED_FACE('',(#2043),#988,.T.);
#19740=ADVANCED_FACE('',(#2044),#18740,.T.);
#19741=ADVANCED_FACE('',(#2045),#300,.T.);
#19742=ADVANCED_FACE('',(#2046),#18741,.T.);
#19743=ADVANCED_FACE('',(#2047),#301,.T.);
#19744=ADVANCED_FACE('',(#2048),#18742,.T.);
#19745=ADVANCED_FACE('',(#2049),#18743,.T.);
#19746=ADVANCED_FACE('',(#2050),#18744,.T.);
#19747=ADVANCED_FACE('',(#2051),#989,.T.);
#19748=ADVANCED_FACE('',(#2052),#990,.F.);
#19749=ADVANCED_FACE('',(#2053),#18745,.T.);
#19750=ADVANCED_FACE('',(#2054),#302,.T.);
#19751=ADVANCED_FACE('',(#2055),#303,.T.);
#19752=ADVANCED_FACE('',(#2056),#18746,.T.);
#19753=ADVANCED_FACE('',(#2057),#18747,.T.);
#19754=ADVANCED_FACE('',(#2058),#991,.T.);
#19755=ADVANCED_FACE('',(#2059),#18748,.T.);
#19756=ADVANCED_FACE('',(#2060),#18749,.T.);
#19757=ADVANCED_FACE('',(#2061),#18750,.T.);
#19758=ADVANCED_FACE('',(#2062),#304,.T.);
#19759=ADVANCED_FACE('',(#2063),#305,.T.);
#19760=ADVANCED_FACE('',(#2064),#18751,.T.);
#19761=ADVANCED_FACE('',(#2065),#992,.T.);
#19762=ADVANCED_FACE('',(#2066),#993,.T.);
#19763=ADVANCED_FACE('',(#2067),#18752,.T.);
#19764=ADVANCED_FACE('',(#2068),#994,.T.);
#19765=ADVANCED_FACE('',(#2069),#18753,.T.);
#19766=ADVANCED_FACE('',(#2070),#160,.T.);
#19767=ADVANCED_FACE('',(#2071,#1120),#995,.T.);
#19768=ADVANCED_FACE('',(#2072),#493,.T.);
#19769=ADVANCED_FACE('',(#2073),#161,.T.);
#19770=ADVANCED_FACE('',(#2074),#18754,.T.);
#19771=ADVANCED_FACE('',(#2075,#1121),#996,.T.);
#19772=ADVANCED_FACE('',(#2076),#306,.T.);
#19773=ADVANCED_FACE('',(#2077),#18755,.T.);
#19774=ADVANCED_FACE('',(#2078),#18756,.T.);
#19775=ADVANCED_FACE('',(#2079),#307,.T.);
#19776=ADVANCED_FACE('',(#2080),#997,.F.);
#19777=ADVANCED_FACE('',(#2081),#998,.T.);
#19778=ADVANCED_FACE('',(#2082),#18757,.T.);
#19779=ADVANCED_FACE('',(#2083),#18758,.T.);
#19780=ADVANCED_FACE('',(#2084),#18759,.T.);
#19781=ADVANCED_FACE('',(#2085),#308,.T.);
#19782=ADVANCED_FACE('',(#2086),#309,.T.);
#19783=ADVANCED_FACE('',(#2087),#310,.T.);
#19784=ADVANCED_FACE('',(#2088),#999,.F.);
#19785=ADVANCED_FACE('',(#2089),#18760,.T.);
#19786=ADVANCED_FACE('',(#2090),#1000,.T.);
#19787=ADVANCED_FACE('',(#2091),#18761,.T.);
#19788=ADVANCED_FACE('',(#2092),#1001,.T.);
#19789=ADVANCED_FACE('',(#2093),#162,.T.);
#19790=ADVANCED_FACE('',(#2094),#494,.T.);
#19791=ADVANCED_FACE('',(#2095),#163,.T.);
#19792=ADVANCED_FACE('',(#2096),#18762,.T.);
#19793=ADVANCED_FACE('',(#2097),#164,.T.);
#19794=ADVANCED_FACE('',(#2098),#165,.T.);
#19795=ADVANCED_FACE('',(#2099,#1122),#1002,.T.);
#19796=ADVANCED_FACE('',(#2100),#18763,.T.);
#19797=ADVANCED_FACE('',(#2101),#311,.T.);
#19798=ADVANCED_FACE('',(#2102),#18764,.T.);
#19799=ADVANCED_FACE('',(#2103),#1003,.T.);
#19800=ADVANCED_FACE('',(#2104),#18765,.T.);
#19801=ADVANCED_FACE('',(#2105),#1004,.T.);
#19802=ADVANCED_FACE('',(#2106),#312,.T.);
#19803=ADVANCED_FACE('',(#2107),#18766,.T.);
#19804=ADVANCED_FACE('',(#2108),#313,.T.);
#19805=ADVANCED_FACE('',(#2109),#18767,.T.);
#19806=ADVANCED_FACE('',(#2110),#18768,.T.);
#19807=ADVANCED_FACE('',(#2111),#166,.T.);
#19808=ADVANCED_FACE('',(#2112),#18769,.F.);
#19809=ADVANCED_FACE('',(#2113),#167,.T.);
#19810=ADVANCED_FACE('',(#2114,#1123),#1005,.F.);
#19811=ADVANCED_FACE('',(#2115),#18770,.F.);
#19812=ADVANCED_FACE('',(#2116),#1006,.T.);
#19813=ADVANCED_FACE('',(#2117),#1007,.T.);
#19814=ADVANCED_FACE('',(#2118),#1008,.T.);
#19815=ADVANCED_FACE('',(#2119),#1009,.T.);
#19816=ADVANCED_FACE('',(#2120),#1010,.T.);
#19817=ADVANCED_FACE('',(#2121),#1011,.T.);
#19818=ADVANCED_FACE('',(#2122),#1012,.T.);
#19819=ADVANCED_FACE('',(#2123),#1013,.T.);
#19820=ADVANCED_FACE('',(#2124),#1014,.T.);
#19821=ADVANCED_FACE('',(#2125),#1015,.T.);
#19822=ADVANCED_FACE('',(#2126),#1016,.T.);
#19823=ADVANCED_FACE('',(#2127),#1017,.T.);
#19824=ADVANCED_FACE('',(#2128),#1018,.T.);
#19825=ADVANCED_FACE('',(#2129),#1019,.T.);
#19826=ADVANCED_FACE('',(#2130),#1020,.T.);
#19827=ADVANCED_FACE('',(#2131),#1021,.T.);
#19828=ADVANCED_FACE('',(#2132),#1022,.T.);
#19829=ADVANCED_FACE('',(#2133),#1023,.T.);
#19830=ADVANCED_FACE('',(#2134),#1024,.T.);
#19831=ADVANCED_FACE('',(#2135),#1025,.T.);
#19832=ADVANCED_FACE('',(#2136),#1026,.T.);
#19833=ADVANCED_FACE('',(#2137),#1027,.T.);
#19834=ADVANCED_FACE('',(#2138),#1028,.T.);
#19835=ADVANCED_FACE('',(#2139),#1029,.T.);
#19836=ADVANCED_FACE('',(#2140),#1030,.T.);
#19837=ADVANCED_FACE('',(#2141),#1031,.T.);
#19838=ADVANCED_FACE('',(#2142),#1032,.T.);
#19839=ADVANCED_FACE('',(#2143),#1033,.T.);
#19840=ADVANCED_FACE('',(#2144),#1034,.T.);
#19841=ADVANCED_FACE('',(#2145),#1035,.T.);
#19842=ADVANCED_FACE('',(#2146),#1036,.T.);
#19843=ADVANCED_FACE('',(#2147),#1037,.T.);
#19844=ADVANCED_FACE('',(#2148),#843,.T.);
#19845=ADVANCED_FACE('',(#2149),#1038,.T.);
#19846=ADVANCED_FACE('',(#2150),#1039,.F.);
#19847=ADVANCED_FACE('',(#2151),#168,.T.);
#19848=ADVANCED_FACE('',(#2152),#18771,.F.);
#19849=ADVANCED_FACE('',(#2153,#1124),#1040,.T.);
#19850=ADVANCED_FACE('',(#2154),#169,.T.);
#19851=ADVANCED_FACE('',(#2155,#1125),#1041,.T.);
#19852=ADVANCED_FACE('',(#2156),#18772,.T.);
#19853=ADVANCED_FACE('',(#2157),#1042,.F.);
#19854=ADVANCED_FACE('',(#2158),#18773,.T.);
#19855=ADVANCED_FACE('',(#2159),#18774,.T.);
#19856=ADVANCED_FACE('',(#2160),#1043,.F.);
#19857=ADVANCED_FACE('',(#2161),#18775,.T.);
#19858=ADVANCED_FACE('',(#2162),#18776,.T.);
#19859=ADVANCED_FACE('',(#2163),#1044,.F.);
#19860=ADVANCED_FACE('',(#2164),#18777,.T.);
#19861=ADVANCED_FACE('',(#2165),#170,.T.);
#19862=ADVANCED_FACE('',(#2166),#314,.T.);
#19863=ADVANCED_FACE('',(#2167),#18778,.T.);
#19864=ADVANCED_FACE('',(#2168),#315,.T.);
#19865=ADVANCED_FACE('',(#2169),#316,.T.);
#19866=ADVANCED_FACE('',(#2170),#18779,.T.);
#19867=ADVANCED_FACE('',(#2171),#844,.F.);
#19868=ADVANCED_FACE('',(#2172),#495,.T.);
#19869=ADVANCED_FACE('',(#2173),#845,.F.);
#19870=ADVANCED_FACE('',(#2174),#1045,.F.);
#19871=ADVANCED_FACE('',(#2175),#18780,.T.);
#19872=ADVANCED_FACE('',(#2176),#317,.T.);
#19873=ADVANCED_FACE('',(#2177),#1046,.T.);
#19874=ADVANCED_FACE('',(#2178),#171,.T.);
#19875=ADVANCED_FACE('',(#2179),#18781,.T.);
#19876=ADVANCED_FACE('',(#2180),#18782,.T.);
#19877=ADVANCED_FACE('',(#2181),#318,.T.);
#19878=ADVANCED_FACE('',(#2182),#319,.T.);
#19879=ADVANCED_FACE('',(#2183),#846,.F.);
#19880=ADVANCED_FACE('',(#2184),#172,.T.);
#19881=ADVANCED_FACE('',(#2185),#496,.T.);
#19882=ADVANCED_FACE('',(#2186),#173,.T.);
#19883=ADVANCED_FACE('',(#2187),#174,.T.);
#19884=ADVANCED_FACE('',(#2188),#1047,.F.);
#19885=ADVANCED_FACE('',(#2189),#320,.T.);
#19886=ADVANCED_FACE('',(#2190),#175,.T.);
#19887=ADVANCED_FACE('',(#2191),#321,.T.);
#19888=ADVANCED_FACE('',(#2192),#322,.T.);
#19889=ADVANCED_FACE('',(#2193),#323,.T.);
#19890=ADVANCED_FACE('',(#2194),#847,.F.);
#19891=ADVANCED_FACE('',(#2195),#848,.F.);
#19892=ADVANCED_FACE('',(#2196),#18783,.T.);
#19893=ADVANCED_FACE('',(#2197),#18784,.T.);
#19894=ADVANCED_FACE('',(#2198),#1048,.F.);
#19895=ADVANCED_FACE('',(#2199),#18785,.T.);
#19896=ADVANCED_FACE('',(#2200),#176,.T.);
#19897=ADVANCED_FACE('',(#2201),#1049,.F.);
#19898=ADVANCED_FACE('',(#2202),#324,.T.);
#19899=ADVANCED_FACE('',(#2203),#325,.T.);
#19900=ADVANCED_FACE('',(#2204),#18786,.T.);
#19901=ADVANCED_FACE('',(#2205),#1050,.F.);
#19902=ADVANCED_FACE('',(#2206),#18787,.T.);
#19903=ADVANCED_FACE('',(#2207),#326,.T.);
#19904=ADVANCED_FACE('',(#2208),#849,.F.);
#19905=ADVANCED_FACE('',(#2209),#18788,.T.);
#19906=ADVANCED_FACE('',(#2210),#177,.T.);
#19907=ADVANCED_FACE('',(#2211),#327,.T.);
#19908=ADVANCED_FACE('',(#2212),#1051,.F.);
#19909=ADVANCED_FACE('',(#2213),#18789,.T.);
#19910=ADVANCED_FACE('',(#2214),#1052,.T.);
#19911=ADVANCED_FACE('',(#2215),#18790,.T.);
#19912=ADVANCED_FACE('',(#2216),#328,.T.);
#19913=ADVANCED_FACE('',(#2217),#178,.T.);
#19914=ADVANCED_FACE('',(#2218),#1053,.F.);
#19915=ADVANCED_FACE('',(#2219),#179,.T.);
#19916=ADVANCED_FACE('',(#2220),#180,.T.);
#19917=ADVANCED_FACE('',(#2221),#18791,.T.);
#19918=ADVANCED_FACE('',(#2222),#181,.T.);
#19919=ADVANCED_FACE('',(#2223),#329,.T.);
#19920=ADVANCED_FACE('',(#2224),#18792,.T.);
#19921=ADVANCED_FACE('',(#2225),#18793,.F.);
#19922=ADVANCED_FACE('',(#2226),#18794,.T.);
#19923=ADVANCED_FACE('',(#2227),#182,.T.);
#19924=ADVANCED_FACE('',(#2228),#1054,.T.);
#19925=ADVANCED_FACE('',(#2229),#18795,.T.);
#19926=ADVANCED_FACE('',(#2230),#183,.T.);
#19927=ADVANCED_FACE('',(#2231),#1055,.T.);
#19928=ADVANCED_FACE('',(#2232),#18796,.T.);
#19929=ADVANCED_FACE('',(#2233),#184,.T.);
#19930=ADVANCED_FACE('',(#2234),#330,.T.);
#19931=ADVANCED_FACE('',(#2235),#18797,.T.);
#19932=ADVANCED_FACE('',(#2236),#185,.T.);
#19933=ADVANCED_FACE('',(#2237),#186,.T.);
#19934=ADVANCED_FACE('',(#2238),#187,.T.);
#19935=ADVANCED_FACE('',(#2239),#1056,.F.);
#19936=ADVANCED_FACE('',(#2240),#18798,.T.);
#19937=ADVANCED_FACE('',(#2241),#18799,.T.);
#19938=ADVANCED_FACE('',(#2242),#331,.T.);
#19939=ADVANCED_FACE('',(#2243),#18800,.T.);
#19940=ADVANCED_FACE('',(#2244),#1057,.F.);
#19941=ADVANCED_FACE('',(#2245),#188,.T.);
#19942=ADVANCED_FACE('',(#2246),#1058,.T.);
#19943=ADVANCED_FACE('',(#2247),#18801,.T.);
#19944=ADVANCED_FACE('',(#2248),#332,.T.);
#19945=ADVANCED_FACE('',(#2249),#333,.T.);
#19946=ADVANCED_FACE('',(#2250),#18802,.T.);
#19947=ADVANCED_FACE('',(#2251),#189,.T.);
#19948=ADVANCED_FACE('',(#2252),#18803,.T.);
#19949=ADVANCED_FACE('',(#2253),#1059,.F.);
#19950=ADVANCED_FACE('',(#2254),#1060,.T.);
#19951=ADVANCED_FACE('',(#2255),#18804,.T.);
#19952=ADVANCED_FACE('',(#2256),#1061,.F.);
#19953=ADVANCED_FACE('',(#2257),#18805,.T.);
#19954=ADVANCED_FACE('',(#2258),#1062,.F.);
#19955=ADVANCED_FACE('',(#2259),#190,.T.);
#19956=ADVANCED_FACE('',(#2260),#1063,.T.);
#19957=ADVANCED_FACE('',(#2261),#191,.T.);
#19958=ADVANCED_FACE('',(#2262),#497,.T.);
#19959=ADVANCED_FACE('',(#2263),#18806,.T.);
#19960=ADVANCED_FACE('',(#2264),#1064,.F.);
#19961=ADVANCED_FACE('',(#2265),#18807,.T.);
#19962=ADVANCED_FACE('',(#2266),#1065,.F.);
#19963=ADVANCED_FACE('',(#2267),#18808,.T.);
#19964=ADVANCED_FACE('',(#2268),#1066,.F.);
#19965=ADVANCED_FACE('',(#2269),#18809,.T.);
#19966=ADVANCED_FACE('',(#2270),#192,.T.);
#19967=ADVANCED_FACE('',(#2271),#334,.T.);
#19968=ADVANCED_FACE('',(#2272),#18810,.T.);
#19969=ADVANCED_FACE('',(#2273),#18811,.F.);
#19970=ADVANCED_FACE('',(#2274),#1067,.T.);
#19971=ADVANCED_FACE('',(#2275),#850,.F.);
#19972=ADVANCED_FACE('',(#2276),#1068,.F.);
#19973=ADVANCED_FACE('',(#2277),#193,.T.);
#19974=ADVANCED_FACE('',(#2278),#1069,.T.);
#19975=ADVANCED_FACE('',(#2279),#194,.T.);
#19976=ADVANCED_FACE('',(#2280),#851,.F.);
#19977=ADVANCED_FACE('',(#2281),#1070,.F.);
#19978=ADVANCED_FACE('',(#2282),#195,.T.);
#19979=ADVANCED_FACE('',(#2283),#1071,.T.);
#19980=ADVANCED_FACE('',(#2284),#196,.T.);
#19981=ADVANCED_FACE('',(#2285),#852,.F.);
#19982=ADVANCED_FACE('',(#2286),#1072,.F.);
#19983=ADVANCED_FACE('',(#2287),#1073,.T.);
#19984=ADVANCED_FACE('',(#2288),#197,.T.);
#19985=ADVANCED_FACE('',(#2289),#18812,.T.);
#19986=ADVANCED_FACE('',(#2290),#335,.T.);
#19987=ADVANCED_FACE('',(#2291),#18813,.F.);
#19988=ADVANCED_FACE('',(#2292),#18814,.T.);
#19989=ADVANCED_FACE('',(#2293),#1074,.F.);
#19990=ADVANCED_FACE('',(#2294),#198,.T.);
#19991=ADVANCED_FACE('',(#2295),#18815,.T.);
#19992=ADVANCED_FACE('',(#2296),#1075,.F.);
#19993=ADVANCED_FACE('',(#2297),#1076,.F.);
#19994=ADVANCED_FACE('',(#2298),#18816,.T.);
#19995=ADVANCED_FACE('',(#2299),#1077,.F.);
#19996=ADVANCED_FACE('',(#2300),#18817,.T.);
#19997=ADVANCED_FACE('',(#2301),#18818,.T.);
#19998=ADVANCED_FACE('',(#2302),#18819,.T.);
#19999=ADVANCED_FACE('',(#2303),#199,.T.);
#20000=ADVANCED_FACE('',(#2304),#1078,.T.);
#20001=ADVANCED_FACE('',(#2305),#1079,.F.);
#20002=ADVANCED_FACE('',(#2306),#1080,.F.);
#20003=ADVANCED_FACE('',(#2307),#18820,.F.);
#20004=ADVANCED_FACE('',(#2308),#18821,.F.);
#20005=ADVANCED_FACE('',(#2309),#1081,.F.);
#20006=ADVANCED_FACE('',(#2310),#498,.T.);
#20007=ADVANCED_FACE('',(#2311),#499,.T.);
#20008=CLOSED_SHELL('',(#18822,#18823,#18824,#18825,#18826,#18827,#18828,
#18829,#18830,#18831,#18832,#18833,#18834,#18835,#18836,#18837,#18838,#18839,
#18840,#18841,#18842,#18843,#18844,#18845,#18846,#18847,#18848,#18849,#18850,
#18851,#18852,#18853,#18854,#18855,#18856,#18857,#18858,#18859,#18860,#18861,
#18862,#18863,#18864,#18865,#18866,#18867,#18868,#18869,#18870,#18871,#18872,
#18873,#18874,#18875,#18876,#18877,#18878,#18879,#18880,#18881,#18882,#18883,
#18884,#18885,#18886,#18887,#18888,#18889,#18890,#18891,#18892,#18893,#18894,
#18895,#18896,#18897,#18898,#18899,#18900,#18901,#18902,#18903,#18904,#18905,
#18906,#18907,#18908,#18909,#18910,#18911,#18912,#18913,#18914,#18915,#18916,
#18917,#18918,#18919,#18920,#18921,#18922,#18923,#18924,#18925,#18926,#18927,
#18928,#18929,#18930,#18931,#18932,#18933,#18934,#18935,#18936,#18937,#18938,
#18939,#18940,#18941,#18942,#18943,#18944,#18945,#18946,#18947,#18948,#18949,
#18950,#18951,#18952,#18953,#18954,#18955,#18956,#18957,#18958,#18959,#18960,
#18961,#18962,#18963,#18964,#18965,#18966,#18967,#18968,#18969,#18970,#18971,
#18972,#18973,#18974,#18975,#18976,#18977,#18978,#18979,#18980,#18981,#18982,
#18983,#18984,#18985,#18986,#18987,#18988,#18989,#18990,#18991,#18992,#18993,
#18994,#18995,#18996,#18997,#18998,#18999,#19000,#19001,#19002,#19003,#19004,
#19005,#19006,#19007,#19008,#19009,#19010,#19011,#19012,#19013,#19014,#19015,
#19016,#19017,#19018,#19019,#19020,#19021,#19022,#19023,#19024,#19025,#19026,
#19027,#19028,#19029,#19030,#19031,#19032,#19033,#19034,#19035,#19036,#19037,
#19038,#19039,#19040,#19041,#19042,#19043,#19044,#19045,#19046,#19047,#19048,
#19049,#19050,#19051,#19052,#19053,#19054,#19055,#19056,#19057,#19058,#19059,
#19060,#19061,#19062,#19063,#19064,#19065,#19066,#19067,#19068,#19069,#19070,
#19071,#19072,#19073,#19074,#19075,#19076,#19077,#19078,#19079,#19080,#19081,
#19082,#19083,#19084,#19085,#19086,#19087,#19088,#19089,#19090,#19091,#19092,
#19093,#19094,#19095,#19096,#19097,#19098,#19099,#19100,#19101,#19102,#19103,
#19104,#19105,#19106,#19107,#19108,#19109,#19110,#19111,#19112,#19113,#19114,
#19115,#19116,#19117,#19118,#19119,#19120));
#20009=CLOSED_SHELL('',(#19121,#19122,#19123,#19124,#19125,#19126,#19127,
#19128,#19129,#19130,#19131,#19132,#19133,#19134,#19135,#19136,#19137,#19138,
#19139,#19140,#19141,#19142,#19143,#19144,#19145,#19146,#19147,#19148,#19149,
#19150,#19151,#19152,#19153,#19154,#19155,#19156,#19157,#19158,#19159,#19160,
#19161,#19162,#19163,#19164,#19165,#19166,#19167,#19168,#19169,#19170,#19171,
#19172,#19173,#19174,#19175,#19176,#19177,#19178,#19179,#19180,#19181,#19182,
#19183,#19184,#19185,#19186,#19187,#19188,#19189,#19190,#19191,#19192,#19193,
#19194,#19195,#19196,#19197,#19198,#19199,#19200,#19201,#19202,#19203,#19204,
#19205,#19206,#19207,#19208,#19209,#19210,#19211,#19212,#19213,#19214,#19215,
#19216,#19217,#19218,#19219,#19220,#19221,#19222,#19223,#19224,#19225,#19226,
#19227,#19228,#19229,#19230,#19231,#19232,#19233,#19234,#19235,#19236,#19237,
#19238,#19239,#19240,#19241,#19242,#19243,#19244,#19245,#19246,#19247,#19248,
#19249,#19250,#19251,#19252,#19253,#19254,#19255,#19256,#19257,#19258,#19259,
#19260,#19261,#19262,#19263,#19264,#19265,#19266,#19267,#19268,#19269,#19270,
#19271,#19272,#19273,#19274,#19275,#19276,#19277,#19278,#19279,#19280,#19281,
#19282,#19283,#19284,#19285,#19286,#19287,#19288,#19289,#19290,#19291,#19292,
#19293,#19294,#19295,#19296,#19297,#19298,#19299,#19300,#19301,#19302,#19303,
#19304,#19305,#19306,#19307,#19308,#19309,#19310,#19311,#19312,#19313,#19314,
#19315,#19316,#19317,#19318,#19319,#19320,#19321,#19322,#19323,#19324,#19325,
#19326,#19327,#19328,#19329,#19330,#19331,#19332,#19333,#19334,#19335,#19336,
#19337,#19338,#19339,#19340,#19341,#19342,#19343,#19344,#19345,#19346,#19347,
#19348,#19349,#19350,#19351,#19352,#19353,#19354,#19355,#19356,#19357,#19358,
#19359,#19360,#19361,#19362,#19363,#19364,#19365,#19366,#19367,#19368,#19369,
#19370,#19371,#19372,#19373,#19374,#19375,#19376,#19377,#19378,#19379,#19380,
#19381,#19382,#19383,#19384,#19385,#19386,#19387,#19388,#19389,#19390,#19391,
#19392,#19393,#19394,#19395,#19396,#19397,#19398,#19399,#19400,#19401,#19402,
#19403,#19404,#19405,#19406,#19407,#19408,#19409,#19410,#19411,#19412,#19413,
#19414,#19415,#19416,#19417,#19418,#19419,#19420,#19421,#19422,#19423,#19424,
#19425,#19426,#19427,#19428,#19429,#19430,#19431,#19432,#19433,#19434,#19435,
#19436,#19437,#19438,#19439,#19440,#19441,#19442,#19443,#19444,#19445,#19446,
#19447));
#20010=CLOSED_SHELL('',(#19448,#19449,#19450,#19451,#19452,#19453,#19454,
#19455,#19456,#19457,#19458,#19459,#19460,#19461,#19462,#19463,#19464,#19465,
#19466,#19467,#19468,#19469,#19470,#19471,#19472,#19473,#19474,#19475,#19476,
#19477,#19478,#19479,#19480,#19481,#19482,#19483,#19484,#19485,#19486,#19487,
#19488,#19489,#19490,#19491,#19492,#19493,#19494,#19495,#19496,#19497,#19498,
#19499,#19500,#19501,#19502,#19503,#19504,#19505,#19506,#19507,#19508,#19509,
#19510,#19511,#19512,#19513,#19514,#19515,#19516,#19517,#19518,#19519,#19520,
#19521,#19522,#19523,#19524,#19525,#19526,#19527,#19528,#19529,#19530,#19531,
#19532,#19533,#19534,#19535,#19536,#19537,#19538,#19539,#19540,#19541,#19542,
#19543,#19544,#19545,#19546,#19547,#19548,#19549,#19550,#19551,#19552,#19553,
#19554,#19555,#19556,#19557,#19558,#19559,#19560,#19561,#19562,#19563,#19564,
#19565,#19566,#19567,#19568,#19569,#19570,#19571,#19572,#19573,#19574,#19575,
#19576,#19577,#19578,#19579,#19580,#19581,#19582,#19583,#19584,#19585,#19586,
#19587,#19588,#19589,#19590,#19591,#19592,#19593,#19594,#19595,#19596,#19597,
#19598,#19599,#19600,#19601,#19602,#19603,#19604,#19605,#19606,#19607,#19608,
#19609,#19610,#19611,#19612,#19613,#19614,#19615,#19616,#19617,#19618,#19619,
#19620,#19621,#19622,#19623,#19624,#19625,#19626,#19627,#19628,#19629,#19630,
#19631,#19632,#19633,#19634,#19635,#19636,#19637,#19638,#19639,#19640,#19641,
#19642,#19643,#19644,#19645,#19646,#19647,#19648,#19649,#19650,#19651,#19652,
#19653,#19654,#19655,#19656,#19657,#19658,#19659,#19660,#19661,#19662,#19663,
#19664,#19665,#19666,#19667,#19668,#19669,#19670,#19671,#19672,#19673));
#20011=CLOSED_SHELL('',(#19674,#19675,#19676,#19677,#19678,#19679,#19680,
#19681,#19682));
#20012=CLOSED_SHELL('',(#19683,#19684,#19685,#19686,#19687,#19688,#19689,
#19690,#19691,#19692,#19693,#19694,#19695,#19696,#19697,#19698,#19699));
#20013=CLOSED_SHELL('',(#19700,#19701,#19702,#19703,#19704,#19705,#19706,
#19707,#19708));
#20014=CLOSED_SHELL('',(#19709,#19710,#19711));
#20015=CLOSED_SHELL('',(#19712,#19713,#19714,#19715,#19716,#19717,#19718,
#19719,#19720,#19721,#19722,#19723,#19724,#19725,#19726,#19727,#19728,#19729,
#19730,#19731,#19732,#19733,#19734,#19735,#19736,#19737,#19738,#19739,#19740,
#19741,#19742,#19743,#19744,#19745,#19746,#19747,#19748,#19749,#19750,#19751,
#19752,#19753,#19754,#19755,#19756,#19757,#19758,#19759,#19760,#19761,#19762,
#19763,#19764,#19765,#19766,#19767,#19768,#19769,#19770,#19771,#19772,#19773,
#19774,#19775,#19776,#19777,#19778,#19779,#19780,#19781,#19782,#19783,#19784,
#19785,#19786,#19787,#19788,#19789,#19790,#19791,#19792,#19793,#19794,#19795,
#19796,#19797,#19798,#19799,#19800,#19801,#19802,#19803,#19804,#19805,#19806,
#19807,#19808,#19809,#19810,#19811,#19812,#19813,#19814,#19815,#19816,#19817));
#20016=CLOSED_SHELL('',(#19818,#19819,#19820,#19821,#19822,#19823,#19824,
#19825,#19826,#19827,#19828,#19829,#19830,#19831,#19832,#19833,#19834,#19835,
#19836,#19837,#19838,#19839,#19840,#19841,#19842,#19843));
#20017=CLOSED_SHELL('',(#19844,#19845,#19846));
#20018=CLOSED_SHELL('',(#19847,#19848,#19849,#19850,#19851,#19852,#19853,
#19854,#19855,#19856,#19857,#19858,#19859,#19860,#19861,#19862,#19863,#19864,
#19865,#19866,#19867,#19868,#19869,#19870,#19871,#19872,#19873,#19874,#19875,
#19876,#19877,#19878,#19879,#19880,#19881,#19882,#19883,#19884,#19885,#19886,
#19887,#19888,#19889,#19890,#19891,#19892,#19893,#19894,#19895,#19896,#19897,
#19898,#19899,#19900,#19901,#19902,#19903,#19904,#19905,#19906,#19907,#19908,
#19909,#19910,#19911,#19912,#19913,#19914,#19915,#19916,#19917,#19918,#19919,
#19920,#19921,#19922,#19923,#19924,#19925,#19926,#19927,#19928,#19929,#19930,
#19931,#19932,#19933,#19934,#19935,#19936,#19937,#19938,#19939,#19940,#19941,
#19942,#19943,#19944,#19945,#19946,#19947,#19948,#19949,#19950,#19951,#19952,
#19953,#19954,#19955,#19956,#19957,#19958,#19959,#19960,#19961,#19962,#19963,
#19964,#19965,#19966,#19967,#19968,#19969,#19970,#19971,#19972,#19973,#19974,
#19975,#19976,#19977,#19978,#19979,#19980,#19981,#19982,#19983,#19984,#19985,
#19986,#19987,#19988,#19989,#19990,#19991,#19992,#19993,#19994,#19995,#19996,
#19997,#19998,#19999,#20000,#20001,#20002,#20003,#20004,#20005,#20006,#20007));
#20019=DERIVED_UNIT_ELEMENT(#20041,1.);
#20020=DERIVED_UNIT_ELEMENT(#65565,-3.);
#20021=DERIVED_UNIT_ELEMENT(#20041,1.);
#20022=DERIVED_UNIT_ELEMENT(#65565,-3.);
#20023=DERIVED_UNIT_ELEMENT(#20041,1.);
#20024=DERIVED_UNIT_ELEMENT(#65565,-3.);
#20025=DERIVED_UNIT_ELEMENT(#20041,1.);
#20026=DERIVED_UNIT_ELEMENT(#65565,-3.);
#20027=DERIVED_UNIT_ELEMENT(#20041,1.);
#20028=DERIVED_UNIT_ELEMENT(#65565,-3.);
#20029=DERIVED_UNIT_ELEMENT(#20041,1.);
#20030=DERIVED_UNIT_ELEMENT(#65565,-3.);
#20031=DERIVED_UNIT_ELEMENT(#20041,1.);
#20032=DERIVED_UNIT_ELEMENT(#65565,-3.);
#20033=DERIVED_UNIT_ELEMENT(#20041,1.);
#20034=DERIVED_UNIT_ELEMENT(#65565,-3.);
#20035=DERIVED_UNIT_ELEMENT(#20041,1.);
#20036=DERIVED_UNIT_ELEMENT(#65565,-3.);
#20037=DERIVED_UNIT_ELEMENT(#20041,1.);
#20038=DERIVED_UNIT_ELEMENT(#65565,-3.);
#20039=DERIVED_UNIT_ELEMENT(#20041,1.);
#20040=DERIVED_UNIT_ELEMENT(#65565,-3.);
#20041=(
MASS_UNIT()
NAMED_UNIT(*)
SI_UNIT(.KILO.,.GRAM.)
);
#20042=DERIVED_UNIT((#20019,#20020));
#20043=DERIVED_UNIT((#20021,#20022));
#20044=DERIVED_UNIT((#20023,#20024));
#20045=DERIVED_UNIT((#20025,#20026));
#20046=DERIVED_UNIT((#20027,#20028));
#20047=DERIVED_UNIT((#20029,#20030));
#20048=DERIVED_UNIT((#20031,#20032));
#20049=DERIVED_UNIT((#20033,#20034));
#20050=DERIVED_UNIT((#20035,#20036));
#20051=DERIVED_UNIT((#20037,#20038));
#20052=DERIVED_UNIT((#20039,#20040));
#20053=MEASURE_REPRESENTATION_ITEM('density measure',
POSITIVE_RATIO_MEASURE(7850.),#20042);
#20054=MEASURE_REPRESENTATION_ITEM('density measure',
POSITIVE_RATIO_MEASURE(7850.),#20043);
#20055=MEASURE_REPRESENTATION_ITEM('density measure',
POSITIVE_RATIO_MEASURE(7850.),#20044);
#20056=MEASURE_REPRESENTATION_ITEM('density measure',
POSITIVE_RATIO_MEASURE(7850.),#20045);
#20057=MEASURE_REPRESENTATION_ITEM('density measure',
POSITIVE_RATIO_MEASURE(7850.),#20046);
#20058=MEASURE_REPRESENTATION_ITEM('density measure',
POSITIVE_RATIO_MEASURE(7850.),#20047);
#20059=MEASURE_REPRESENTATION_ITEM('density measure',
POSITIVE_RATIO_MEASURE(7850.),#20048);
#20060=MEASURE_REPRESENTATION_ITEM('density measure',
POSITIVE_RATIO_MEASURE(7850.),#20049);
#20061=MEASURE_REPRESENTATION_ITEM('density measure',
POSITIVE_RATIO_MEASURE(7850.),#20050);
#20062=MEASURE_REPRESENTATION_ITEM('density measure',
POSITIVE_RATIO_MEASURE(7850.),#20051);
#20063=MEASURE_REPRESENTATION_ITEM('density measure',
POSITIVE_RATIO_MEASURE(7850.),#20052);
#20064=PROPERTY_DEFINITION_REPRESENTATION(#20119,#20086);
#20065=PROPERTY_DEFINITION_REPRESENTATION(#20120,#20087);
#20066=PROPERTY_DEFINITION_REPRESENTATION(#20121,#20088);
#20067=PROPERTY_DEFINITION_REPRESENTATION(#20122,#20089);
#20068=PROPERTY_DEFINITION_REPRESENTATION(#20123,#20090);
#20069=PROPERTY_DEFINITION_REPRESENTATION(#20124,#20091);
#20070=PROPERTY_DEFINITION_REPRESENTATION(#20125,#20092);
#20071=PROPERTY_DEFINITION_REPRESENTATION(#20126,#20093);
#20072=PROPERTY_DEFINITION_REPRESENTATION(#20127,#20094);
#20073=PROPERTY_DEFINITION_REPRESENTATION(#20128,#20095);
#20074=PROPERTY_DEFINITION_REPRESENTATION(#20129,#20096);
#20075=PROPERTY_DEFINITION_REPRESENTATION(#20130,#20097);
#20076=PROPERTY_DEFINITION_REPRESENTATION(#20131,#20098);
#20077=PROPERTY_DEFINITION_REPRESENTATION(#20132,#20099);
#20078=PROPERTY_DEFINITION_REPRESENTATION(#20133,#20100);
#20079=PROPERTY_DEFINITION_REPRESENTATION(#20134,#20101);
#20080=PROPERTY_DEFINITION_REPRESENTATION(#20135,#20102);
#20081=PROPERTY_DEFINITION_REPRESENTATION(#20136,#20103);
#20082=PROPERTY_DEFINITION_REPRESENTATION(#20137,#20104);
#20083=PROPERTY_DEFINITION_REPRESENTATION(#20138,#20105);
#20084=PROPERTY_DEFINITION_REPRESENTATION(#20139,#20106);
#20085=PROPERTY_DEFINITION_REPRESENTATION(#20140,#20107);
#20086=REPRESENTATION('material name',(#20108),#65552);
#20087=REPRESENTATION('density',(#20053),#65552);
#20088=REPRESENTATION('material name',(#20109),#65553);
#20089=REPRESENTATION('density',(#20054),#65553);
#20090=REPRESENTATION('material name',(#20110),#65554);
#20091=REPRESENTATION('density',(#20055),#65554);
#20092=REPRESENTATION('material name',(#20111),#65555);
#20093=REPRESENTATION('density',(#20056),#65555);
#20094=REPRESENTATION('material name',(#20112),#65556);
#20095=REPRESENTATION('density',(#20057),#65556);
#20096=REPRESENTATION('material name',(#20113),#65557);
#20097=REPRESENTATION('density',(#20058),#65557);
#20098=REPRESENTATION('material name',(#20114),#65558);
#20099=REPRESENTATION('density',(#20059),#65558);
#20100=REPRESENTATION('material name',(#20115),#65559);
#20101=REPRESENTATION('density',(#20060),#65559);
#20102=REPRESENTATION('material name',(#20116),#65560);
#20103=REPRESENTATION('density',(#20061),#65560);
#20104=REPRESENTATION('material name',(#20117),#65561);
#20105=REPRESENTATION('density',(#20062),#65561);
#20106=REPRESENTATION('material name',(#20118),#65562);
#20107=REPRESENTATION('density',(#20063),#65562);
#20108=DESCRIPTIVE_REPRESENTATION_ITEM('Steel','Steel');
#20109=DESCRIPTIVE_REPRESENTATION_ITEM('Steel','Steel');
#20110=DESCRIPTIVE_REPRESENTATION_ITEM('Steel','Steel');
#20111=DESCRIPTIVE_REPRESENTATION_ITEM('Steel','Steel');
#20112=DESCRIPTIVE_REPRESENTATION_ITEM('Steel','Steel');
#20113=DESCRIPTIVE_REPRESENTATION_ITEM('Steel','Steel');
#20114=DESCRIPTIVE_REPRESENTATION_ITEM('Steel','Steel');
#20115=DESCRIPTIVE_REPRESENTATION_ITEM('Steel','Steel');
#20116=DESCRIPTIVE_REPRESENTATION_ITEM('Steel','Steel');
#20117=DESCRIPTIVE_REPRESENTATION_ITEM('Steel','Steel');
#20118=DESCRIPTIVE_REPRESENTATION_ITEM('Steel','Steel');
#20119=PROPERTY_DEFINITION('material property','material name',#65627);
#20120=PROPERTY_DEFINITION('material property','density of part',#65627);
#20121=PROPERTY_DEFINITION('material property','material name',#65628);
#20122=PROPERTY_DEFINITION('material property','density of part',#65628);
#20123=PROPERTY_DEFINITION('material property','material name',#65629);
#20124=PROPERTY_DEFINITION('material property','density of part',#65629);
#20125=PROPERTY_DEFINITION('material property','material name',#65630);
#20126=PROPERTY_DEFINITION('material property','density of part',#65630);
#20127=PROPERTY_DEFINITION('material property','material name',#65631);
#20128=PROPERTY_DEFINITION('material property','density of part',#65631);
#20129=PROPERTY_DEFINITION('material property','material name',#65632);
#20130=PROPERTY_DEFINITION('material property','density of part',#65632);
#20131=PROPERTY_DEFINITION('material property','material name',#65633);
#20132=PROPERTY_DEFINITION('material property','density of part',#65633);
#20133=PROPERTY_DEFINITION('material property','material name',#65634);
#20134=PROPERTY_DEFINITION('material property','density of part',#65634);
#20135=PROPERTY_DEFINITION('material property','material name',#65635);
#20136=PROPERTY_DEFINITION('material property','density of part',#65635);
#20137=PROPERTY_DEFINITION('material property','material name',#65636);
#20138=PROPERTY_DEFINITION('material property','density of part',#65636);
#20139=PROPERTY_DEFINITION('material property','material name',#65637);
#20140=PROPERTY_DEFINITION('material property','density of part',#65637);
#20141=AXIS2_PLACEMENT_3D('',#27819,#22403,#22404);
#20142=AXIS2_PLACEMENT_3D('',#27820,#22405,#22406);
#20143=AXIS2_PLACEMENT_3D('',#27821,#22407,#22408);
#20144=AXIS2_PLACEMENT_3D('',#27852,#22410,#22411);
#20145=AXIS2_PLACEMENT_3D('',#27856,#22413,#22414);
#20146=AXIS2_PLACEMENT_3D('',#27860,#22416,#22417);
#20147=AXIS2_PLACEMENT_3D('',#27863,#22419,#22420);
#20148=AXIS2_PLACEMENT_3D('',#27865,#22421,#22422);
#20149=AXIS2_PLACEMENT_3D('',#27868,#22424,#22425);
#20150=AXIS2_PLACEMENT_3D('',#27870,#22426,#22427);
#20151=AXIS2_PLACEMENT_3D('',#27897,#22429,#22430);
#20152=AXIS2_PLACEMENT_3D('',#27900,#22432,#22433);
#20153=AXIS2_PLACEMENT_3D('',#27901,#22434,#22435);
#20154=AXIS2_PLACEMENT_3D('',#27961,#22437,#22438);
#20155=AXIS2_PLACEMENT_3D('',#28021,#22440,#22441);
#20156=AXIS2_PLACEMENT_3D('',#28078,#22443,#22444);
#20157=AXIS2_PLACEMENT_3D('',#28138,#22446,#22447);
#20158=AXIS2_PLACEMENT_3D('',#28198,#22449,#22450);
#20159=AXIS2_PLACEMENT_3D('',#28258,#22452,#22453);
#20160=AXIS2_PLACEMENT_3D('',#28315,#22455,#22456);
#20161=AXIS2_PLACEMENT_3D('',#28372,#22458,#22459);
#20162=AXIS2_PLACEMENT_3D('',#28435,#22461,#22462);
#20163=AXIS2_PLACEMENT_3D('',#28489,#22464,#22465);
#20164=AXIS2_PLACEMENT_3D('',#28549,#22467,#22468);
#20165=AXIS2_PLACEMENT_3D('',#28609,#22470,#22471);
#20166=AXIS2_PLACEMENT_3D('',#28666,#22473,#22474);
#20167=AXIS2_PLACEMENT_3D('',#28723,#22476,#22477);
#20168=AXIS2_PLACEMENT_3D('',#28789,#22479,#22480);
#20169=AXIS2_PLACEMENT_3D('',#28849,#22482,#22483);
#20170=AXIS2_PLACEMENT_3D('',#28906,#22485,#22486);
#20171=AXIS2_PLACEMENT_3D('',#28963,#22488,#22489);
#20172=AXIS2_PLACEMENT_3D('',#29026,#22491,#22492);
#20173=AXIS2_PLACEMENT_3D('',#29080,#22494,#22495);
#20174=AXIS2_PLACEMENT_3D('',#29137,#22497,#22498);
#20175=AXIS2_PLACEMENT_3D('',#29197,#22500,#22501);
#20176=AXIS2_PLACEMENT_3D('',#29254,#22503,#22504);
#20177=AXIS2_PLACEMENT_3D('',#29311,#22506,#22507);
#20178=AXIS2_PLACEMENT_3D('',#29377,#22509,#22510);
#20179=AXIS2_PLACEMENT_3D('',#29437,#22512,#22513);
#20180=AXIS2_PLACEMENT_3D('',#29494,#22515,#22516);
#20181=AXIS2_PLACEMENT_3D('',#29551,#22518,#22519);
#20182=AXIS2_PLACEMENT_3D('',#29611,#22521,#22522);
#20183=AXIS2_PLACEMENT_3D('',#29665,#22524,#22525);
#20184=AXIS2_PLACEMENT_3D('',#29722,#22527,#22528);
#20185=AXIS2_PLACEMENT_3D('',#29785,#22530,#22531);
#20186=AXIS2_PLACEMENT_3D('',#29845,#22533,#22534);
#20187=AXIS2_PLACEMENT_3D('',#29899,#22536,#22537);
#20188=AXIS2_PLACEMENT_3D('',#29959,#22539,#22540);
#20189=AXIS2_PLACEMENT_3D('',#30019,#22542,#22543);
#20190=AXIS2_PLACEMENT_3D('',#30076,#22545,#22546);
#20191=AXIS2_PLACEMENT_3D('',#30136,#22548,#22549);
#20192=AXIS2_PLACEMENT_3D('',#30196,#22551,#22552);
#20193=AXIS2_PLACEMENT_3D('',#30253,#22554,#22555);
#20194=AXIS2_PLACEMENT_3D('',#30313,#22557,#22558);
#20195=AXIS2_PLACEMENT_3D('',#30373,#22560,#22561);
#20196=AXIS2_PLACEMENT_3D('',#30433,#22563,#22564);
#20197=AXIS2_PLACEMENT_3D('',#30487,#22566,#22567);
#20198=AXIS2_PLACEMENT_3D('',#30544,#22569,#22570);
#20199=AXIS2_PLACEMENT_3D('',#30607,#22572,#22573);
#20200=AXIS2_PLACEMENT_3D('',#30664,#22575,#22576);
#20201=AXIS2_PLACEMENT_3D('',#30724,#22578,#22579);
#20202=AXIS2_PLACEMENT_3D('',#30784,#22581,#22582);
#20203=AXIS2_PLACEMENT_3D('',#30841,#22584,#22585);
#20204=AXIS2_PLACEMENT_3D('',#30901,#22587,#22588);
#20205=AXIS2_PLACEMENT_3D('',#30964,#22590,#22591);
#20206=AXIS2_PLACEMENT_3D('',#31024,#22593,#22594);
#20207=AXIS2_PLACEMENT_3D('',#31078,#22596,#22597);
#20208=AXIS2_PLACEMENT_3D('',#31135,#22599,#22600);
#20209=AXIS2_PLACEMENT_3D('',#31195,#22602,#22603);
#20210=AXIS2_PLACEMENT_3D('',#31252,#22605,#22606);
#20211=AXIS2_PLACEMENT_3D('',#31309,#22608,#22609);
#20212=AXIS2_PLACEMENT_3D('',#31369,#22611,#22612);
#20213=AXIS2_PLACEMENT_3D('',#31426,#22614,#22615);
#20214=AXIS2_PLACEMENT_3D('',#31486,#22617,#22618);
#20215=AXIS2_PLACEMENT_3D('',#31505,#22620,#22621);
#20216=AXIS2_PLACEMENT_3D('',#31508,#22623,#22624);
#20217=AXIS2_PLACEMENT_3D('',#31510,#22625,#22626);
#20218=AXIS2_PLACEMENT_3D('',#31518,#22627,#22628);
#20219=AXIS2_PLACEMENT_3D('',#31608,#22630,#22631);
#20220=AXIS2_PLACEMENT_3D('',#31692,#22633,#22634);
#20221=AXIS2_PLACEMENT_3D('',#31782,#22636,#22637);
#20222=AXIS2_PLACEMENT_3D('',#31872,#22639,#22640);
#20223=AXIS2_PLACEMENT_3D('',#31956,#22642,#22643);
#20224=AXIS2_PLACEMENT_3D('',#32046,#22645,#22646);
#20225=AXIS2_PLACEMENT_3D('',#32130,#22648,#22649);
#20226=AXIS2_PLACEMENT_3D('',#32220,#22651,#22652);
#20227=AXIS2_PLACEMENT_3D('',#32310,#22654,#22655);
#20228=AXIS2_PLACEMENT_3D('',#32394,#22657,#22658);
#20229=AXIS2_PLACEMENT_3D('',#32484,#22660,#22661);
#20230=AXIS2_PLACEMENT_3D('',#32574,#22663,#22664);
#20231=AXIS2_PLACEMENT_3D('',#32658,#22666,#22667);
#20232=AXIS2_PLACEMENT_3D('',#32748,#22669,#22670);
#20233=AXIS2_PLACEMENT_3D('',#32832,#22672,#22673);
#20234=AXIS2_PLACEMENT_3D('',#32847,#22675,#22676);
#20235=AXIS2_PLACEMENT_3D('',#32854,#22677,#22678);
#20236=AXIS2_PLACEMENT_3D('',#32891,#22680,#22681);
#20237=AXIS2_PLACEMENT_3D('',#32928,#22683,#22684);
#20238=AXIS2_PLACEMENT_3D('',#32965,#22686,#22687);
#20239=AXIS2_PLACEMENT_3D('',#33002,#22689,#22690);
#20240=AXIS2_PLACEMENT_3D('',#33040,#22692,#22693);
#20241=AXIS2_PLACEMENT_3D('',#33077,#22695,#22696);
#20242=AXIS2_PLACEMENT_3D('',#33114,#22698,#22699);
#20243=AXIS2_PLACEMENT_3D('',#33152,#22701,#22702);
#20244=AXIS2_PLACEMENT_3D('',#33189,#22704,#22705);
#20245=AXIS2_PLACEMENT_3D('',#33226,#22707,#22708);
#20246=AXIS2_PLACEMENT_3D('',#33263,#22710,#22711);
#20247=AXIS2_PLACEMENT_3D('',#33300,#22713,#22714);
#20248=AXIS2_PLACEMENT_3D('',#33338,#22716,#22717);
#20249=AXIS2_PLACEMENT_3D('',#33375,#22719,#22720);
#20250=AXIS2_PLACEMENT_3D('',#33412,#22722,#22723);
#20251=AXIS2_PLACEMENT_3D('',#33424,#22725,#22726);
#20252=AXIS2_PLACEMENT_3D('',#33425,#22727,#22728);
#20253=AXIS2_PLACEMENT_3D('',#33442,#22730,#22731);
#20254=AXIS2_PLACEMENT_3D('',#33456,#22732,#22733);
#20255=AXIS2_PLACEMENT_3D('',#33484,#22735,#22736);
#20256=AXIS2_PLACEMENT_3D('',#33512,#22738,#22739);
#20257=AXIS2_PLACEMENT_3D('',#33553,#22741,#22742);
#20258=AXIS2_PLACEMENT_3D('',#33594,#22744,#22745);
#20259=AXIS2_PLACEMENT_3D('',#33622,#22747,#22748);
#20260=AXIS2_PLACEMENT_3D('',#33650,#22750,#22751);
#20261=AXIS2_PLACEMENT_3D('',#33691,#22753,#22754);
#20262=AXIS2_PLACEMENT_3D('',#33732,#22756,#22757);
#20263=AXIS2_PLACEMENT_3D('',#33761,#22759,#22760);
#20264=AXIS2_PLACEMENT_3D('',#33789,#22762,#22763);
#20265=AXIS2_PLACEMENT_3D('',#33817,#22765,#22766);
#20266=AXIS2_PLACEMENT_3D('',#33845,#22768,#22769);
#20267=AXIS2_PLACEMENT_3D('',#33886,#22771,#22772);
#20268=AXIS2_PLACEMENT_3D('',#33927,#22774,#22775);
#20269=AXIS2_PLACEMENT_3D('',#33955,#22777,#22778);
#20270=AXIS2_PLACEMENT_3D('',#33983,#22780,#22781);
#20271=AXIS2_PLACEMENT_3D('',#34024,#22783,#22784);
#20272=AXIS2_PLACEMENT_3D('',#34065,#22786,#22787);
#20273=AXIS2_PLACEMENT_3D('',#34094,#22789,#22790);
#20274=AXIS2_PLACEMENT_3D('',#34122,#22792,#22793);
#20275=AXIS2_PLACEMENT_3D('',#34150,#22795,#22796);
#20276=AXIS2_PLACEMENT_3D('',#34178,#22798,#22799);
#20277=AXIS2_PLACEMENT_3D('',#34219,#22801,#22802);
#20278=AXIS2_PLACEMENT_3D('',#34260,#22804,#22805);
#20279=AXIS2_PLACEMENT_3D('',#34288,#22807,#22808);
#20280=AXIS2_PLACEMENT_3D('',#34315,#22810,#22811);
#20281=AXIS2_PLACEMENT_3D('',#34357,#22813,#22814);
#20282=AXIS2_PLACEMENT_3D('',#34398,#22816,#22817);
#20283=AXIS2_PLACEMENT_3D('',#34427,#22819,#22820);
#20284=AXIS2_PLACEMENT_3D('',#34454,#22822,#22823);
#20285=AXIS2_PLACEMENT_3D('',#34495,#22825,#22826);
#20286=AXIS2_PLACEMENT_3D('',#34537,#22828,#22829);
#20287=AXIS2_PLACEMENT_3D('',#34565,#22831,#22832);
#20288=AXIS2_PLACEMENT_3D('',#34592,#22834,#22835);
#20289=AXIS2_PLACEMENT_3D('',#34633,#22837,#22838);
#20290=AXIS2_PLACEMENT_3D('',#34662,#22840,#22841);
#20291=AXIS2_PLACEMENT_3D('',#34704,#22843,#22844);
#20292=AXIS2_PLACEMENT_3D('',#34731,#22846,#22847);
#20293=AXIS2_PLACEMENT_3D('',#34772,#22849,#22850);
#20294=AXIS2_PLACEMENT_3D('',#34801,#22852,#22853);
#20295=AXIS2_PLACEMENT_3D('',#34842,#22855,#22856);
#20296=AXIS2_PLACEMENT_3D('',#34884,#22858,#22859);
#20297=AXIS2_PLACEMENT_3D('',#34912,#22861,#22862);
#20298=AXIS2_PLACEMENT_3D('',#34939,#22864,#22865);
#20299=AXIS2_PLACEMENT_3D('',#34980,#22867,#22868);
#20300=AXIS2_PLACEMENT_3D('',#35009,#22870,#22871);
#20301=AXIS2_PLACEMENT_3D('',#35038,#22873,#22874);
#20302=AXIS2_PLACEMENT_3D('',#35065,#22876,#22877);
#20303=AXIS2_PLACEMENT_3D('',#35106,#22879,#22880);
#20304=AXIS2_PLACEMENT_3D('',#35135,#22882,#22883);
#20305=AXIS2_PLACEMENT_3D('',#35176,#22885,#22886);
#20306=AXIS2_PLACEMENT_3D('',#35218,#22888,#22889);
#20307=AXIS2_PLACEMENT_3D('',#35246,#22891,#22892);
#20308=AXIS2_PLACEMENT_3D('',#35273,#22894,#22895);
#20309=AXIS2_PLACEMENT_3D('',#35314,#22897,#22898);
#20310=AXIS2_PLACEMENT_3D('',#35343,#22900,#22901);
#20311=AXIS2_PLACEMENT_3D('',#35372,#22903,#22904);
#20312=AXIS2_PLACEMENT_3D('',#35399,#22906,#22907);
#20313=AXIS2_PLACEMENT_3D('',#35427,#22909,#22910);
#20314=AXIS2_PLACEMENT_3D('',#35456,#22912,#22913);
#20315=AXIS2_PLACEMENT_3D('',#35497,#22915,#22916);
#20316=AXIS2_PLACEMENT_3D('',#35500,#22919,#22920);
#20317=AXIS2_PLACEMENT_3D('',#35502,#22922,#22923);
#20318=AXIS2_PLACEMENT_3D('',#35504,#22925,#22926);
#20319=AXIS2_PLACEMENT_3D('',#35505,#22927,#22928);
#20320=AXIS2_PLACEMENT_3D('',#35623,#22929,#22930);
#20321=AXIS2_PLACEMENT_3D('',#35625,#22931,#22932);
#20322=AXIS2_PLACEMENT_3D('',#37934,#22933,#22934);
#20323=AXIS2_PLACEMENT_3D('',#38051,#22935,#22936);
#20324=AXIS2_PLACEMENT_3D('',#38052,#22937,#22938);
#20325=AXIS2_PLACEMENT_3D('',#40130,#22939,#22940);
#20326=AXIS2_PLACEMENT_3D('',#40245,#22941,#22942);
#20327=AXIS2_PLACEMENT_3D('',#40247,#22943,#22944);
#20328=AXIS2_PLACEMENT_3D('',#41363,#22945,#22946);
#20329=AXIS2_PLACEMENT_3D('',#41480,#22947,#22948);
#20330=AXIS2_PLACEMENT_3D('',#41481,#22949,#22950);
#20331=AXIS2_PLACEMENT_3D('',#42360,#22951,#22952);
#20332=AXIS2_PLACEMENT_3D('',#42361,#22953,#22954);
#20333=AXIS2_PLACEMENT_3D('',#42362,#22955,#22956);
#20334=AXIS2_PLACEMENT_3D('',#42365,#22957,#22958);
#20335=AXIS2_PLACEMENT_3D('',#42397,#22959,#22960);
#20336=AXIS2_PLACEMENT_3D('',#42547,#22962,#22963);
#20337=AXIS2_PLACEMENT_3D('',#42550,#22965,#22966);
#20338=AXIS2_PLACEMENT_3D('',#42681,#22967,#22968);
#20339=AXIS2_PLACEMENT_3D('',#42682,#22969,#22970);
#20340=AXIS2_PLACEMENT_3D('',#42683,#22971,#22972);
#20341=AXIS2_PLACEMENT_3D('',#42685,#22973,#22974);
#20342=AXIS2_PLACEMENT_3D('',#42691,#22975,#22976);
#20343=AXIS2_PLACEMENT_3D('',#42692,#22977,#22978);
#20344=AXIS2_PLACEMENT_3D('',#42694,#22979,#22980);
#20345=AXIS2_PLACEMENT_3D('',#42700,#22981,#22982);
#20346=AXIS2_PLACEMENT_3D('',#42701,#22983,#22984);
#20347=AXIS2_PLACEMENT_3D('',#42703,#22985,#22986);
#20348=AXIS2_PLACEMENT_3D('',#42708,#22987,#22988);
#20349=AXIS2_PLACEMENT_3D('',#42710,#22989,#22990);
#20350=AXIS2_PLACEMENT_3D('',#42715,#22991,#22992);
#20351=AXIS2_PLACEMENT_3D('',#42717,#22993,#22994);
#20352=AXIS2_PLACEMENT_3D('',#42749,#22995,#22996);
#20353=AXIS2_PLACEMENT_3D('',#42899,#22998,#22999);
#20354=AXIS2_PLACEMENT_3D('',#42902,#23001,#23002);
#20355=AXIS2_PLACEMENT_3D('',#43012,#23003,#23004);
#20356=AXIS2_PLACEMENT_3D('',#43013,#23005,#23006);
#20357=AXIS2_PLACEMENT_3D('',#43014,#23007,#23008);
#20358=AXIS2_PLACEMENT_3D('',#43016,#23009,#23010);
#20359=AXIS2_PLACEMENT_3D('',#43022,#23011,#23012);
#20360=AXIS2_PLACEMENT_3D('',#43023,#23013,#23014);
#20361=AXIS2_PLACEMENT_3D('',#43025,#23015,#23016);
#20362=AXIS2_PLACEMENT_3D('',#43030,#23017,#23018);
#20363=AXIS2_PLACEMENT_3D('',#43032,#23019,#23020);
#20364=AXIS2_PLACEMENT_3D('',#43037,#23021,#23022);
#20365=AXIS2_PLACEMENT_3D('',#43039,#23023,#23024);
#20366=AXIS2_PLACEMENT_3D('',#43071,#23025,#23026);
#20367=AXIS2_PLACEMENT_3D('',#43221,#23028,#23029);
#20368=AXIS2_PLACEMENT_3D('',#43224,#23031,#23032);
#20369=AXIS2_PLACEMENT_3D('',#43334,#23033,#23034);
#20370=AXIS2_PLACEMENT_3D('',#43335,#23035,#23036);
#20371=AXIS2_PLACEMENT_3D('',#43336,#23037,#23038);
#20372=AXIS2_PLACEMENT_3D('',#43338,#23039,#23040);
#20373=AXIS2_PLACEMENT_3D('',#43344,#23041,#23042);
#20374=AXIS2_PLACEMENT_3D('',#43345,#23043,#23044);
#20375=AXIS2_PLACEMENT_3D('',#43347,#23045,#23046);
#20376=AXIS2_PLACEMENT_3D('',#43352,#23047,#23048);
#20377=AXIS2_PLACEMENT_3D('',#43354,#23049,#23050);
#20378=AXIS2_PLACEMENT_3D('',#43359,#23051,#23052);
#20379=AXIS2_PLACEMENT_3D('',#43361,#23053,#23054);
#20380=AXIS2_PLACEMENT_3D('',#43393,#23055,#23056);
#20381=AXIS2_PLACEMENT_3D('',#43543,#23058,#23059);
#20382=AXIS2_PLACEMENT_3D('',#43546,#23061,#23062);
#20383=AXIS2_PLACEMENT_3D('',#43656,#23063,#23064);
#20384=AXIS2_PLACEMENT_3D('',#43657,#23065,#23066);
#20385=AXIS2_PLACEMENT_3D('',#43658,#23067,#23068);
#20386=AXIS2_PLACEMENT_3D('',#43660,#23069,#23070);
#20387=AXIS2_PLACEMENT_3D('',#43666,#23071,#23072);
#20388=AXIS2_PLACEMENT_3D('',#43667,#23073,#23074);
#20389=AXIS2_PLACEMENT_3D('',#43669,#23075,#23076);
#20390=AXIS2_PLACEMENT_3D('',#43674,#23077,#23078);
#20391=AXIS2_PLACEMENT_3D('',#43676,#23079,#23080);
#20392=AXIS2_PLACEMENT_3D('',#43681,#23081,#23082);
#20393=AXIS2_PLACEMENT_3D('',#43683,#23083,#23084);
#20394=AXIS2_PLACEMENT_3D('',#43715,#23085,#23086);
#20395=AXIS2_PLACEMENT_3D('',#43878,#23088,#23089);
#20396=AXIS2_PLACEMENT_3D('',#43881,#23091,#23092);
#20397=AXIS2_PLACEMENT_3D('',#43991,#23093,#23094);
#20398=AXIS2_PLACEMENT_3D('',#43992,#23095,#23096);
#20399=AXIS2_PLACEMENT_3D('',#43993,#23097,#23098);
#20400=AXIS2_PLACEMENT_3D('',#43995,#23099,#23100);
#20401=AXIS2_PLACEMENT_3D('',#44001,#23101,#23102);
#20402=AXIS2_PLACEMENT_3D('',#44002,#23103,#23104);
#20403=AXIS2_PLACEMENT_3D('',#44004,#23105,#23106);
#20404=AXIS2_PLACEMENT_3D('',#44009,#23107,#23108);
#20405=AXIS2_PLACEMENT_3D('',#44011,#23109,#23110);
#20406=AXIS2_PLACEMENT_3D('',#44016,#23111,#23112);
#20407=AXIS2_PLACEMENT_3D('',#44018,#23113,#23114);
#20408=AXIS2_PLACEMENT_3D('',#44050,#23115,#23116);
#20409=AXIS2_PLACEMENT_3D('',#44200,#23118,#23119);
#20410=AXIS2_PLACEMENT_3D('',#44203,#23121,#23122);
#20411=AXIS2_PLACEMENT_3D('',#44313,#23123,#23124);
#20412=AXIS2_PLACEMENT_3D('',#44314,#23125,#23126);
#20413=AXIS2_PLACEMENT_3D('',#44315,#23127,#23128);
#20414=AXIS2_PLACEMENT_3D('',#44317,#23129,#23130);
#20415=AXIS2_PLACEMENT_3D('',#44323,#23131,#23132);
#20416=AXIS2_PLACEMENT_3D('',#44324,#23133,#23134);
#20417=AXIS2_PLACEMENT_3D('',#44326,#23135,#23136);
#20418=AXIS2_PLACEMENT_3D('',#44331,#23137,#23138);
#20419=AXIS2_PLACEMENT_3D('',#44333,#23139,#23140);
#20420=AXIS2_PLACEMENT_3D('',#44338,#23141,#23142);
#20421=AXIS2_PLACEMENT_3D('',#44340,#23143,#23144);
#20422=AXIS2_PLACEMENT_3D('',#44372,#23145,#23146);
#20423=AXIS2_PLACEMENT_3D('',#44522,#23148,#23149);
#20424=AXIS2_PLACEMENT_3D('',#44525,#23151,#23152);
#20425=AXIS2_PLACEMENT_3D('',#44635,#23153,#23154);
#20426=AXIS2_PLACEMENT_3D('',#44636,#23155,#23156);
#20427=AXIS2_PLACEMENT_3D('',#44637,#23157,#23158);
#20428=AXIS2_PLACEMENT_3D('',#44639,#23159,#23160);
#20429=AXIS2_PLACEMENT_3D('',#44645,#23161,#23162);
#20430=AXIS2_PLACEMENT_3D('',#44646,#23163,#23164);
#20431=AXIS2_PLACEMENT_3D('',#44648,#23165,#23166);
#20432=AXIS2_PLACEMENT_3D('',#44653,#23167,#23168);
#20433=AXIS2_PLACEMENT_3D('',#44655,#23169,#23170);
#20434=AXIS2_PLACEMENT_3D('',#44660,#23171,#23172);
#20435=AXIS2_PLACEMENT_3D('',#44663,#23173,#23174);
#20436=AXIS2_PLACEMENT_3D('',#44664,#23175,#23176);
#20437=AXIS2_PLACEMENT_3D('',#44696,#23177,#23178);
#20438=AXIS2_PLACEMENT_3D('',#44848,#23180,#23181);
#20439=AXIS2_PLACEMENT_3D('',#44851,#23183,#23184);
#20440=AXIS2_PLACEMENT_3D('',#44961,#23185,#23186);
#20441=AXIS2_PLACEMENT_3D('',#44963,#23187,#23188);
#20442=AXIS2_PLACEMENT_3D('',#44964,#23189,#23190);
#20443=AXIS2_PLACEMENT_3D('',#44965,#23191,#23192);
#20444=AXIS2_PLACEMENT_3D('',#44967,#23193,#23194);
#20445=AXIS2_PLACEMENT_3D('',#44973,#23195,#23196);
#20446=AXIS2_PLACEMENT_3D('',#44974,#23197,#23198);
#20447=AXIS2_PLACEMENT_3D('',#44976,#23199,#23200);
#20448=AXIS2_PLACEMENT_3D('',#44981,#23201,#23202);
#20449=AXIS2_PLACEMENT_3D('',#44983,#23203,#23204);
#20450=AXIS2_PLACEMENT_3D('',#44988,#23205,#23206);
#20451=AXIS2_PLACEMENT_3D('',#44990,#23207,#23208);
#20452=AXIS2_PLACEMENT_3D('',#45022,#23209,#23210);
#20453=AXIS2_PLACEMENT_3D('',#45172,#23212,#23213);
#20454=AXIS2_PLACEMENT_3D('',#45175,#23215,#23216);
#20455=AXIS2_PLACEMENT_3D('',#45285,#23217,#23218);
#20456=AXIS2_PLACEMENT_3D('',#45286,#23219,#23220);
#20457=AXIS2_PLACEMENT_3D('',#45287,#23221,#23222);
#20458=AXIS2_PLACEMENT_3D('',#45289,#23223,#23224);
#20459=AXIS2_PLACEMENT_3D('',#45295,#23225,#23226);
#20460=AXIS2_PLACEMENT_3D('',#45296,#23227,#23228);
#20461=AXIS2_PLACEMENT_3D('',#45298,#23229,#23230);
#20462=AXIS2_PLACEMENT_3D('',#45303,#23231,#23232);
#20463=AXIS2_PLACEMENT_3D('',#45305,#23233,#23234);
#20464=AXIS2_PLACEMENT_3D('',#45310,#23235,#23236);
#20465=AXIS2_PLACEMENT_3D('',#45312,#23237,#23238);
#20466=AXIS2_PLACEMENT_3D('',#45344,#23239,#23240);
#20467=AXIS2_PLACEMENT_3D('',#45494,#23242,#23243);
#20468=AXIS2_PLACEMENT_3D('',#45497,#23245,#23246);
#20469=AXIS2_PLACEMENT_3D('',#45607,#23247,#23248);
#20470=AXIS2_PLACEMENT_3D('',#45608,#23249,#23250);
#20471=AXIS2_PLACEMENT_3D('',#45609,#23251,#23252);
#20472=AXIS2_PLACEMENT_3D('',#45611,#23253,#23254);
#20473=AXIS2_PLACEMENT_3D('',#45617,#23255,#23256);
#20474=AXIS2_PLACEMENT_3D('',#45618,#23257,#23258);
#20475=AXIS2_PLACEMENT_3D('',#45620,#23259,#23260);
#20476=AXIS2_PLACEMENT_3D('',#45625,#23261,#23262);
#20477=AXIS2_PLACEMENT_3D('',#45627,#23263,#23264);
#20478=AXIS2_PLACEMENT_3D('',#45632,#23265,#23266);
#20479=AXIS2_PLACEMENT_3D('',#45634,#23267,#23268);
#20480=AXIS2_PLACEMENT_3D('',#45666,#23269,#23270);
#20481=AXIS2_PLACEMENT_3D('',#45816,#23272,#23273);
#20482=AXIS2_PLACEMENT_3D('',#45819,#23275,#23276);
#20483=AXIS2_PLACEMENT_3D('',#45929,#23277,#23278);
#20484=AXIS2_PLACEMENT_3D('',#45930,#23279,#23280);
#20485=AXIS2_PLACEMENT_3D('',#45931,#23281,#23282);
#20486=AXIS2_PLACEMENT_3D('',#45933,#23283,#23284);
#20487=AXIS2_PLACEMENT_3D('',#45942,#23285,#23286);
#20488=AXIS2_PLACEMENT_3D('',#45943,#23287,#23288);
#20489=AXIS2_PLACEMENT_3D('',#45945,#23289,#23290);
#20490=AXIS2_PLACEMENT_3D('',#45950,#23291,#23292);
#20491=AXIS2_PLACEMENT_3D('',#45952,#23293,#23294);
#20492=AXIS2_PLACEMENT_3D('',#45960,#23295,#23296);
#20493=AXIS2_PLACEMENT_3D('',#45962,#23297,#23298);
#20494=AXIS2_PLACEMENT_3D('',#45994,#23299,#23300);
#20495=AXIS2_PLACEMENT_3D('',#46144,#23302,#23303);
#20496=AXIS2_PLACEMENT_3D('',#46147,#23305,#23306);
#20497=AXIS2_PLACEMENT_3D('',#46257,#23307,#23308);
#20498=AXIS2_PLACEMENT_3D('',#46258,#23309,#23310);
#20499=AXIS2_PLACEMENT_3D('',#46259,#23311,#23312);
#20500=AXIS2_PLACEMENT_3D('',#46261,#23313,#23314);
#20501=AXIS2_PLACEMENT_3D('',#46267,#23315,#23316);
#20502=AXIS2_PLACEMENT_3D('',#46268,#23317,#23318);
#20503=AXIS2_PLACEMENT_3D('',#46270,#23319,#23320);
#20504=AXIS2_PLACEMENT_3D('',#46275,#23321,#23322);
#20505=AXIS2_PLACEMENT_3D('',#46277,#23323,#23324);
#20506=AXIS2_PLACEMENT_3D('',#46282,#23325,#23326);
#20507=AXIS2_PLACEMENT_3D('',#46284,#23327,#23328);
#20508=AXIS2_PLACEMENT_3D('',#46316,#23329,#23330);
#20509=AXIS2_PLACEMENT_3D('',#46466,#23332,#23333);
#20510=AXIS2_PLACEMENT_3D('',#46469,#23335,#23336);
#20511=AXIS2_PLACEMENT_3D('',#46579,#23337,#23338);
#20512=AXIS2_PLACEMENT_3D('',#46580,#23339,#23340);
#20513=AXIS2_PLACEMENT_3D('',#46581,#23341,#23342);
#20514=AXIS2_PLACEMENT_3D('',#46583,#23343,#23344);
#20515=AXIS2_PLACEMENT_3D('',#46589,#23345,#23346);
#20516=AXIS2_PLACEMENT_3D('',#46590,#23347,#23348);
#20517=AXIS2_PLACEMENT_3D('',#46592,#23349,#23350);
#20518=AXIS2_PLACEMENT_3D('',#46597,#23351,#23352);
#20519=AXIS2_PLACEMENT_3D('',#46599,#23353,#23354);
#20520=AXIS2_PLACEMENT_3D('',#46604,#23355,#23356);
#20521=AXIS2_PLACEMENT_3D('',#46606,#23357,#23358);
#20522=AXIS2_PLACEMENT_3D('',#46638,#23359,#23360);
#20523=AXIS2_PLACEMENT_3D('',#46788,#23362,#23363);
#20524=AXIS2_PLACEMENT_3D('',#46791,#23365,#23366);
#20525=AXIS2_PLACEMENT_3D('',#46901,#23367,#23368);
#20526=AXIS2_PLACEMENT_3D('',#46902,#23369,#23370);
#20527=AXIS2_PLACEMENT_3D('',#46903,#23371,#23372);
#20528=AXIS2_PLACEMENT_3D('',#46905,#23373,#23374);
#20529=AXIS2_PLACEMENT_3D('',#46911,#23375,#23376);
#20530=AXIS2_PLACEMENT_3D('',#46912,#23377,#23378);
#20531=AXIS2_PLACEMENT_3D('',#46914,#23379,#23380);
#20532=AXIS2_PLACEMENT_3D('',#46919,#23381,#23382);
#20533=AXIS2_PLACEMENT_3D('',#46921,#23383,#23384);
#20534=AXIS2_PLACEMENT_3D('',#47067,#23386,#23387);
#20535=AXIS2_PLACEMENT_3D('',#47068,#23388,#23389);
#20536=AXIS2_PLACEMENT_3D('',#47070,#23390,#23391);
#20537=AXIS2_PLACEMENT_3D('',#47096,#23392,#23393);
#20538=AXIS2_PLACEMENT_3D('',#47098,#23394,#23395);
#20539=AXIS2_PLACEMENT_3D('',#47217,#23397,#23398);
#20540=AXIS2_PLACEMENT_3D('',#47218,#23399,#23400);
#20541=AXIS2_PLACEMENT_3D('',#47219,#23401,#23402);
#20542=AXIS2_PLACEMENT_3D('',#47220,#23403,#23404);
#20543=AXIS2_PLACEMENT_3D('',#47221,#23405,#23406);
#20544=AXIS2_PLACEMENT_3D('',#47222,#23407,#23408);
#20545=AXIS2_PLACEMENT_3D('',#47223,#23409,#23410);
#20546=AXIS2_PLACEMENT_3D('',#47225,#23411,#23412);
#20547=AXIS2_PLACEMENT_3D('',#47226,#23413,#23414);
#20548=AXIS2_PLACEMENT_3D('',#47228,#23416,#23417);
#20549=AXIS2_PLACEMENT_3D('',#47230,#23419,#23420);
#20550=AXIS2_PLACEMENT_3D('',#47232,#23422,#23423);
#20551=AXIS2_PLACEMENT_3D('',#47233,#23424,#23425);
#20552=AXIS2_PLACEMENT_3D('',#47234,#23426,#23427);
#20553=AXIS2_PLACEMENT_3D('',#47236,#23428,#23429);
#20554=AXIS2_PLACEMENT_3D('',#47238,#23431,#23432);
#20555=AXIS2_PLACEMENT_3D('',#47239,#23433,#23434);
#20556=AXIS2_PLACEMENT_3D('',#47240,#23435,#23436);
#20557=AXIS2_PLACEMENT_3D('',#47243,#23437,#23438);
#20558=AXIS2_PLACEMENT_3D('',#47247,#23440,#23441);
#20559=AXIS2_PLACEMENT_3D('',#47249,#23443,#23444);
#20560=AXIS2_PLACEMENT_3D('',#47252,#23445,#23446);
#20561=AXIS2_PLACEMENT_3D('',#47253,#23447,#23448);
#20562=AXIS2_PLACEMENT_3D('',#47254,#23449,#23450);
#20563=AXIS2_PLACEMENT_3D('',#47255,#23451,#23452);
#20564=AXIS2_PLACEMENT_3D('',#47258,#23453,#23454);
#20565=AXIS2_PLACEMENT_3D('',#47261,#23456,#23457);
#20566=AXIS2_PLACEMENT_3D('',#47263,#23459,#23460);
#20567=AXIS2_PLACEMENT_3D('',#47266,#23461,#23462);
#20568=AXIS2_PLACEMENT_3D('',#47269,#23464,#23465);
#20569=AXIS2_PLACEMENT_3D('',#47271,#23467,#23468);
#20570=AXIS2_PLACEMENT_3D('',#47272,#23469,#23470);
#20571=AXIS2_PLACEMENT_3D('',#47273,#23471,#23472);
#20572=AXIS2_PLACEMENT_3D('',#47276,#23473,#23474);
#20573=AXIS2_PLACEMENT_3D('',#47278,#23475,#23476);
#20574=AXIS2_PLACEMENT_3D('',#47280,#23477,#23478);
#20575=AXIS2_PLACEMENT_3D('',#47281,#23479,#23480);
#20576=AXIS2_PLACEMENT_3D('',#47282,#23481,#23482);
#20577=AXIS2_PLACEMENT_3D('',#47285,#23483,#23484);
#20578=AXIS2_PLACEMENT_3D('',#47288,#23487,#23488);
#20579=AXIS2_PLACEMENT_3D('',#47290,#23489,#23490);
#20580=AXIS2_PLACEMENT_3D('',#47293,#23492,#23493);
#20581=AXIS2_PLACEMENT_3D('',#47295,#23495,#23496);
#20582=AXIS2_PLACEMENT_3D('',#47296,#23497,#23498);
#20583=AXIS2_PLACEMENT_3D('',#47297,#23499,#23500);
#20584=AXIS2_PLACEMENT_3D('',#47301,#23502,#23503);
#20585=AXIS2_PLACEMENT_3D('',#47303,#23505,#23506);
#20586=AXIS2_PLACEMENT_3D('',#47305,#23508,#23509);
#20587=AXIS2_PLACEMENT_3D('',#47308,#23511,#23512);
#20588=AXIS2_PLACEMENT_3D('',#47309,#23513,#23514);
#20589=AXIS2_PLACEMENT_3D('',#47313,#23517,#23518);
#20590=AXIS2_PLACEMENT_3D('',#47316,#23520,#23521);
#20591=AXIS2_PLACEMENT_3D('',#47317,#23522,#23523);
#20592=AXIS2_PLACEMENT_3D('',#47319,#23525,#23526);
#20593=AXIS2_PLACEMENT_3D('',#47322,#23529,#23530);
#20594=AXIS2_PLACEMENT_3D('',#47325,#23532,#23533);
#20595=AXIS2_PLACEMENT_3D('',#47326,#23534,#23535);
#20596=AXIS2_PLACEMENT_3D('',#47327,#23536,#23537);
#20597=AXIS2_PLACEMENT_3D('',#47328,#23538,#23539);
#20598=AXIS2_PLACEMENT_3D('',#47330,#23541,#23542);
#20599=AXIS2_PLACEMENT_3D('',#47331,#23543,#23544);
#20600=AXIS2_PLACEMENT_3D('',#47332,#23545,#23546);
#20601=AXIS2_PLACEMENT_3D('',#47334,#23548,#23549);
#20602=AXIS2_PLACEMENT_3D('',#47344,#23550,#23551);
#20603=AXIS2_PLACEMENT_3D('',#47346,#23552,#23553);
#20604=AXIS2_PLACEMENT_3D('',#47349,#23555,#23556);
#20605=AXIS2_PLACEMENT_3D('',#47351,#23558,#23559);
#20606=AXIS2_PLACEMENT_3D('',#47352,#23560,#23561);
#20607=AXIS2_PLACEMENT_3D('',#47353,#23562,#23563);
#20608=AXIS2_PLACEMENT_3D('',#47357,#23565,#23566);
#20609=AXIS2_PLACEMENT_3D('',#47360,#23568,#23569);
#20610=AXIS2_PLACEMENT_3D('',#47361,#23570,#23571);
#20611=AXIS2_PLACEMENT_3D('',#47364,#23573,#23574);
#20612=AXIS2_PLACEMENT_3D('',#47365,#23575,#23576);
#20613=AXIS2_PLACEMENT_3D('',#47366,#23577,#23578);
#20614=AXIS2_PLACEMENT_3D('',#47367,#23579,#23580);
#20615=AXIS2_PLACEMENT_3D('',#47371,#23582,#23583);
#20616=AXIS2_PLACEMENT_3D('',#47373,#23585,#23586);
#20617=AXIS2_PLACEMENT_3D('',#47379,#23590,#23591);
#20618=AXIS2_PLACEMENT_3D('',#47382,#23592,#23593);
#20619=AXIS2_PLACEMENT_3D('',#47383,#23594,#23595);
#20620=AXIS2_PLACEMENT_3D('',#47385,#23596,#23597);
#20621=AXIS2_PLACEMENT_3D('',#47386,#23598,#23599);
#20622=AXIS2_PLACEMENT_3D('',#47387,#23600,#23601);
#20623=AXIS2_PLACEMENT_3D('',#47389,#23603,#23604);
#20624=AXIS2_PLACEMENT_3D('',#47404,#23606,#23607);
#20625=AXIS2_PLACEMENT_3D('',#47405,#23608,#23609);
#20626=AXIS2_PLACEMENT_3D('',#47409,#23611,#23612);
#20627=AXIS2_PLACEMENT_3D('',#47411,#23614,#23615);
#20628=AXIS2_PLACEMENT_3D('',#47415,#23617,#23618);
#20629=AXIS2_PLACEMENT_3D('',#47417,#23620,#23621);
#20630=AXIS2_PLACEMENT_3D('',#47419,#23622,#23623);
#20631=AXIS2_PLACEMENT_3D('',#47422,#23626,#23627);
#20632=AXIS2_PLACEMENT_3D('',#47423,#23628,#23629);
#20633=AXIS2_PLACEMENT_3D('',#47424,#23630,#23631);
#20634=AXIS2_PLACEMENT_3D('',#47428,#23634,#23635);
#20635=AXIS2_PLACEMENT_3D('',#47431,#23637,#23638);
#20636=AXIS2_PLACEMENT_3D('',#47432,#23639,#23640);
#20637=AXIS2_PLACEMENT_3D('',#47434,#23642,#23643);
#20638=AXIS2_PLACEMENT_3D('',#47435,#23644,#23645);
#20639=AXIS2_PLACEMENT_3D('',#47439,#23647,#23648);
#20640=AXIS2_PLACEMENT_3D('',#47441,#23650,#23651);
#20641=AXIS2_PLACEMENT_3D('',#47449,#23656,#23657);
#20642=AXIS2_PLACEMENT_3D('',#47451,#23658,#23659);
#20643=AXIS2_PLACEMENT_3D('',#47453,#23660,#23661);
#20644=AXIS2_PLACEMENT_3D('',#47460,#23662,#23663);
#20645=AXIS2_PLACEMENT_3D('',#47462,#23664,#23665);
#20646=AXIS2_PLACEMENT_3D('',#47464,#23667,#23668);
#20647=AXIS2_PLACEMENT_3D('',#47465,#23669,#23670);
#20648=AXIS2_PLACEMENT_3D('',#47466,#23671,#23672);
#20649=AXIS2_PLACEMENT_3D('',#47468,#23673,#23674);
#20650=AXIS2_PLACEMENT_3D('',#47470,#23676,#23677);
#20651=AXIS2_PLACEMENT_3D('',#47484,#23680,#23681);
#20652=AXIS2_PLACEMENT_3D('',#47485,#23682,#23683);
#20653=AXIS2_PLACEMENT_3D('',#47486,#23684,#23685);
#20654=AXIS2_PLACEMENT_3D('',#47488,#23687,#23688);
#20655=AXIS2_PLACEMENT_3D('',#47489,#23689,#23690);
#20656=AXIS2_PLACEMENT_3D('',#47490,#23691,#23692);
#20657=AXIS2_PLACEMENT_3D('',#47492,#23693,#23694);
#20658=AXIS2_PLACEMENT_3D('',#47504,#23695,#23696);
#20659=AXIS2_PLACEMENT_3D('',#47505,#23697,#23698);
#20660=AXIS2_PLACEMENT_3D('',#47508,#23699,#23700);
#20661=AXIS2_PLACEMENT_3D('',#47512,#23702,#23703);
#20662=AXIS2_PLACEMENT_3D('',#47514,#23705,#23706);
#20663=AXIS2_PLACEMENT_3D('',#47516,#23707,#23708);
#20664=AXIS2_PLACEMENT_3D('',#47520,#23710,#23711);
#20665=AXIS2_PLACEMENT_3D('',#47522,#23713,#23714);
#20666=AXIS2_PLACEMENT_3D('',#47525,#23715,#23716);
#20667=AXIS2_PLACEMENT_3D('',#47526,#23717,#23718);
#20668=AXIS2_PLACEMENT_3D('',#47527,#23719,#23720);
#20669=AXIS2_PLACEMENT_3D('',#47528,#23721,#23722);
#20670=AXIS2_PLACEMENT_3D('',#47534,#23726,#23727);
#20671=AXIS2_PLACEMENT_3D('',#47540,#23731,#23732);
#20672=AXIS2_PLACEMENT_3D('',#47542,#23733,#23734);
#20673=AXIS2_PLACEMENT_3D('',#47544,#23735,#23736);
#20674=AXIS2_PLACEMENT_3D('',#47546,#23738,#23739);
#20675=AXIS2_PLACEMENT_3D('',#47547,#23740,#23741);
#20676=AXIS2_PLACEMENT_3D('',#47548,#23742,#23743);
#20677=AXIS2_PLACEMENT_3D('',#47550,#23744,#23745);
#20678=AXIS2_PLACEMENT_3D('',#47553,#23747,#23748);
#20679=AXIS2_PLACEMENT_3D('',#47554,#23749,#23750);
#20680=AXIS2_PLACEMENT_3D('',#47555,#23751,#23752);
#20681=AXIS2_PLACEMENT_3D('',#47556,#23753,#23754);
#20682=AXIS2_PLACEMENT_3D('',#47559,#23756,#23757);
#20683=AXIS2_PLACEMENT_3D('',#47560,#23758,#23759);
#20684=AXIS2_PLACEMENT_3D('',#47561,#23760,#23761);
#20685=AXIS2_PLACEMENT_3D('',#47562,#23762,#23763);
#20686=AXIS2_PLACEMENT_3D('',#47565,#23765,#23766);
#20687=AXIS2_PLACEMENT_3D('',#47566,#23767,#23768);
#20688=AXIS2_PLACEMENT_3D('',#47570,#23771,#23772);
#20689=AXIS2_PLACEMENT_3D('',#47573,#23774,#23775);
#20690=AXIS2_PLACEMENT_3D('',#47574,#23776,#23777);
#20691=AXIS2_PLACEMENT_3D('',#47578,#23780,#23781);
#20692=AXIS2_PLACEMENT_3D('',#47581,#23783,#23784);
#20693=AXIS2_PLACEMENT_3D('',#47582,#23785,#23786);
#20694=AXIS2_PLACEMENT_3D('',#47586,#23789,#23790);
#20695=AXIS2_PLACEMENT_3D('',#47589,#23792,#23793);
#20696=AXIS2_PLACEMENT_3D('',#47590,#23794,#23795);
#20697=AXIS2_PLACEMENT_3D('',#47593,#23796,#23797);
#20698=AXIS2_PLACEMENT_3D('',#47597,#23799,#23800);
#20699=AXIS2_PLACEMENT_3D('',#47599,#23802,#23803);
#20700=AXIS2_PLACEMENT_3D('',#47615,#23805,#23806);
#20701=AXIS2_PLACEMENT_3D('',#47618,#23808,#23809);
#20702=AXIS2_PLACEMENT_3D('',#47619,#23810,#23811);
#20703=AXIS2_PLACEMENT_3D('',#47620,#23812,#23813);
#20704=AXIS2_PLACEMENT_3D('',#47621,#23814,#23815);
#20705=AXIS2_PLACEMENT_3D('',#47627,#23819,#23820);
#20706=AXIS2_PLACEMENT_3D('',#47630,#23822,#23823);
#20707=AXIS2_PLACEMENT_3D('',#47631,#23824,#23825);
#20708=AXIS2_PLACEMENT_3D('',#47645,#23828,#23829);
#20709=AXIS2_PLACEMENT_3D('',#47647,#23830,#23831);
#20710=AXIS2_PLACEMENT_3D('',#47648,#23832,#23833);
#20711=AXIS2_PLACEMENT_3D('',#47649,#23834,#23835);
#20712=AXIS2_PLACEMENT_3D('',#47652,#23838,#23839);
#20713=AXIS2_PLACEMENT_3D('',#47666,#23840,#23841);
#20714=AXIS2_PLACEMENT_3D('',#47668,#23843,#23844);
#20715=AXIS2_PLACEMENT_3D('',#47671,#23846,#23847);
#20716=AXIS2_PLACEMENT_3D('',#47672,#23848,#23849);
#20717=AXIS2_PLACEMENT_3D('',#47674,#23850,#23851);
#20718=AXIS2_PLACEMENT_3D('',#47676,#23852,#23853);
#20719=AXIS2_PLACEMENT_3D('',#47678,#23855,#23856);
#20720=AXIS2_PLACEMENT_3D('',#47680,#23857,#23858);
#20721=AXIS2_PLACEMENT_3D('',#47681,#23859,#23860);
#20722=AXIS2_PLACEMENT_3D('',#47683,#23862,#23863);
#20723=AXIS2_PLACEMENT_3D('',#47684,#23864,#23865);
#20724=AXIS2_PLACEMENT_3D('',#47685,#23866,#23867);
#20725=AXIS2_PLACEMENT_3D('',#47687,#23868,#23869);
#20726=AXIS2_PLACEMENT_3D('',#47689,#23871,#23872);
#20727=AXIS2_PLACEMENT_3D('',#47690,#23873,#23874);
#20728=AXIS2_PLACEMENT_3D('',#47692,#23876,#23877);
#20729=AXIS2_PLACEMENT_3D('',#47695,#23880,#23881);
#20730=AXIS2_PLACEMENT_3D('',#47696,#23882,#23883);
#20731=AXIS2_PLACEMENT_3D('',#47698,#23884,#23885);
#20732=AXIS2_PLACEMENT_3D('',#47700,#23887,#23888);
#20733=AXIS2_PLACEMENT_3D('',#47701,#23889,#23890);
#20734=AXIS2_PLACEMENT_3D('',#47702,#23891,#23892);
#20735=AXIS2_PLACEMENT_3D('',#47705,#23894,#23895);
#20736=AXIS2_PLACEMENT_3D('',#47706,#23896,#23897);
#20737=AXIS2_PLACEMENT_3D('',#47710,#23900,#23901);
#20738=AXIS2_PLACEMENT_3D('',#47711,#23902,#23903);
#20739=AXIS2_PLACEMENT_3D('',#47712,#23904,#23905);
#20740=AXIS2_PLACEMENT_3D('',#47713,#23906,#23907);
#20741=AXIS2_PLACEMENT_3D('',#47714,#23908,#23909);
#20742=AXIS2_PLACEMENT_3D('',#47728,#23911,#23912);
#20743=AXIS2_PLACEMENT_3D('',#47731,#23914,#23915);
#20744=AXIS2_PLACEMENT_3D('',#47732,#23916,#23917);
#20745=AXIS2_PLACEMENT_3D('',#47735,#23918,#23919);
#20746=AXIS2_PLACEMENT_3D('',#47738,#23921,#23922);
#20747=AXIS2_PLACEMENT_3D('',#47741,#23924,#23925);
#20748=AXIS2_PLACEMENT_3D('',#47742,#23926,#23927);
#20749=AXIS2_PLACEMENT_3D('',#47743,#23928,#23929);
#20750=AXIS2_PLACEMENT_3D('',#47744,#23930,#23931);
#20751=AXIS2_PLACEMENT_3D('',#47750,#23935,#23936);
#20752=AXIS2_PLACEMENT_3D('',#47754,#23938,#23939);
#20753=AXIS2_PLACEMENT_3D('',#47755,#23940,#23941);
#20754=AXIS2_PLACEMENT_3D('',#47756,#23942,#23943);
#20755=AXIS2_PLACEMENT_3D('',#47760,#23946,#23947);
#20756=AXIS2_PLACEMENT_3D('',#47762,#23948,#23949);
#20757=AXIS2_PLACEMENT_3D('',#47765,#23951,#23952);
#20758=AXIS2_PLACEMENT_3D('',#47766,#23953,#23954);
#20759=AXIS2_PLACEMENT_3D('',#47768,#23955,#23956);
#20760=AXIS2_PLACEMENT_3D('',#47772,#23958,#23959);
#20761=AXIS2_PLACEMENT_3D('',#47774,#23961,#23962);
#20762=AXIS2_PLACEMENT_3D('',#47777,#23963,#23964);
#20763=AXIS2_PLACEMENT_3D('',#47781,#23966,#23967);
#20764=AXIS2_PLACEMENT_3D('',#47783,#23969,#23970);
#20765=AXIS2_PLACEMENT_3D('',#47786,#23971,#23972);
#20766=AXIS2_PLACEMENT_3D('',#47787,#23973,#23974);
#20767=AXIS2_PLACEMENT_3D('',#47788,#23975,#23976);
#20768=AXIS2_PLACEMENT_3D('',#47789,#23977,#23978);
#20769=AXIS2_PLACEMENT_3D('',#47792,#23979,#23980);
#20770=AXIS2_PLACEMENT_3D('',#47793,#23981,#23982);
#20771=AXIS2_PLACEMENT_3D('',#47794,#23983,#23984);
#20772=AXIS2_PLACEMENT_3D('',#47795,#23985,#23986);
#20773=AXIS2_PLACEMENT_3D('',#47799,#23988,#23989);
#20774=AXIS2_PLACEMENT_3D('',#47801,#23991,#23992);
#20775=AXIS2_PLACEMENT_3D('',#47805,#23994,#23995);
#20776=AXIS2_PLACEMENT_3D('',#47807,#23997,#23998);
#20777=AXIS2_PLACEMENT_3D('',#47811,#24000,#24001);
#20778=AXIS2_PLACEMENT_3D('',#47813,#24003,#24004);
#20779=AXIS2_PLACEMENT_3D('',#47817,#24007,#24008);
#20780=AXIS2_PLACEMENT_3D('',#47820,#24010,#24011);
#20781=AXIS2_PLACEMENT_3D('',#47821,#24012,#24013);
#20782=AXIS2_PLACEMENT_3D('',#47824,#24014,#24015);
#20783=AXIS2_PLACEMENT_3D('',#47827,#24017,#24018);
#20784=AXIS2_PLACEMENT_3D('',#47829,#24020,#24021);
#20785=AXIS2_PLACEMENT_3D('',#47831,#24022,#24023);
#20786=AXIS2_PLACEMENT_3D('',#47832,#24024,#24025);
#20787=AXIS2_PLACEMENT_3D('',#47833,#24026,#24027);
#20788=AXIS2_PLACEMENT_3D('',#47834,#24028,#24029);
#20789=AXIS2_PLACEMENT_3D('',#47835,#24030,#24031);
#20790=AXIS2_PLACEMENT_3D('',#47838,#24032,#24033);
#20791=AXIS2_PLACEMENT_3D('',#47842,#24036,#24037);
#20792=AXIS2_PLACEMENT_3D('',#47843,#24038,#24039);
#20793=AXIS2_PLACEMENT_3D('',#47846,#24041,#24042);
#20794=AXIS2_PLACEMENT_3D('',#47847,#24043,#24044);
#20795=AXIS2_PLACEMENT_3D('',#47851,#24047,#24048);
#20796=AXIS2_PLACEMENT_3D('',#47854,#24050,#24051);
#20797=AXIS2_PLACEMENT_3D('',#47855,#24052,#24053);
#20798=AXIS2_PLACEMENT_3D('',#47859,#24056,#24057);
#20799=AXIS2_PLACEMENT_3D('',#47861,#24058,#24059);
#20800=AXIS2_PLACEMENT_3D('',#47862,#24060,#24061);
#20801=AXIS2_PLACEMENT_3D('',#47863,#24062,#24063);
#20802=AXIS2_PLACEMENT_3D('',#47866,#24066,#24067);
#20803=AXIS2_PLACEMENT_3D('',#47867,#24068,#24069);
#20804=AXIS2_PLACEMENT_3D('',#47871,#24071,#24072);
#20805=AXIS2_PLACEMENT_3D('',#47873,#24074,#24075);
#20806=AXIS2_PLACEMENT_3D('',#47875,#24077,#24078);
#20807=AXIS2_PLACEMENT_3D('',#47877,#24079,#24080);
#20808=AXIS2_PLACEMENT_3D('',#47880,#24082,#24083);
#20809=AXIS2_PLACEMENT_3D('',#47882,#24085,#24086);
#20810=AXIS2_PLACEMENT_3D('',#47883,#24087,#24088);
#20811=AXIS2_PLACEMENT_3D('',#47884,#24089,#24090);
#20812=AXIS2_PLACEMENT_3D('',#47887,#24092,#24093);
#20813=AXIS2_PLACEMENT_3D('',#47888,#24094,#24095);
#20814=AXIS2_PLACEMENT_3D('',#47890,#24096,#24097);
#20815=AXIS2_PLACEMENT_3D('',#47892,#24099,#24100);
#20816=AXIS2_PLACEMENT_3D('',#47895,#24103,#24104);
#20817=AXIS2_PLACEMENT_3D('',#47896,#24105,#24106);
#20818=AXIS2_PLACEMENT_3D('',#47899,#24107,#24108);
#20819=AXIS2_PLACEMENT_3D('',#47903,#24110,#24111);
#20820=AXIS2_PLACEMENT_3D('',#47905,#24113,#24114);
#20821=AXIS2_PLACEMENT_3D('',#47910,#24118,#24119);
#20822=AXIS2_PLACEMENT_3D('',#47912,#24120,#24121);
#20823=AXIS2_PLACEMENT_3D('',#47917,#24122,#24123);
#20824=AXIS2_PLACEMENT_3D('',#47918,#24124,#24125);
#20825=AXIS2_PLACEMENT_3D('',#47919,#24126,#24127);
#20826=AXIS2_PLACEMENT_3D('',#47920,#24128,#24129);
#20827=AXIS2_PLACEMENT_3D('',#47931,#24131,#24132);
#20828=AXIS2_PLACEMENT_3D('',#47932,#24133,#24134);
#20829=AXIS2_PLACEMENT_3D('',#47933,#24135,#24136);
#20830=AXIS2_PLACEMENT_3D('',#47948,#24138,#24139);
#20831=AXIS2_PLACEMENT_3D('',#47949,#24140,#24141);
#20832=AXIS2_PLACEMENT_3D('',#47950,#24142,#24143);
#20833=AXIS2_PLACEMENT_3D('',#47951,#24144,#24145);
#20834=AXIS2_PLACEMENT_3D('',#47953,#24146,#24147);
#20835=AXIS2_PLACEMENT_3D('',#47954,#24148,#24149);
#20836=AXIS2_PLACEMENT_3D('',#47956,#24151,#24152);
#20837=AXIS2_PLACEMENT_3D('',#47957,#24153,#24154);
#20838=AXIS2_PLACEMENT_3D('',#47958,#24155,#24156);
#20839=AXIS2_PLACEMENT_3D('',#47959,#24157,#24158);
#20840=AXIS2_PLACEMENT_3D('',#47960,#24159,#24160);
#20841=AXIS2_PLACEMENT_3D('',#47962,#24162,#24163);
#20842=AXIS2_PLACEMENT_3D('',#47963,#24164,#24165);
#20843=AXIS2_PLACEMENT_3D('',#47964,#24166,#24167);
#20844=AXIS2_PLACEMENT_3D('',#47967,#24168,#24169);
#20845=AXIS2_PLACEMENT_3D('',#47969,#24170,#24171);
#20846=AXIS2_PLACEMENT_3D('',#47970,#24172,#24173);
#20847=AXIS2_PLACEMENT_3D('',#47971,#24174,#24175);
#20848=AXIS2_PLACEMENT_3D('',#47972,#24176,#24177);
#20849=AXIS2_PLACEMENT_3D('',#47976,#24179,#24180);
#20850=AXIS2_PLACEMENT_3D('',#47980,#24182,#24183);
#20851=AXIS2_PLACEMENT_3D('',#47984,#24185,#24186);
#20852=AXIS2_PLACEMENT_3D('',#47988,#24188,#24189);
#20853=AXIS2_PLACEMENT_3D('',#47992,#24191,#24192);
#20854=AXIS2_PLACEMENT_3D('',#47996,#24194,#24195);
#20855=AXIS2_PLACEMENT_3D('',#48000,#24197,#24198);
#20856=AXIS2_PLACEMENT_3D('',#48004,#24200,#24201);
#20857=AXIS2_PLACEMENT_3D('',#48007,#24203,#24204);
#20858=AXIS2_PLACEMENT_3D('',#48008,#24205,#24206);
#20859=AXIS2_PLACEMENT_3D('',#48010,#24207,#24208);
#20860=AXIS2_PLACEMENT_3D('',#48011,#24209,#24210);
#20861=AXIS2_PLACEMENT_3D('',#48027,#24212,#24213);
#20862=AXIS2_PLACEMENT_3D('',#48040,#24215,#24216);
#20863=AXIS2_PLACEMENT_3D('',#48043,#24217,#24218);
#20864=AXIS2_PLACEMENT_3D('',#48044,#24219,#24220);
#20865=AXIS2_PLACEMENT_3D('',#48045,#24221,#24222);
#20866=AXIS2_PLACEMENT_3D('',#48046,#24223,#24224);
#20867=AXIS2_PLACEMENT_3D('',#48049,#24225,#24226);
#20868=AXIS2_PLACEMENT_3D('',#48052,#24229,#24230);
#20869=AXIS2_PLACEMENT_3D('',#48054,#24231,#24232);
#20870=AXIS2_PLACEMENT_3D('',#48055,#24233,#24234);
#20871=AXIS2_PLACEMENT_3D('',#48056,#24235,#24236);
#20872=AXIS2_PLACEMENT_3D('',#48059,#24237,#24238);
#20873=AXIS2_PLACEMENT_3D('',#48061,#24239,#24240);
#20874=AXIS2_PLACEMENT_3D('',#48063,#24241,#24242);
#20875=AXIS2_PLACEMENT_3D('',#48064,#24243,#24244);
#20876=AXIS2_PLACEMENT_3D('',#48065,#24245,#24246);
#20877=AXIS2_PLACEMENT_3D('',#48102,#24247,#24248);
#20878=AXIS2_PLACEMENT_3D('',#48104,#24249,#24250);
#20879=AXIS2_PLACEMENT_3D('',#48108,#24252,#24253);
#20880=AXIS2_PLACEMENT_3D('',#48112,#24255,#24256);
#20881=AXIS2_PLACEMENT_3D('',#48116,#24258,#24259);
#20882=AXIS2_PLACEMENT_3D('',#48120,#24261,#24262);
#20883=AXIS2_PLACEMENT_3D('',#48124,#24264,#24265);
#20884=AXIS2_PLACEMENT_3D('',#48127,#24267,#24268);
#20885=AXIS2_PLACEMENT_3D('',#48129,#24269,#24270);
#20886=AXIS2_PLACEMENT_3D('',#48130,#24271,#24272);
#20887=AXIS2_PLACEMENT_3D('',#48132,#24273,#24274);
#20888=AXIS2_PLACEMENT_3D('',#48133,#24275,#24276);
#20889=AXIS2_PLACEMENT_3D('',#48134,#24277,#24278);
#20890=AXIS2_PLACEMENT_3D('',#48136,#24279,#24280);
#20891=AXIS2_PLACEMENT_3D('',#48141,#24281,#24282);
#20892=AXIS2_PLACEMENT_3D('',#48142,#24283,#24284);
#20893=AXIS2_PLACEMENT_3D('',#48143,#24285,#24286);
#20894=AXIS2_PLACEMENT_3D('',#48147,#24288,#24289);
#20895=AXIS2_PLACEMENT_3D('',#48162,#24290,#24291);
#20896=AXIS2_PLACEMENT_3D('',#48177,#24293,#24294);
#20897=AXIS2_PLACEMENT_3D('',#48188,#24295,#24296);
#20898=AXIS2_PLACEMENT_3D('',#48190,#24297,#24298);
#20899=AXIS2_PLACEMENT_3D('',#48191,#24299,#24300);
#20900=AXIS2_PLACEMENT_3D('',#48192,#24301,#24302);
#20901=AXIS2_PLACEMENT_3D('',#48202,#24304,#24305);
#20902=AXIS2_PLACEMENT_3D('',#48203,#24306,#24307);
#20903=AXIS2_PLACEMENT_3D('',#48205,#24308,#24309);
#20904=AXIS2_PLACEMENT_3D('',#48206,#24310,#24311);
#20905=AXIS2_PLACEMENT_3D('',#48207,#24312,#24313);
#20906=AXIS2_PLACEMENT_3D('',#48213,#24314,#24315);
#20907=AXIS2_PLACEMENT_3D('',#48214,#24316,#24317);
#20908=AXIS2_PLACEMENT_3D('',#48236,#24321,#24322);
#20909=AXIS2_PLACEMENT_3D('',#48248,#24323,#24324);
#20910=AXIS2_PLACEMENT_3D('',#48249,#24325,#24326);
#20911=AXIS2_PLACEMENT_3D('',#48253,#24328,#24329);
#20912=AXIS2_PLACEMENT_3D('',#48308,#24330,#24331);
#20913=AXIS2_PLACEMENT_3D('',#48314,#24332,#24333);
#20914=AXIS2_PLACEMENT_3D('',#48319,#24334,#24335);
#20915=AXIS2_PLACEMENT_3D('',#48320,#24336,#24337);
#20916=AXIS2_PLACEMENT_3D('',#48321,#24338,#24339);
#20917=AXIS2_PLACEMENT_3D('',#48338,#24340,#24341);
#20918=AXIS2_PLACEMENT_3D('',#48339,#24342,#24343);
#20919=AXIS2_PLACEMENT_3D('',#48342,#24345,#24346);
#20920=AXIS2_PLACEMENT_3D('',#48343,#24347,#24348);
#20921=AXIS2_PLACEMENT_3D('',#48344,#24349,#24350);
#20922=AXIS2_PLACEMENT_3D('',#48346,#24351,#24352);
#20923=AXIS2_PLACEMENT_3D('',#48347,#24353,#24354);
#20924=AXIS2_PLACEMENT_3D('',#48369,#24358,#24359);
#20925=AXIS2_PLACEMENT_3D('',#48370,#24360,#24361);
#20926=AXIS2_PLACEMENT_3D('',#48371,#24362,#24363);
#20927=AXIS2_PLACEMENT_3D('',#48380,#24364,#24365);
#20928=AXIS2_PLACEMENT_3D('',#48389,#24366,#24367);
#20929=AXIS2_PLACEMENT_3D('',#48393,#24370,#24371);
#20930=AXIS2_PLACEMENT_3D('',#48402,#24372,#24373);
#20931=AXIS2_PLACEMENT_3D('',#48411,#24374,#24375);
#20932=AXIS2_PLACEMENT_3D('',#48432,#24378,#24379);
#20933=AXIS2_PLACEMENT_3D('',#48434,#24380,#24381);
#20934=AXIS2_PLACEMENT_3D('',#48439,#24382,#24383);
#20935=AXIS2_PLACEMENT_3D('',#48440,#24384,#24385);
#20936=AXIS2_PLACEMENT_3D('',#48441,#24386,#24387);
#20937=AXIS2_PLACEMENT_3D('',#48442,#24388,#24389);
#20938=AXIS2_PLACEMENT_3D('',#48443,#24390,#24391);
#20939=AXIS2_PLACEMENT_3D('',#48446,#24393,#24394);
#20940=AXIS2_PLACEMENT_3D('',#48447,#24395,#24396);
#20941=AXIS2_PLACEMENT_3D('',#48460,#24400,#24401);
#20942=AXIS2_PLACEMENT_3D('',#48469,#24402,#24403);
#20943=AXIS2_PLACEMENT_3D('',#48471,#24404,#24405);
#20944=AXIS2_PLACEMENT_3D('',#48500,#24407,#24408);
#20945=AXIS2_PLACEMENT_3D('',#48506,#24409,#24410);
#20946=AXIS2_PLACEMENT_3D('',#48511,#24411,#24412);
#20947=AXIS2_PLACEMENT_3D('',#48512,#24413,#24414);
#20948=AXIS2_PLACEMENT_3D('',#48513,#24415,#24416);
#20949=AXIS2_PLACEMENT_3D('',#48514,#24417,#24418);
#20950=AXIS2_PLACEMENT_3D('',#48515,#24419,#24420);
#20951=AXIS2_PLACEMENT_3D('',#48516,#24421,#24422);
#20952=AXIS2_PLACEMENT_3D('',#48518,#24423,#24424);
#20953=AXIS2_PLACEMENT_3D('',#48519,#24425,#24426);
#20954=AXIS2_PLACEMENT_3D('',#48520,#24427,#24428);
#20955=AXIS2_PLACEMENT_3D('',#48522,#24429,#24430);
#20956=AXIS2_PLACEMENT_3D('',#48527,#24431,#24432);
#20957=AXIS2_PLACEMENT_3D('',#48529,#24433,#24434);
#20958=AXIS2_PLACEMENT_3D('',#48536,#24435,#24436);
#20959=AXIS2_PLACEMENT_3D('',#48540,#24438,#24439);
#20960=AXIS2_PLACEMENT_3D('',#48543,#24441,#24442);
#20961=AXIS2_PLACEMENT_3D('',#48544,#24443,#24444);
#20962=AXIS2_PLACEMENT_3D('',#48546,#24445,#24446);
#20963=AXIS2_PLACEMENT_3D('',#48547,#24447,#24448);
#20964=AXIS2_PLACEMENT_3D('',#48577,#24449,#24450);
#20965=AXIS2_PLACEMENT_3D('',#48582,#24451,#24452);
#20966=AXIS2_PLACEMENT_3D('',#48600,#24454,#24455);
#20967=AXIS2_PLACEMENT_3D('',#48601,#24456,#24457);
#20968=AXIS2_PLACEMENT_3D('',#48602,#24458,#24459);
#20969=AXIS2_PLACEMENT_3D('',#48603,#24460,#24461);
#20970=AXIS2_PLACEMENT_3D('',#48606,#24463,#24464);
#20971=AXIS2_PLACEMENT_3D('',#48607,#24465,#24466);
#20972=AXIS2_PLACEMENT_3D('',#48609,#24467,#24468);
#20973=AXIS2_PLACEMENT_3D('',#48610,#24469,#24470);
#20974=AXIS2_PLACEMENT_3D('',#48611,#24471,#24472);
#20975=AXIS2_PLACEMENT_3D('',#48613,#24474,#24475);
#20976=AXIS2_PLACEMENT_3D('',#48614,#24476,#24477);
#20977=AXIS2_PLACEMENT_3D('',#48615,#24478,#24479);
#20978=AXIS2_PLACEMENT_3D('',#48617,#24481,#24482);
#20979=AXIS2_PLACEMENT_3D('',#48623,#24486,#24487);
#20980=AXIS2_PLACEMENT_3D('',#48624,#24488,#24489);
#20981=AXIS2_PLACEMENT_3D('',#48625,#24490,#24491);
#20982=AXIS2_PLACEMENT_3D('',#48626,#24492,#24493);
#20983=AXIS2_PLACEMENT_3D('',#48627,#24494,#24495);
#20984=AXIS2_PLACEMENT_3D('',#48628,#24496,#24497);
#20985=AXIS2_PLACEMENT_3D('',#48629,#24498,#24499);
#20986=AXIS2_PLACEMENT_3D('',#48631,#24500,#24501);
#20987=AXIS2_PLACEMENT_3D('',#48632,#24502,#24503);
#20988=AXIS2_PLACEMENT_3D('',#48633,#24504,#24505);
#20989=AXIS2_PLACEMENT_3D('',#48637,#24507,#24508);
#20990=AXIS2_PLACEMENT_3D('',#48638,#24509,#24510);
#20991=AXIS2_PLACEMENT_3D('',#48639,#24511,#24512);
#20992=AXIS2_PLACEMENT_3D('',#48642,#24513,#24514);
#20993=AXIS2_PLACEMENT_3D('',#48644,#24515,#24516);
#20994=AXIS2_PLACEMENT_3D('',#48645,#24517,#24518);
#20995=AXIS2_PLACEMENT_3D('',#48646,#24519,#24520);
#20996=AXIS2_PLACEMENT_3D('',#48649,#24521,#24522);
#20997=AXIS2_PLACEMENT_3D('',#48652,#24525,#24526);
#20998=AXIS2_PLACEMENT_3D('',#48662,#24532,#24533);
#20999=AXIS2_PLACEMENT_3D('',#48665,#24535,#24536);
#21000=AXIS2_PLACEMENT_3D('',#48666,#24537,#24538);
#21001=AXIS2_PLACEMENT_3D('',#48669,#24539,#24540);
#21002=AXIS2_PLACEMENT_3D('',#48673,#24542,#24543);
#21003=AXIS2_PLACEMENT_3D('',#48675,#24544,#24545);
#21004=AXIS2_PLACEMENT_3D('',#48678,#24547,#24548);
#21005=AXIS2_PLACEMENT_3D('',#48679,#24549,#24550);
#21006=AXIS2_PLACEMENT_3D('',#48683,#24552,#24553);
#21007=AXIS2_PLACEMENT_3D('',#48686,#24555,#24556);
#21008=AXIS2_PLACEMENT_3D('',#48687,#24557,#24558);
#21009=AXIS2_PLACEMENT_3D('',#48691,#24561,#24562);
#21010=AXIS2_PLACEMENT_3D('',#48693,#24563,#24564);
#21011=AXIS2_PLACEMENT_3D('',#48696,#24566,#24567);
#21012=AXIS2_PLACEMENT_3D('',#48697,#24568,#24569);
#21013=AXIS2_PLACEMENT_3D('',#48698,#24570,#24571);
#21014=AXIS2_PLACEMENT_3D('',#48699,#24572,#24573);
#21015=AXIS2_PLACEMENT_3D('',#48700,#24574,#24575);
#21016=AXIS2_PLACEMENT_3D('',#48706,#24579,#24580);
#21017=AXIS2_PLACEMENT_3D('',#48710,#24582,#24583);
#21018=AXIS2_PLACEMENT_3D('',#48712,#24585,#24586);
#21019=AXIS2_PLACEMENT_3D('',#48716,#24588,#24589);
#21020=AXIS2_PLACEMENT_3D('',#48723,#24590,#24591);
#21021=AXIS2_PLACEMENT_3D('',#48724,#24592,#24593);
#21022=AXIS2_PLACEMENT_3D('',#48725,#24594,#24595);
#21023=AXIS2_PLACEMENT_3D('',#48726,#24596,#24597);
#21024=AXIS2_PLACEMENT_3D('',#48728,#24598,#24599);
#21025=AXIS2_PLACEMENT_3D('',#48729,#24600,#24601);
#21026=AXIS2_PLACEMENT_3D('',#48731,#24602,#24603);
#21027=AXIS2_PLACEMENT_3D('',#48732,#24604,#24605);
#21028=AXIS2_PLACEMENT_3D('',#48733,#24606,#24607);
#21029=AXIS2_PLACEMENT_3D('',#48737,#24609,#24610);
#21030=AXIS2_PLACEMENT_3D('',#48738,#24611,#24612);
#21031=AXIS2_PLACEMENT_3D('',#48739,#24613,#24614);
#21032=AXIS2_PLACEMENT_3D('',#48741,#24615,#24616);
#21033=AXIS2_PLACEMENT_3D('',#48743,#24617,#24618);
#21034=AXIS2_PLACEMENT_3D('',#48745,#24620,#24621);
#21035=AXIS2_PLACEMENT_3D('',#48746,#24622,#24623);
#21036=AXIS2_PLACEMENT_3D('',#48747,#24624,#24625);
#21037=AXIS2_PLACEMENT_3D('',#48749,#24626,#24627);
#21038=AXIS2_PLACEMENT_3D('',#48751,#24629,#24630);
#21039=AXIS2_PLACEMENT_3D('',#48752,#24631,#24632);
#21040=AXIS2_PLACEMENT_3D('',#48753,#24633,#24634);
#21041=AXIS2_PLACEMENT_3D('',#48756,#24636,#24637);
#21042=AXIS2_PLACEMENT_3D('',#48757,#24638,#24639);
#21043=AXIS2_PLACEMENT_3D('',#48760,#24640,#24641);
#21044=AXIS2_PLACEMENT_3D('',#48761,#24642,#24643);
#21045=AXIS2_PLACEMENT_3D('',#48762,#24644,#24645);
#21046=AXIS2_PLACEMENT_3D('',#48763,#24646,#24647);
#21047=AXIS2_PLACEMENT_3D('',#48767,#24649,#24650);
#21048=AXIS2_PLACEMENT_3D('',#48769,#24652,#24653);
#21049=AXIS2_PLACEMENT_3D('',#48771,#24655,#24656);
#21050=AXIS2_PLACEMENT_3D('',#48773,#24657,#24658);
#21051=AXIS2_PLACEMENT_3D('',#48775,#24660,#24661);
#21052=AXIS2_PLACEMENT_3D('',#48778,#24663,#24664);
#21053=AXIS2_PLACEMENT_3D('',#48779,#24665,#24666);
#21054=AXIS2_PLACEMENT_3D('',#48780,#24667,#24668);
#21055=AXIS2_PLACEMENT_3D('',#48781,#24669,#24670);
#21056=AXIS2_PLACEMENT_3D('',#48783,#24672,#24673);
#21057=AXIS2_PLACEMENT_3D('',#48786,#24675,#24676);
#21058=AXIS2_PLACEMENT_3D('',#48787,#24677,#24678);
#21059=AXIS2_PLACEMENT_3D('',#48791,#24681,#24682);
#21060=AXIS2_PLACEMENT_3D('',#48794,#24683,#24684);
#21061=AXIS2_PLACEMENT_3D('',#48796,#24685,#24686);
#21062=AXIS2_PLACEMENT_3D('',#48797,#24687,#24688);
#21063=AXIS2_PLACEMENT_3D('',#48798,#24689,#24690);
#21064=AXIS2_PLACEMENT_3D('',#48799,#24691,#24692);
#21065=AXIS2_PLACEMENT_3D('',#48802,#24693,#24694);
#21066=AXIS2_PLACEMENT_3D('',#48804,#24696,#24697);
#21067=AXIS2_PLACEMENT_3D('',#48805,#24698,#24699);
#21068=AXIS2_PLACEMENT_3D('',#48807,#24700,#24701);
#21069=AXIS2_PLACEMENT_3D('',#48808,#24702,#24703);
#21070=AXIS2_PLACEMENT_3D('',#48811,#24704,#24705);
#21071=AXIS2_PLACEMENT_3D('',#48812,#24706,#24707);
#21072=AXIS2_PLACEMENT_3D('',#48813,#24708,#24709);
#21073=AXIS2_PLACEMENT_3D('',#48814,#24710,#24711);
#21074=AXIS2_PLACEMENT_3D('',#48817,#24712,#24713);
#21075=AXIS2_PLACEMENT_3D('',#48819,#24715,#24716);
#21076=AXIS2_PLACEMENT_3D('',#48820,#24717,#24718);
#21077=AXIS2_PLACEMENT_3D('',#48821,#24719,#24720);
#21078=AXIS2_PLACEMENT_3D('',#48822,#24721,#24722);
#21079=AXIS2_PLACEMENT_3D('',#48823,#24723,#24724);
#21080=AXIS2_PLACEMENT_3D('',#48825,#24725,#24726);
#21081=AXIS2_PLACEMENT_3D('',#48826,#24727,#24728);
#21082=AXIS2_PLACEMENT_3D('',#48827,#24729,#24730);
#21083=AXIS2_PLACEMENT_3D('',#48828,#24731,#24732);
#21084=AXIS2_PLACEMENT_3D('',#48830,#24733,#24734);
#21085=AXIS2_PLACEMENT_3D('',#48831,#24735,#24736);
#21086=AXIS2_PLACEMENT_3D('',#48833,#24737,#24738);
#21087=AXIS2_PLACEMENT_3D('',#48834,#24739,#24740);
#21088=AXIS2_PLACEMENT_3D('',#48835,#24741,#24742);
#21089=AXIS2_PLACEMENT_3D('',#48837,#24744,#24745);
#21090=AXIS2_PLACEMENT_3D('',#48841,#24748,#24749);
#21091=AXIS2_PLACEMENT_3D('',#48844,#24751,#24752);
#21092=AXIS2_PLACEMENT_3D('',#48845,#24753,#24754);
#21093=AXIS2_PLACEMENT_3D('',#48846,#24755,#24756);
#21094=AXIS2_PLACEMENT_3D('',#48847,#24757,#24758);
#21095=AXIS2_PLACEMENT_3D('',#48855,#24763,#24764);
#21096=AXIS2_PLACEMENT_3D('',#48856,#24765,#24766);
#21097=AXIS2_PLACEMENT_3D('',#48857,#24767,#24768);
#21098=AXIS2_PLACEMENT_3D('',#48859,#24769,#24770);
#21099=AXIS2_PLACEMENT_3D('',#48860,#24771,#24772);
#21100=AXIS2_PLACEMENT_3D('',#48861,#24773,#24774);
#21101=AXIS2_PLACEMENT_3D('',#48865,#24776,#24777);
#21102=AXIS2_PLACEMENT_3D('',#48866,#24778,#24779);
#21103=AXIS2_PLACEMENT_3D('',#48867,#24780,#24781);
#21104=AXIS2_PLACEMENT_3D('',#48869,#24782,#24783);
#21105=AXIS2_PLACEMENT_3D('',#48870,#24784,#24785);
#21106=AXIS2_PLACEMENT_3D('',#48871,#24786,#24787);
#21107=AXIS2_PLACEMENT_3D('',#48875,#24789,#24790);
#21108=AXIS2_PLACEMENT_3D('',#48876,#24791,#24792);
#21109=AXIS2_PLACEMENT_3D('',#48877,#24793,#24794);
#21110=AXIS2_PLACEMENT_3D('',#48879,#24795,#24796);
#21111=AXIS2_PLACEMENT_3D('',#48881,#24797,#24798);
#21112=AXIS2_PLACEMENT_3D('',#48883,#24799,#24800);
#21113=AXIS2_PLACEMENT_3D('',#48884,#24801,#24802);
#21114=AXIS2_PLACEMENT_3D('',#48885,#24803,#24804);
#21115=AXIS2_PLACEMENT_3D('',#48887,#24805,#24806);
#21116=AXIS2_PLACEMENT_3D('',#48889,#24807,#24808);
#21117=AXIS2_PLACEMENT_3D('',#48891,#24809,#24810);
#21118=AXIS2_PLACEMENT_3D('',#48893,#24811,#24812);
#21119=AXIS2_PLACEMENT_3D('',#48895,#24813,#24814);
#21120=AXIS2_PLACEMENT_3D('',#48897,#24815,#24816);
#21121=AXIS2_PLACEMENT_3D('',#48899,#24817,#24818);
#21122=AXIS2_PLACEMENT_3D('',#48901,#24819,#24820);
#21123=AXIS2_PLACEMENT_3D('',#48903,#24821,#24822);
#21124=AXIS2_PLACEMENT_3D('',#48905,#24823,#24824);
#21125=AXIS2_PLACEMENT_3D('',#48907,#24825,#24826);
#21126=AXIS2_PLACEMENT_3D('',#48908,#24827,#24828);
#21127=AXIS2_PLACEMENT_3D('',#48910,#24829,#24830);
#21128=AXIS2_PLACEMENT_3D('',#48912,#24832,#24833);
#21129=AXIS2_PLACEMENT_3D('',#48914,#24834,#24835);
#21130=AXIS2_PLACEMENT_3D('',#48916,#24836,#24837);
#21131=AXIS2_PLACEMENT_3D('',#48917,#24838,#24839);
#21132=AXIS2_PLACEMENT_3D('',#48918,#24840,#24841);
#21133=AXIS2_PLACEMENT_3D('',#48920,#24842,#24843);
#21134=AXIS2_PLACEMENT_3D('',#48922,#24845,#24846);
#21135=AXIS2_PLACEMENT_3D('',#48923,#24847,#24848);
#21136=AXIS2_PLACEMENT_3D('',#48924,#24849,#24850);
#21137=AXIS2_PLACEMENT_3D('',#48925,#24851,#24852);
#21138=AXIS2_PLACEMENT_3D('',#48926,#24853,#24854);
#21139=AXIS2_PLACEMENT_3D('',#48927,#24855,#24856);
#21140=AXIS2_PLACEMENT_3D('',#48928,#24857,#24858);
#21141=AXIS2_PLACEMENT_3D('',#48930,#24859,#24860);
#21142=AXIS2_PLACEMENT_3D('',#48932,#24861,#24862);
#21143=AXIS2_PLACEMENT_3D('',#48933,#24863,#24864);
#21144=AXIS2_PLACEMENT_3D('',#48934,#24865,#24866);
#21145=AXIS2_PLACEMENT_3D('',#48936,#24867,#24868);
#21146=AXIS2_PLACEMENT_3D('',#48938,#24870,#24871);
#21147=AXIS2_PLACEMENT_3D('',#48939,#24872,#24873);
#21148=AXIS2_PLACEMENT_3D('',#48940,#24874,#24875);
#21149=AXIS2_PLACEMENT_3D('',#48941,#24876,#24877);
#21150=AXIS2_PLACEMENT_3D('',#48942,#24878,#24879);
#21151=AXIS2_PLACEMENT_3D('',#48944,#24880,#24881);
#21152=AXIS2_PLACEMENT_3D('',#48946,#24882,#24883);
#21153=AXIS2_PLACEMENT_3D('',#48947,#24884,#24885);
#21154=AXIS2_PLACEMENT_3D('',#48948,#24886,#24887);
#21155=AXIS2_PLACEMENT_3D('',#48950,#24888,#24889);
#21156=AXIS2_PLACEMENT_3D('',#48952,#24891,#24892);
#21157=AXIS2_PLACEMENT_3D('',#48954,#24893,#24894);
#21158=AXIS2_PLACEMENT_3D('',#48955,#24895,#24896);
#21159=AXIS2_PLACEMENT_3D('',#48957,#24897,#24898);
#21160=AXIS2_PLACEMENT_3D('',#48959,#24899,#24900);
#21161=AXIS2_PLACEMENT_3D('',#48960,#24901,#24902);
#21162=AXIS2_PLACEMENT_3D('',#48961,#24903,#24904);
#21163=AXIS2_PLACEMENT_3D('',#48963,#24905,#24906);
#21164=AXIS2_PLACEMENT_3D('',#48965,#24908,#24909);
#21165=AXIS2_PLACEMENT_3D('',#48967,#24910,#24911);
#21166=AXIS2_PLACEMENT_3D('',#48968,#24912,#24913);
#21167=AXIS2_PLACEMENT_3D('',#48970,#24914,#24915);
#21168=AXIS2_PLACEMENT_3D('',#48972,#24916,#24917);
#21169=AXIS2_PLACEMENT_3D('',#48973,#24918,#24919);
#21170=AXIS2_PLACEMENT_3D('',#48974,#24920,#24921);
#21171=AXIS2_PLACEMENT_3D('',#48976,#24922,#24923);
#21172=AXIS2_PLACEMENT_3D('',#48978,#24925,#24926);
#21173=AXIS2_PLACEMENT_3D('',#48980,#24927,#24928);
#21174=AXIS2_PLACEMENT_3D('',#48981,#24929,#24930);
#21175=AXIS2_PLACEMENT_3D('',#48985,#24932,#24933);
#21176=AXIS2_PLACEMENT_3D('',#48987,#24935,#24936);
#21177=AXIS2_PLACEMENT_3D('',#48988,#24937,#24938);
#21178=AXIS2_PLACEMENT_3D('',#48990,#24940,#24941);
#21179=AXIS2_PLACEMENT_3D('',#48991,#24942,#24943);
#21180=AXIS2_PLACEMENT_3D('',#48992,#24944,#24945);
#21181=AXIS2_PLACEMENT_3D('',#49016,#24949,#24950);
#21182=AXIS2_PLACEMENT_3D('',#49018,#24951,#24952);
#21183=AXIS2_PLACEMENT_3D('',#49030,#24953,#24954);
#21184=AXIS2_PLACEMENT_3D('',#49033,#24955,#24956);
#21185=AXIS2_PLACEMENT_3D('',#49034,#24957,#24958);
#21186=AXIS2_PLACEMENT_3D('',#49036,#24959,#24960);
#21187=AXIS2_PLACEMENT_3D('',#49038,#24961,#24962);
#21188=AXIS2_PLACEMENT_3D('',#49039,#24963,#24964);
#21189=AXIS2_PLACEMENT_3D('',#49040,#24965,#24966);
#21190=AXIS2_PLACEMENT_3D('',#49044,#24968,#24969);
#21191=AXIS2_PLACEMENT_3D('',#49045,#24970,#24971);
#21192=AXIS2_PLACEMENT_3D('',#49046,#24972,#24973);
#21193=AXIS2_PLACEMENT_3D('',#49049,#24974,#24975);
#21194=AXIS2_PLACEMENT_3D('',#49051,#24977,#24978);
#21195=AXIS2_PLACEMENT_3D('',#49052,#24979,#24980);
#21196=AXIS2_PLACEMENT_3D('',#49054,#24981,#24982);
#21197=AXIS2_PLACEMENT_3D('',#49055,#24983,#24984);
#21198=AXIS2_PLACEMENT_3D('',#49056,#24985,#24986);
#21199=AXIS2_PLACEMENT_3D('',#49058,#24987,#24988);
#21200=AXIS2_PLACEMENT_3D('',#49060,#24989,#24990);
#21201=AXIS2_PLACEMENT_3D('',#49062,#24991,#24992);
#21202=AXIS2_PLACEMENT_3D('',#49064,#24993,#24994);
#21203=AXIS2_PLACEMENT_3D('',#49066,#24995,#24996);
#21204=AXIS2_PLACEMENT_3D('',#49068,#24997,#24998);
#21205=AXIS2_PLACEMENT_3D('',#49070,#24999,#25000);
#21206=AXIS2_PLACEMENT_3D('',#49071,#25001,#25002);
#21207=AXIS2_PLACEMENT_3D('',#49072,#25003,#25004);
#21208=AXIS2_PLACEMENT_3D('',#49073,#25005,#25006);
#21209=AXIS2_PLACEMENT_3D('',#49074,#25007,#25008);
#21210=AXIS2_PLACEMENT_3D('',#49075,#25009,#25010);
#21211=AXIS2_PLACEMENT_3D('',#49076,#25011,#25012);
#21212=AXIS2_PLACEMENT_3D('',#49077,#25013,#25014);
#21213=AXIS2_PLACEMENT_3D('',#49080,#25015,#25016);
#21214=AXIS2_PLACEMENT_3D('',#49081,#25017,#25018);
#21215=AXIS2_PLACEMENT_3D('',#49082,#25019,#25020);
#21216=AXIS2_PLACEMENT_3D('',#49083,#25021,#25022);
#21217=AXIS2_PLACEMENT_3D('',#49087,#25024,#25025);
#21218=AXIS2_PLACEMENT_3D('',#49088,#25026,#25027);
#21219=AXIS2_PLACEMENT_3D('',#49089,#25028,#25029);
#21220=AXIS2_PLACEMENT_3D('',#49092,#25030,#25031);
#21221=AXIS2_PLACEMENT_3D('',#49093,#25032,#25033);
#21222=AXIS2_PLACEMENT_3D('',#49094,#25034,#25035);
#21223=AXIS2_PLACEMENT_3D('',#49095,#25036,#25037);
#21224=AXIS2_PLACEMENT_3D('',#49099,#25039,#25040);
#21225=AXIS2_PLACEMENT_3D('',#49100,#25041,#25042);
#21226=AXIS2_PLACEMENT_3D('',#49101,#25043,#25044);
#21227=AXIS2_PLACEMENT_3D('',#49102,#25045,#25046);
#21228=AXIS2_PLACEMENT_3D('',#49103,#25047,#25048);
#21229=AXIS2_PLACEMENT_3D('',#49105,#25049,#25050);
#21230=AXIS2_PLACEMENT_3D('',#49107,#25051,#25052);
#21231=AXIS2_PLACEMENT_3D('',#49108,#25053,#25054);
#21232=AXIS2_PLACEMENT_3D('',#49109,#25055,#25056);
#21233=AXIS2_PLACEMENT_3D('',#49112,#25057,#25058);
#21234=AXIS2_PLACEMENT_3D('',#49114,#25060,#25061);
#21235=AXIS2_PLACEMENT_3D('',#49115,#25062,#25063);
#21236=AXIS2_PLACEMENT_3D('',#49118,#25064,#25065);
#21237=AXIS2_PLACEMENT_3D('',#49119,#25066,#25067);
#21238=AXIS2_PLACEMENT_3D('',#49120,#25068,#25069);
#21239=AXIS2_PLACEMENT_3D('',#49121,#25070,#25071);
#21240=AXIS2_PLACEMENT_3D('',#49123,#25072,#25073);
#21241=AXIS2_PLACEMENT_3D('',#49126,#25075,#25076);
#21242=AXIS2_PLACEMENT_3D('',#49131,#25077,#25078);
#21243=AXIS2_PLACEMENT_3D('',#49132,#25079,#25080);
#21244=AXIS2_PLACEMENT_3D('',#49133,#25081,#25082);
#21245=AXIS2_PLACEMENT_3D('',#49134,#25083,#25084);
#21246=AXIS2_PLACEMENT_3D('',#49135,#25085,#25086);
#21247=AXIS2_PLACEMENT_3D('',#49136,#25087,#25088);
#21248=AXIS2_PLACEMENT_3D('',#49137,#25089,#25090);
#21249=AXIS2_PLACEMENT_3D('',#49144,#25091,#25092);
#21250=AXIS2_PLACEMENT_3D('',#49153,#25093,#25094);
#21251=AXIS2_PLACEMENT_3D('',#49154,#25095,#25096);
#21252=AXIS2_PLACEMENT_3D('',#49156,#25097,#25098);
#21253=AXIS2_PLACEMENT_3D('',#49158,#25099,#25100);
#21254=AXIS2_PLACEMENT_3D('',#49160,#25101,#25102);
#21255=AXIS2_PLACEMENT_3D('',#49161,#25103,#25104);
#21256=AXIS2_PLACEMENT_3D('',#49162,#25105,#25106);
#21257=AXIS2_PLACEMENT_3D('',#49166,#25109,#25110);
#21258=AXIS2_PLACEMENT_3D('',#49168,#25111,#25112);
#21259=AXIS2_PLACEMENT_3D('',#49170,#25113,#25114);
#21260=AXIS2_PLACEMENT_3D('',#49171,#25115,#25116);
#21261=AXIS2_PLACEMENT_3D('',#49173,#25118,#25119);
#21262=AXIS2_PLACEMENT_3D('',#49175,#25120,#25121);
#21263=AXIS2_PLACEMENT_3D('',#49177,#25122,#25123);
#21264=AXIS2_PLACEMENT_3D('',#49178,#25124,#25125);
#21265=AXIS2_PLACEMENT_3D('',#49179,#25126,#25127);
#21266=AXIS2_PLACEMENT_3D('',#49181,#25129,#25130);
#21267=AXIS2_PLACEMENT_3D('',#49183,#25131,#25132);
#21268=AXIS2_PLACEMENT_3D('',#49185,#25133,#25134);
#21269=AXIS2_PLACEMENT_3D('',#49186,#25135,#25136);
#21270=AXIS2_PLACEMENT_3D('',#49187,#25137,#25138);
#21271=AXIS2_PLACEMENT_3D('',#49189,#25140,#25141);
#21272=AXIS2_PLACEMENT_3D('',#49192,#25142,#25143);
#21273=AXIS2_PLACEMENT_3D('',#49193,#25144,#25145);
#21274=AXIS2_PLACEMENT_3D('',#49194,#25146,#25147);
#21275=AXIS2_PLACEMENT_3D('',#49195,#25148,#25149);
#21276=AXIS2_PLACEMENT_3D('',#49199,#25151,#25152);
#21277=AXIS2_PLACEMENT_3D('',#49200,#25153,#25154);
#21278=AXIS2_PLACEMENT_3D('',#49201,#25155,#25156);
#21279=AXIS2_PLACEMENT_3D('',#49202,#25157,#25158);
#21280=AXIS2_PLACEMENT_3D('',#49203,#25159,#25160);
#21281=AXIS2_PLACEMENT_3D('',#49205,#25162,#25163);
#21282=AXIS2_PLACEMENT_3D('',#49206,#25164,#25165);
#21283=AXIS2_PLACEMENT_3D('',#49207,#25166,#25167);
#21284=AXIS2_PLACEMENT_3D('',#49208,#25168,#25169);
#21285=AXIS2_PLACEMENT_3D('',#49209,#25170,#25171);
#21286=AXIS2_PLACEMENT_3D('',#49210,#25172,#25173);
#21287=AXIS2_PLACEMENT_3D('',#49211,#25174,#25175);
#21288=AXIS2_PLACEMENT_3D('',#49213,#25177,#25178);
#21289=AXIS2_PLACEMENT_3D('',#49214,#25179,#25180);
#21290=AXIS2_PLACEMENT_3D('',#49215,#25181,#25182);
#21291=AXIS2_PLACEMENT_3D('',#49216,#25183,#25184);
#21292=AXIS2_PLACEMENT_3D('',#49217,#25185,#25186);
#21293=AXIS2_PLACEMENT_3D('',#49218,#25187,#25188);
#21294=AXIS2_PLACEMENT_3D('',#49219,#25189,#25190);
#21295=AXIS2_PLACEMENT_3D('',#49221,#25192,#25193);
#21296=AXIS2_PLACEMENT_3D('',#49223,#25195,#25196);
#21297=AXIS2_PLACEMENT_3D('',#49225,#25198,#25199);
#21298=AXIS2_PLACEMENT_3D('',#49227,#25201,#25202);
#21299=AXIS2_PLACEMENT_3D('',#49228,#25203,#25204);
#21300=AXIS2_PLACEMENT_3D('',#49231,#25205,#25206);
#21301=AXIS2_PLACEMENT_3D('',#49232,#25207,#25208);
#21302=AXIS2_PLACEMENT_3D('',#49235,#25210,#25211);
#21303=AXIS2_PLACEMENT_3D('',#49236,#25212,#25213);
#21304=AXIS2_PLACEMENT_3D('',#49240,#25215,#25216);
#21305=AXIS2_PLACEMENT_3D('',#49241,#25217,#25218);
#21306=AXIS2_PLACEMENT_3D('',#49242,#25219,#25220);
#21307=AXIS2_PLACEMENT_3D('',#49271,#25221,#25222);
#21308=AXIS2_PLACEMENT_3D('',#49303,#25223,#25224);
#21309=AXIS2_PLACEMENT_3D('',#49331,#25225,#25226);
#21310=AXIS2_PLACEMENT_3D('',#49363,#25227,#25228);
#21311=AXIS2_PLACEMENT_3D('',#49391,#25229,#25230);
#21312=AXIS2_PLACEMENT_3D('',#49423,#25231,#25232);
#21313=AXIS2_PLACEMENT_3D('',#49451,#25233,#25234);
#21314=AXIS2_PLACEMENT_3D('',#49483,#25235,#25236);
#21315=AXIS2_PLACEMENT_3D('',#49511,#25237,#25238);
#21316=AXIS2_PLACEMENT_3D('',#49543,#25239,#25240);
#21317=AXIS2_PLACEMENT_3D('',#49571,#25241,#25242);
#21318=AXIS2_PLACEMENT_3D('',#49603,#25243,#25244);
#21319=AXIS2_PLACEMENT_3D('',#49631,#25245,#25246);
#21320=AXIS2_PLACEMENT_3D('',#49663,#25247,#25248);
#21321=AXIS2_PLACEMENT_3D('',#49691,#25249,#25250);
#21322=AXIS2_PLACEMENT_3D('',#49723,#25251,#25252);
#21323=AXIS2_PLACEMENT_3D('',#49751,#25253,#25254);
#21324=AXIS2_PLACEMENT_3D('',#49783,#25255,#25256);
#21325=AXIS2_PLACEMENT_3D('',#49811,#25257,#25258);
#21326=AXIS2_PLACEMENT_3D('',#49843,#25259,#25260);
#21327=AXIS2_PLACEMENT_3D('',#49871,#25261,#25262);
#21328=AXIS2_PLACEMENT_3D('',#49903,#25263,#25264);
#21329=AXIS2_PLACEMENT_3D('',#49931,#25265,#25266);
#21330=AXIS2_PLACEMENT_3D('',#49963,#25267,#25268);
#21331=AXIS2_PLACEMENT_3D('',#49991,#25269,#25270);
#21332=AXIS2_PLACEMENT_3D('',#50023,#25271,#25272);
#21333=AXIS2_PLACEMENT_3D('',#50051,#25273,#25274);
#21334=AXIS2_PLACEMENT_3D('',#50082,#25275,#25276);
#21335=AXIS2_PLACEMENT_3D('',#50083,#25277,#25278);
#21336=AXIS2_PLACEMENT_3D('',#50085,#25279,#25280);
#21337=AXIS2_PLACEMENT_3D('',#50087,#25282,#25283);
#21338=AXIS2_PLACEMENT_3D('',#50120,#25284,#25285);
#21339=AXIS2_PLACEMENT_3D('',#50149,#25286,#25287);
#21340=AXIS2_PLACEMENT_3D('',#50181,#25288,#25289);
#21341=AXIS2_PLACEMENT_3D('',#50210,#25290,#25291);
#21342=AXIS2_PLACEMENT_3D('',#50242,#25292,#25293);
#21343=AXIS2_PLACEMENT_3D('',#50271,#25294,#25295);
#21344=AXIS2_PLACEMENT_3D('',#50303,#25296,#25297);
#21345=AXIS2_PLACEMENT_3D('',#50332,#25298,#25299);
#21346=AXIS2_PLACEMENT_3D('',#50364,#25300,#25301);
#21347=AXIS2_PLACEMENT_3D('',#50393,#25302,#25303);
#21348=AXIS2_PLACEMENT_3D('',#50425,#25304,#25305);
#21349=AXIS2_PLACEMENT_3D('',#50454,#25306,#25307);
#21350=AXIS2_PLACEMENT_3D('',#50486,#25308,#25309);
#21351=AXIS2_PLACEMENT_3D('',#50515,#25310,#25311);
#21352=AXIS2_PLACEMENT_3D('',#50547,#25312,#25313);
#21353=AXIS2_PLACEMENT_3D('',#50576,#25314,#25315);
#21354=AXIS2_PLACEMENT_3D('',#50608,#25316,#25317);
#21355=AXIS2_PLACEMENT_3D('',#50637,#25318,#25319);
#21356=AXIS2_PLACEMENT_3D('',#50669,#25320,#25321);
#21357=AXIS2_PLACEMENT_3D('',#50698,#25322,#25323);
#21358=AXIS2_PLACEMENT_3D('',#50730,#25324,#25325);
#21359=AXIS2_PLACEMENT_3D('',#50759,#25326,#25327);
#21360=AXIS2_PLACEMENT_3D('',#50791,#25328,#25329);
#21361=AXIS2_PLACEMENT_3D('',#50820,#25330,#25331);
#21362=AXIS2_PLACEMENT_3D('',#50852,#25332,#25333);
#21363=AXIS2_PLACEMENT_3D('',#50881,#25334,#25335);
#21364=AXIS2_PLACEMENT_3D('',#50913,#25336,#25337);
#21365=AXIS2_PLACEMENT_3D('',#50942,#25338,#25339);
#21366=AXIS2_PLACEMENT_3D('',#50974,#25340,#25341);
#21367=AXIS2_PLACEMENT_3D('',#51003,#25342,#25343);
#21368=AXIS2_PLACEMENT_3D('',#51035,#25344,#25345);
#21369=AXIS2_PLACEMENT_3D('',#51064,#25346,#25347);
#21370=AXIS2_PLACEMENT_3D('',#51096,#25348,#25349);
#21371=AXIS2_PLACEMENT_3D('',#51125,#25350,#25351);
#21372=AXIS2_PLACEMENT_3D('',#51157,#25352,#25353);
#21373=AXIS2_PLACEMENT_3D('',#51186,#25354,#25355);
#21374=AXIS2_PLACEMENT_3D('',#51218,#25356,#25357);
#21375=AXIS2_PLACEMENT_3D('',#51247,#25358,#25359);
#21376=AXIS2_PLACEMENT_3D('',#51279,#25360,#25361);
#21377=AXIS2_PLACEMENT_3D('',#51308,#25362,#25363);
#21378=AXIS2_PLACEMENT_3D('',#51340,#25364,#25365);
#21379=AXIS2_PLACEMENT_3D('',#51369,#25366,#25367);
#21380=AXIS2_PLACEMENT_3D('',#51401,#25368,#25369);
#21381=AXIS2_PLACEMENT_3D('',#51430,#25370,#25371);
#21382=AXIS2_PLACEMENT_3D('',#51462,#25372,#25373);
#21383=AXIS2_PLACEMENT_3D('',#51491,#25374,#25375);
#21384=AXIS2_PLACEMENT_3D('',#51523,#25376,#25377);
#21385=AXIS2_PLACEMENT_3D('',#51552,#25378,#25379);
#21386=AXIS2_PLACEMENT_3D('',#51584,#25380,#25381);
#21387=AXIS2_PLACEMENT_3D('',#51612,#25382,#25383);
#21388=AXIS2_PLACEMENT_3D('',#51744,#25385,#25386);
#21389=AXIS2_PLACEMENT_3D('',#51746,#25387,#25388);
#21390=AXIS2_PLACEMENT_3D('',#51871,#25390,#25391);
#21391=AXIS2_PLACEMENT_3D('',#51873,#25392,#25393);
#21392=AXIS2_PLACEMENT_3D('',#51880,#25394,#25395);
#21393=AXIS2_PLACEMENT_3D('',#51882,#25396,#25397);
#21394=AXIS2_PLACEMENT_3D('',#52014,#25399,#25400);
#21395=AXIS2_PLACEMENT_3D('',#52016,#25401,#25402);
#21396=AXIS2_PLACEMENT_3D('',#52144,#25404,#25405);
#21397=AXIS2_PLACEMENT_3D('',#52177,#25406,#25407);
#21398=AXIS2_PLACEMENT_3D('',#52206,#25408,#25409);
#21399=AXIS2_PLACEMENT_3D('',#52238,#25410,#25411);
#21400=AXIS2_PLACEMENT_3D('',#52267,#25412,#25413);
#21401=AXIS2_PLACEMENT_3D('',#52299,#25414,#25415);
#21402=AXIS2_PLACEMENT_3D('',#52328,#25416,#25417);
#21403=AXIS2_PLACEMENT_3D('',#52360,#25418,#25419);
#21404=AXIS2_PLACEMENT_3D('',#52389,#25420,#25421);
#21405=AXIS2_PLACEMENT_3D('',#52421,#25422,#25423);
#21406=AXIS2_PLACEMENT_3D('',#52450,#25424,#25425);
#21407=AXIS2_PLACEMENT_3D('',#52482,#25426,#25427);
#21408=AXIS2_PLACEMENT_3D('',#52511,#25428,#25429);
#21409=AXIS2_PLACEMENT_3D('',#52543,#25430,#25431);
#21410=AXIS2_PLACEMENT_3D('',#52572,#25432,#25433);
#21411=AXIS2_PLACEMENT_3D('',#52604,#25434,#25435);
#21412=AXIS2_PLACEMENT_3D('',#52633,#25436,#25437);
#21413=AXIS2_PLACEMENT_3D('',#52665,#25438,#25439);
#21414=AXIS2_PLACEMENT_3D('',#52694,#25440,#25441);
#21415=AXIS2_PLACEMENT_3D('',#52726,#25442,#25443);
#21416=AXIS2_PLACEMENT_3D('',#52755,#25444,#25445);
#21417=AXIS2_PLACEMENT_3D('',#52787,#25446,#25447);
#21418=AXIS2_PLACEMENT_3D('',#52816,#25448,#25449);
#21419=AXIS2_PLACEMENT_3D('',#52848,#25450,#25451);
#21420=AXIS2_PLACEMENT_3D('',#52877,#25452,#25453);
#21421=AXIS2_PLACEMENT_3D('',#52909,#25454,#25455);
#21422=AXIS2_PLACEMENT_3D('',#52938,#25456,#25457);
#21423=AXIS2_PLACEMENT_3D('',#52970,#25458,#25459);
#21424=AXIS2_PLACEMENT_3D('',#52999,#25460,#25461);
#21425=AXIS2_PLACEMENT_3D('',#53031,#25462,#25463);
#21426=AXIS2_PLACEMENT_3D('',#53060,#25464,#25465);
#21427=AXIS2_PLACEMENT_3D('',#53092,#25466,#25467);
#21428=AXIS2_PLACEMENT_3D('',#53121,#25468,#25469);
#21429=AXIS2_PLACEMENT_3D('',#53153,#25470,#25471);
#21430=AXIS2_PLACEMENT_3D('',#53182,#25472,#25473);
#21431=AXIS2_PLACEMENT_3D('',#53214,#25474,#25475);
#21432=AXIS2_PLACEMENT_3D('',#53243,#25476,#25477);
#21433=AXIS2_PLACEMENT_3D('',#53275,#25478,#25479);
#21434=AXIS2_PLACEMENT_3D('',#53304,#25480,#25481);
#21435=AXIS2_PLACEMENT_3D('',#53336,#25482,#25483);
#21436=AXIS2_PLACEMENT_3D('',#53365,#25484,#25485);
#21437=AXIS2_PLACEMENT_3D('',#53397,#25486,#25487);
#21438=AXIS2_PLACEMENT_3D('',#53426,#25488,#25489);
#21439=AXIS2_PLACEMENT_3D('',#53458,#25490,#25491);
#21440=AXIS2_PLACEMENT_3D('',#53487,#25492,#25493);
#21441=AXIS2_PLACEMENT_3D('',#53519,#25494,#25495);
#21442=AXIS2_PLACEMENT_3D('',#53548,#25496,#25497);
#21443=AXIS2_PLACEMENT_3D('',#53580,#25498,#25499);
#21444=AXIS2_PLACEMENT_3D('',#53609,#25500,#25501);
#21445=AXIS2_PLACEMENT_3D('',#53641,#25502,#25503);
#21446=AXIS2_PLACEMENT_3D('',#53669,#25504,#25505);
#21447=AXIS2_PLACEMENT_3D('',#53670,#25506,#25507);
#21448=AXIS2_PLACEMENT_3D('',#53672,#25508,#25509);
#21449=AXIS2_PLACEMENT_3D('',#53709,#25510,#25511);
#21450=AXIS2_PLACEMENT_3D('',#53741,#25512,#25513);
#21451=AXIS2_PLACEMENT_3D('',#53778,#25514,#25515);
#21452=AXIS2_PLACEMENT_3D('',#53810,#25516,#25517);
#21453=AXIS2_PLACEMENT_3D('',#53847,#25518,#25519);
#21454=AXIS2_PLACEMENT_3D('',#53879,#25520,#25521);
#21455=AXIS2_PLACEMENT_3D('',#53916,#25522,#25523);
#21456=AXIS2_PLACEMENT_3D('',#53948,#25524,#25525);
#21457=AXIS2_PLACEMENT_3D('',#53985,#25526,#25527);
#21458=AXIS2_PLACEMENT_3D('',#54017,#25528,#25529);
#21459=AXIS2_PLACEMENT_3D('',#54054,#25530,#25531);
#21460=AXIS2_PLACEMENT_3D('',#54086,#25532,#25533);
#21461=AXIS2_PLACEMENT_3D('',#54123,#25534,#25535);
#21462=AXIS2_PLACEMENT_3D('',#54155,#25536,#25537);
#21463=AXIS2_PLACEMENT_3D('',#54192,#25538,#25539);
#21464=AXIS2_PLACEMENT_3D('',#54224,#25540,#25541);
#21465=AXIS2_PLACEMENT_3D('',#54261,#25542,#25543);
#21466=AXIS2_PLACEMENT_3D('',#54293,#25544,#25545);
#21467=AXIS2_PLACEMENT_3D('',#54330,#25546,#25547);
#21468=AXIS2_PLACEMENT_3D('',#54362,#25548,#25549);
#21469=AXIS2_PLACEMENT_3D('',#54399,#25550,#25551);
#21470=AXIS2_PLACEMENT_3D('',#54431,#25552,#25553);
#21471=AXIS2_PLACEMENT_3D('',#54468,#25554,#25555);
#21472=AXIS2_PLACEMENT_3D('',#54498,#25556,#25557);
#21473=AXIS2_PLACEMENT_3D('',#54500,#25558,#25559);
#21474=AXIS2_PLACEMENT_3D('',#54507,#25560,#25561);
#21475=AXIS2_PLACEMENT_3D('',#54593,#25563,#25564);
#21476=AXIS2_PLACEMENT_3D('',#54688,#25566,#25567);
#21477=AXIS2_PLACEMENT_3D('',#54689,#25568,#25569);
#21478=AXIS2_PLACEMENT_3D('',#54690,#25570,#25571);
#21479=AXIS2_PLACEMENT_3D('',#54785,#25573,#25574);
#21480=AXIS2_PLACEMENT_3D('',#54878,#25576,#25577);
#21481=AXIS2_PLACEMENT_3D('',#54880,#25578,#25579);
#21482=AXIS2_PLACEMENT_3D('',#54887,#25580,#25581);
#21483=AXIS2_PLACEMENT_3D('',#54979,#25583,#25584);
#21484=AXIS2_PLACEMENT_3D('',#55074,#25586,#25587);
#21485=AXIS2_PLACEMENT_3D('',#55075,#25588,#25589);
#21486=AXIS2_PLACEMENT_3D('',#55076,#25590,#25591);
#21487=AXIS2_PLACEMENT_3D('',#55171,#25593,#25594);
#21488=AXIS2_PLACEMENT_3D('',#55264,#25596,#25597);
#21489=AXIS2_PLACEMENT_3D('',#55266,#25598,#25599);
#21490=AXIS2_PLACEMENT_3D('',#55273,#25600,#25601);
#21491=AXIS2_PLACEMENT_3D('',#55359,#25603,#25604);
#21492=AXIS2_PLACEMENT_3D('',#55454,#25606,#25607);
#21493=AXIS2_PLACEMENT_3D('',#55455,#25608,#25609);
#21494=AXIS2_PLACEMENT_3D('',#55456,#25610,#25611);
#21495=AXIS2_PLACEMENT_3D('',#55551,#25613,#25614);
#21496=AXIS2_PLACEMENT_3D('',#55647,#25616,#25617);
#21497=AXIS2_PLACEMENT_3D('',#55649,#25618,#25619);
#21498=AXIS2_PLACEMENT_3D('',#55656,#25620,#25621);
#21499=AXIS2_PLACEMENT_3D('',#55742,#25623,#25624);
#21500=AXIS2_PLACEMENT_3D('',#55837,#25626,#25627);
#21501=AXIS2_PLACEMENT_3D('',#55838,#25628,#25629);
#21502=AXIS2_PLACEMENT_3D('',#55839,#25630,#25631);
#21503=AXIS2_PLACEMENT_3D('',#55934,#25633,#25634);
#21504=AXIS2_PLACEMENT_3D('',#56027,#25636,#25637);
#21505=AXIS2_PLACEMENT_3D('',#56029,#25638,#25639);
#21506=AXIS2_PLACEMENT_3D('',#56036,#25640,#25641);
#21507=AXIS2_PLACEMENT_3D('',#56122,#25643,#25644);
#21508=AXIS2_PLACEMENT_3D('',#56217,#25646,#25647);
#21509=AXIS2_PLACEMENT_3D('',#56218,#25648,#25649);
#21510=AXIS2_PLACEMENT_3D('',#56219,#25650,#25651);
#21511=AXIS2_PLACEMENT_3D('',#56314,#25653,#25654);
#21512=AXIS2_PLACEMENT_3D('',#56413,#25656,#25657);
#21513=AXIS2_PLACEMENT_3D('',#56415,#25658,#25659);
#21514=AXIS2_PLACEMENT_3D('',#56422,#25660,#25661);
#21515=AXIS2_PLACEMENT_3D('',#56508,#25663,#25664);
#21516=AXIS2_PLACEMENT_3D('',#56603,#25666,#25667);
#21517=AXIS2_PLACEMENT_3D('',#56604,#25668,#25669);
#21518=AXIS2_PLACEMENT_3D('',#56605,#25670,#25671);
#21519=AXIS2_PLACEMENT_3D('',#56698,#25673,#25674);
#21520=AXIS2_PLACEMENT_3D('',#56877,#25677,#25678);
#21521=AXIS2_PLACEMENT_3D('',#56985,#25680,#25681);
#21522=AXIS2_PLACEMENT_3D('',#56987,#25682,#25683);
#21523=AXIS2_PLACEMENT_3D('',#56992,#25684,#25685);
#21524=AXIS2_PLACEMENT_3D('',#56994,#25686,#25687);
#21525=AXIS2_PLACEMENT_3D('',#56999,#25688,#25689);
#21526=AXIS2_PLACEMENT_3D('',#57101,#25691,#25692);
#21527=AXIS2_PLACEMENT_3D('',#57183,#25694,#25695);
#21528=AXIS2_PLACEMENT_3D('',#57185,#25696,#25697);
#21529=AXIS2_PLACEMENT_3D('',#57190,#25698,#25699);
#21530=AXIS2_PLACEMENT_3D('',#57192,#25700,#25701);
#21531=AXIS2_PLACEMENT_3D('',#57197,#25702,#25703);
#21532=AXIS2_PLACEMENT_3D('',#57299,#25705,#25706);
#21533=AXIS2_PLACEMENT_3D('',#57381,#25708,#25709);
#21534=AXIS2_PLACEMENT_3D('',#57383,#25710,#25711);
#21535=AXIS2_PLACEMENT_3D('',#57388,#25712,#25713);
#21536=AXIS2_PLACEMENT_3D('',#57390,#25714,#25715);
#21537=AXIS2_PLACEMENT_3D('',#57395,#25716,#25717);
#21538=AXIS2_PLACEMENT_3D('',#57497,#25719,#25720);
#21539=AXIS2_PLACEMENT_3D('',#57579,#25722,#25723);
#21540=AXIS2_PLACEMENT_3D('',#57581,#25724,#25725);
#21541=AXIS2_PLACEMENT_3D('',#57586,#25726,#25727);
#21542=AXIS2_PLACEMENT_3D('',#57588,#25728,#25729);
#21543=AXIS2_PLACEMENT_3D('',#57593,#25730,#25731);
#21544=AXIS2_PLACEMENT_3D('',#57695,#25733,#25734);
#21545=AXIS2_PLACEMENT_3D('',#57777,#25736,#25737);
#21546=AXIS2_PLACEMENT_3D('',#57779,#25738,#25739);
#21547=AXIS2_PLACEMENT_3D('',#57784,#25740,#25741);
#21548=AXIS2_PLACEMENT_3D('',#57786,#25742,#25743);
#21549=AXIS2_PLACEMENT_3D('',#57791,#25744,#25745);
#21550=AXIS2_PLACEMENT_3D('',#57893,#25747,#25748);
#21551=AXIS2_PLACEMENT_3D('',#57975,#25750,#25751);
#21552=AXIS2_PLACEMENT_3D('',#57977,#25752,#25753);
#21553=AXIS2_PLACEMENT_3D('',#57988,#25754,#25755);
#21554=AXIS2_PLACEMENT_3D('',#57990,#25756,#25757);
#21555=AXIS2_PLACEMENT_3D('',#57995,#25758,#25759);
#21556=AXIS2_PLACEMENT_3D('',#58118,#25761,#25762);
#21557=AXIS2_PLACEMENT_3D('',#58200,#25764,#25765);
#21558=AXIS2_PLACEMENT_3D('',#58202,#25766,#25767);
#21559=AXIS2_PLACEMENT_3D('',#58207,#25768,#25769);
#21560=AXIS2_PLACEMENT_3D('',#58209,#25770,#25771);
#21561=AXIS2_PLACEMENT_3D('',#58214,#25772,#25773);
#21562=AXIS2_PLACEMENT_3D('',#58316,#25775,#25776);
#21563=AXIS2_PLACEMENT_3D('',#58398,#25778,#25779);
#21564=AXIS2_PLACEMENT_3D('',#58400,#25780,#25781);
#21565=AXIS2_PLACEMENT_3D('',#58405,#25782,#25783);
#21566=AXIS2_PLACEMENT_3D('',#58407,#25784,#25785);
#21567=AXIS2_PLACEMENT_3D('',#58412,#25786,#25787);
#21568=AXIS2_PLACEMENT_3D('',#58514,#25789,#25790);
#21569=AXIS2_PLACEMENT_3D('',#58596,#25792,#25793);
#21570=AXIS2_PLACEMENT_3D('',#58598,#25794,#25795);
#21571=AXIS2_PLACEMENT_3D('',#58603,#25796,#25797);
#21572=AXIS2_PLACEMENT_3D('',#58605,#25798,#25799);
#21573=AXIS2_PLACEMENT_3D('',#58610,#25800,#25801);
#21574=AXIS2_PLACEMENT_3D('',#58712,#25803,#25804);
#21575=AXIS2_PLACEMENT_3D('',#58794,#25806,#25807);
#21576=AXIS2_PLACEMENT_3D('',#58796,#25808,#25809);
#21577=AXIS2_PLACEMENT_3D('',#58801,#25810,#25811);
#21578=AXIS2_PLACEMENT_3D('',#58803,#25812,#25813);
#21579=AXIS2_PLACEMENT_3D('',#58808,#25814,#25815);
#21580=AXIS2_PLACEMENT_3D('',#58910,#25817,#25818);
#21581=AXIS2_PLACEMENT_3D('',#58992,#25820,#25821);
#21582=AXIS2_PLACEMENT_3D('',#58994,#25822,#25823);
#21583=AXIS2_PLACEMENT_3D('',#58999,#25824,#25825);
#21584=AXIS2_PLACEMENT_3D('',#59001,#25826,#25827);
#21585=AXIS2_PLACEMENT_3D('',#59006,#25828,#25829);
#21586=AXIS2_PLACEMENT_3D('',#59108,#25831,#25832);
#21587=AXIS2_PLACEMENT_3D('',#59190,#25834,#25835);
#21588=AXIS2_PLACEMENT_3D('',#59192,#25836,#25837);
#21589=AXIS2_PLACEMENT_3D('',#59203,#25838,#25839);
#21590=AXIS2_PLACEMENT_3D('',#59205,#25840,#25841);
#21591=AXIS2_PLACEMENT_3D('',#59210,#25842,#25843);
#21592=AXIS2_PLACEMENT_3D('',#59322,#25845,#25846);
#21593=AXIS2_PLACEMENT_3D('',#59404,#25848,#25849);
#21594=AXIS2_PLACEMENT_3D('',#59406,#25850,#25851);
#21595=AXIS2_PLACEMENT_3D('',#59417,#25852,#25853);
#21596=AXIS2_PLACEMENT_3D('',#59419,#25854,#25855);
#21597=AXIS2_PLACEMENT_3D('',#59424,#25856,#25857);
#21598=AXIS2_PLACEMENT_3D('',#59532,#25859,#25860);
#21599=AXIS2_PLACEMENT_3D('',#59614,#25862,#25863);
#21600=AXIS2_PLACEMENT_3D('',#59616,#25864,#25865);
#21601=AXIS2_PLACEMENT_3D('',#59621,#25866,#25867);
#21602=AXIS2_PLACEMENT_3D('',#59623,#25868,#25869);
#21603=AXIS2_PLACEMENT_3D('',#59628,#25870,#25871);
#21604=AXIS2_PLACEMENT_3D('',#59730,#25873,#25874);
#21605=AXIS2_PLACEMENT_3D('',#59812,#25876,#25877);
#21606=AXIS2_PLACEMENT_3D('',#59814,#25878,#25879);
#21607=AXIS2_PLACEMENT_3D('',#59819,#25880,#25881);
#21608=AXIS2_PLACEMENT_3D('',#59821,#25882,#25883);
#21609=AXIS2_PLACEMENT_3D('',#59826,#25884,#25885);
#21610=AXIS2_PLACEMENT_3D('',#59928,#25887,#25888);
#21611=AXIS2_PLACEMENT_3D('',#60010,#25890,#25891);
#21612=AXIS2_PLACEMENT_3D('',#60012,#25892,#25893);
#21613=AXIS2_PLACEMENT_3D('',#60017,#25894,#25895);
#21614=AXIS2_PLACEMENT_3D('',#60019,#25896,#25897);
#21615=AXIS2_PLACEMENT_3D('',#60024,#25898,#25899);
#21616=AXIS2_PLACEMENT_3D('',#60126,#25901,#25902);
#21617=AXIS2_PLACEMENT_3D('',#60208,#25904,#25905);
#21618=AXIS2_PLACEMENT_3D('',#60210,#25906,#25907);
#21619=AXIS2_PLACEMENT_3D('',#60215,#25908,#25909);
#21620=AXIS2_PLACEMENT_3D('',#60217,#25910,#25911);
#21621=AXIS2_PLACEMENT_3D('',#60222,#25912,#25913);
#21622=AXIS2_PLACEMENT_3D('',#60324,#25915,#25916);
#21623=AXIS2_PLACEMENT_3D('',#60406,#25918,#25919);
#21624=AXIS2_PLACEMENT_3D('',#60408,#25920,#25921);
#21625=AXIS2_PLACEMENT_3D('',#60419,#25922,#25923);
#21626=AXIS2_PLACEMENT_3D('',#60421,#25924,#25925);
#21627=AXIS2_PLACEMENT_3D('',#60426,#25926,#25927);
#21628=AXIS2_PLACEMENT_3D('',#60536,#25929,#25930);
#21629=AXIS2_PLACEMENT_3D('',#60618,#25932,#25933);
#21630=AXIS2_PLACEMENT_3D('',#60620,#25934,#25935);
#21631=AXIS2_PLACEMENT_3D('',#60631,#25936,#25937);
#21632=AXIS2_PLACEMENT_3D('',#60633,#25938,#25939);
#21633=AXIS2_PLACEMENT_3D('',#60638,#25940,#25941);
#21634=AXIS2_PLACEMENT_3D('',#60746,#25943,#25944);
#21635=AXIS2_PLACEMENT_3D('',#60828,#25946,#25947);
#21636=AXIS2_PLACEMENT_3D('',#60830,#25948,#25949);
#21637=AXIS2_PLACEMENT_3D('',#60835,#25950,#25951);
#21638=AXIS2_PLACEMENT_3D('',#60837,#25952,#25953);
#21639=AXIS2_PLACEMENT_3D('',#60842,#25954,#25955);
#21640=AXIS2_PLACEMENT_3D('',#60944,#25957,#25958);
#21641=AXIS2_PLACEMENT_3D('',#61026,#25960,#25961);
#21642=AXIS2_PLACEMENT_3D('',#61028,#25962,#25963);
#21643=AXIS2_PLACEMENT_3D('',#61033,#25964,#25965);
#21644=AXIS2_PLACEMENT_3D('',#61035,#25966,#25967);
#21645=AXIS2_PLACEMENT_3D('',#61040,#25968,#25969);
#21646=AXIS2_PLACEMENT_3D('',#61142,#25971,#25972);
#21647=AXIS2_PLACEMENT_3D('',#61224,#25974,#25975);
#21648=AXIS2_PLACEMENT_3D('',#61226,#25976,#25977);
#21649=AXIS2_PLACEMENT_3D('',#61231,#25978,#25979);
#21650=AXIS2_PLACEMENT_3D('',#61233,#25980,#25981);
#21651=AXIS2_PLACEMENT_3D('',#61238,#25982,#25983);
#21652=AXIS2_PLACEMENT_3D('',#61340,#25985,#25986);
#21653=AXIS2_PLACEMENT_3D('',#61422,#25988,#25989);
#21654=AXIS2_PLACEMENT_3D('',#61424,#25990,#25991);
#21655=AXIS2_PLACEMENT_3D('',#61429,#25992,#25993);
#21656=AXIS2_PLACEMENT_3D('',#61431,#25994,#25995);
#21657=AXIS2_PLACEMENT_3D('',#61436,#25996,#25997);
#21658=AXIS2_PLACEMENT_3D('',#61538,#25999,#26000);
#21659=AXIS2_PLACEMENT_3D('',#61620,#26002,#26003);
#21660=AXIS2_PLACEMENT_3D('',#61622,#26004,#26005);
#21661=AXIS2_PLACEMENT_3D('',#61627,#26006,#26007);
#21662=AXIS2_PLACEMENT_3D('',#61629,#26008,#26009);
#21663=AXIS2_PLACEMENT_3D('',#61634,#26010,#26011);
#21664=AXIS2_PLACEMENT_3D('',#61736,#26013,#26014);
#21665=AXIS2_PLACEMENT_3D('',#61818,#26016,#26017);
#21666=AXIS2_PLACEMENT_3D('',#61819,#26018,#26019);
#21667=AXIS2_PLACEMENT_3D('',#61820,#26020,#26021);
#21668=AXIS2_PLACEMENT_3D('',#61821,#26022,#26023);
#21669=AXIS2_PLACEMENT_3D('',#61822,#26024,#26025);
#21670=AXIS2_PLACEMENT_3D('',#61823,#26026,#26027);
#21671=AXIS2_PLACEMENT_3D('',#61824,#26028,#26029);
#21672=AXIS2_PLACEMENT_3D('',#61825,#26030,#26031);
#21673=AXIS2_PLACEMENT_3D('',#61826,#26032,#26033);
#21674=AXIS2_PLACEMENT_3D('',#61827,#26034,#26035);
#21675=AXIS2_PLACEMENT_3D('',#61829,#26036,#26037);
#21676=AXIS2_PLACEMENT_3D('',#61831,#26038,#26039);
#21677=AXIS2_PLACEMENT_3D('',#61833,#26040,#26041);
#21678=AXIS2_PLACEMENT_3D('',#61834,#26042,#26043);
#21679=AXIS2_PLACEMENT_3D('',#61835,#26044,#26045);
#21680=AXIS2_PLACEMENT_3D('',#61839,#26047,#26048);
#21681=AXIS2_PLACEMENT_3D('',#61840,#26049,#26050);
#21682=AXIS2_PLACEMENT_3D('',#61841,#26051,#26052);
#21683=AXIS2_PLACEMENT_3D('',#61842,#26053,#26054);
#21684=AXIS2_PLACEMENT_3D('',#61844,#26055,#26056);
#21685=AXIS2_PLACEMENT_3D('',#61846,#26057,#26058);
#21686=AXIS2_PLACEMENT_3D('',#61847,#26059,#26060);
#21687=AXIS2_PLACEMENT_3D('',#61848,#26061,#26062);
#21688=AXIS2_PLACEMENT_3D('',#61852,#26064,#26065);
#21689=AXIS2_PLACEMENT_3D('',#61853,#26066,#26067);
#21690=AXIS2_PLACEMENT_3D('',#61854,#26068,#26069);
#21691=AXIS2_PLACEMENT_3D('',#61856,#26070,#26071);
#21692=AXIS2_PLACEMENT_3D('',#61858,#26072,#26073);
#21693=AXIS2_PLACEMENT_3D('',#61859,#26074,#26075);
#21694=AXIS2_PLACEMENT_3D('',#61860,#26076,#26077);
#21695=AXIS2_PLACEMENT_3D('',#61864,#26079,#26080);
#21696=AXIS2_PLACEMENT_3D('',#61865,#26081,#26082);
#21697=AXIS2_PLACEMENT_3D('',#61866,#26083,#26084);
#21698=AXIS2_PLACEMENT_3D('',#61868,#26085,#26086);
#21699=AXIS2_PLACEMENT_3D('',#61869,#26087,#26088);
#21700=AXIS2_PLACEMENT_3D('',#61870,#26089,#26090);
#21701=AXIS2_PLACEMENT_3D('',#61871,#26091,#26092);
#21702=AXIS2_PLACEMENT_3D('',#61872,#26093,#26094);
#21703=AXIS2_PLACEMENT_3D('',#61875,#26095,#26096);
#21704=AXIS2_PLACEMENT_3D('',#61879,#26098,#26099);
#21705=AXIS2_PLACEMENT_3D('',#61881,#26101,#26102);
#21706=AXIS2_PLACEMENT_3D('',#61884,#26103,#26104);
#21707=AXIS2_PLACEMENT_3D('',#61885,#26105,#26106);
#21708=AXIS2_PLACEMENT_3D('',#61886,#26107,#26108);
#21709=AXIS2_PLACEMENT_3D('',#61887,#26109,#26110);
#21710=AXIS2_PLACEMENT_3D('',#61890,#26111,#26112);
#21711=AXIS2_PLACEMENT_3D('',#61893,#26115,#26116);
#21712=AXIS2_PLACEMENT_3D('',#61894,#26117,#26118);
#21713=AXIS2_PLACEMENT_3D('',#61895,#26119,#26120);
#21714=AXIS2_PLACEMENT_3D('',#61896,#26121,#26122);
#21715=AXIS2_PLACEMENT_3D('',#61900,#26124,#26125);
#21716=AXIS2_PLACEMENT_3D('',#61902,#26127,#26128);
#21717=AXIS2_PLACEMENT_3D('',#61906,#26131,#26132);
#21718=AXIS2_PLACEMENT_3D('',#61908,#26133,#26134);
#21719=AXIS2_PLACEMENT_3D('',#61909,#26135,#26136);
#21720=AXIS2_PLACEMENT_3D('',#61911,#26137,#26138);
#21721=AXIS2_PLACEMENT_3D('',#61913,#26139,#26140);
#21722=AXIS2_PLACEMENT_3D('',#61915,#26142,#26143);
#21723=AXIS2_PLACEMENT_3D('',#61918,#26144,#26145);
#21724=AXIS2_PLACEMENT_3D('',#61919,#26146,#26147);
#21725=AXIS2_PLACEMENT_3D('',#61920,#26148,#26149);
#21726=AXIS2_PLACEMENT_3D('',#61921,#26150,#26151);
#21727=AXIS2_PLACEMENT_3D('',#61923,#26152,#26153);
#21728=AXIS2_PLACEMENT_3D('',#61926,#26156,#26157);
#21729=AXIS2_PLACEMENT_3D('',#61927,#26158,#26159);
#21730=AXIS2_PLACEMENT_3D('',#61928,#26160,#26161);
#21731=AXIS2_PLACEMENT_3D('',#61930,#26163,#26164);
#21732=AXIS2_PLACEMENT_3D('',#61932,#26165,#26166);
#21733=AXIS2_PLACEMENT_3D('',#61933,#26167,#26168);
#21734=AXIS2_PLACEMENT_3D('',#61935,#26169,#26170);
#21735=AXIS2_PLACEMENT_3D('',#61936,#26171,#26172);
#21736=AXIS2_PLACEMENT_3D('',#61937,#26173,#26174);
#21737=AXIS2_PLACEMENT_3D('',#61941,#26176,#26177);
#21738=AXIS2_PLACEMENT_3D('',#61942,#26178,#26179);
#21739=AXIS2_PLACEMENT_3D('',#61943,#26180,#26181);
#21740=AXIS2_PLACEMENT_3D('',#61944,#26182,#26183);
#21741=AXIS2_PLACEMENT_3D('',#61945,#26184,#26185);
#21742=AXIS2_PLACEMENT_3D('',#61946,#26186,#26187);
#21743=AXIS2_PLACEMENT_3D('',#61947,#26188,#26189);
#21744=AXIS2_PLACEMENT_3D('',#61949,#26190,#26191);
#21745=AXIS2_PLACEMENT_3D('',#61951,#26192,#26193);
#21746=AXIS2_PLACEMENT_3D('',#61953,#26194,#26195);
#21747=AXIS2_PLACEMENT_3D('',#61954,#26196,#26197);
#21748=AXIS2_PLACEMENT_3D('',#61955,#26198,#26199);
#21749=AXIS2_PLACEMENT_3D('',#61959,#26201,#26202);
#21750=AXIS2_PLACEMENT_3D('',#61960,#26203,#26204);
#21751=AXIS2_PLACEMENT_3D('',#61961,#26205,#26206);
#21752=AXIS2_PLACEMENT_3D('',#61962,#26207,#26208);
#21753=AXIS2_PLACEMENT_3D('',#61964,#26209,#26210);
#21754=AXIS2_PLACEMENT_3D('',#61966,#26211,#26212);
#21755=AXIS2_PLACEMENT_3D('',#61967,#26213,#26214);
#21756=AXIS2_PLACEMENT_3D('',#61968,#26215,#26216);
#21757=AXIS2_PLACEMENT_3D('',#61972,#26218,#26219);
#21758=AXIS2_PLACEMENT_3D('',#61973,#26220,#26221);
#21759=AXIS2_PLACEMENT_3D('',#61974,#26222,#26223);
#21760=AXIS2_PLACEMENT_3D('',#61976,#26224,#26225);
#21761=AXIS2_PLACEMENT_3D('',#61978,#26226,#26227);
#21762=AXIS2_PLACEMENT_3D('',#61979,#26228,#26229);
#21763=AXIS2_PLACEMENT_3D('',#61980,#26230,#26231);
#21764=AXIS2_PLACEMENT_3D('',#61984,#26233,#26234);
#21765=AXIS2_PLACEMENT_3D('',#61985,#26235,#26236);
#21766=AXIS2_PLACEMENT_3D('',#61986,#26237,#26238);
#21767=AXIS2_PLACEMENT_3D('',#61988,#26239,#26240);
#21768=AXIS2_PLACEMENT_3D('',#61989,#26241,#26242);
#21769=AXIS2_PLACEMENT_3D('',#61990,#26243,#26244);
#21770=AXIS2_PLACEMENT_3D('',#61991,#26245,#26246);
#21771=AXIS2_PLACEMENT_3D('',#61992,#26247,#26248);
#21772=AXIS2_PLACEMENT_3D('',#61994,#26249,#26250);
#21773=AXIS2_PLACEMENT_3D('',#61996,#26251,#26252);
#21774=AXIS2_PLACEMENT_3D('',#61997,#26253,#26254);
#21775=AXIS2_PLACEMENT_3D('',#61998,#26255,#26256);
#21776=AXIS2_PLACEMENT_3D('',#61999,#26257,#26258);
#21777=AXIS2_PLACEMENT_3D('',#62000,#26259,#26260);
#21778=AXIS2_PLACEMENT_3D('',#62001,#26261,#26262);
#21779=AXIS2_PLACEMENT_3D('',#62022,#26264,#26265);
#21780=AXIS2_PLACEMENT_3D('',#62026,#26267,#26268);
#21781=AXIS2_PLACEMENT_3D('',#62028,#26270,#26271);
#21782=AXIS2_PLACEMENT_3D('',#62032,#26273,#26274);
#21783=AXIS2_PLACEMENT_3D('',#62035,#26276,#26277);
#21784=AXIS2_PLACEMENT_3D('',#62036,#26278,#26279);
#21785=AXIS2_PLACEMENT_3D('',#62039,#26280,#26281);
#21786=AXIS2_PLACEMENT_3D('',#62041,#26282,#26283);
#21787=AXIS2_PLACEMENT_3D('',#62042,#26284,#26285);
#21788=AXIS2_PLACEMENT_3D('',#62043,#26286,#26287);
#21789=AXIS2_PLACEMENT_3D('',#62046,#26290,#26291);
#21790=AXIS2_PLACEMENT_3D('',#62049,#26292,#26293);
#21791=AXIS2_PLACEMENT_3D('',#62052,#26296,#26297);
#21792=AXIS2_PLACEMENT_3D('',#62054,#26298,#26299);
#21793=AXIS2_PLACEMENT_3D('',#62055,#26300,#26301);
#21794=AXIS2_PLACEMENT_3D('',#62056,#26302,#26303);
#21795=AXIS2_PLACEMENT_3D('',#62059,#26304,#26305);
#21796=AXIS2_PLACEMENT_3D('',#62061,#26306,#26307);
#21797=AXIS2_PLACEMENT_3D('',#62062,#26308,#26309);
#21798=AXIS2_PLACEMENT_3D('',#62063,#26310,#26311);
#21799=AXIS2_PLACEMENT_3D('',#62066,#26314,#26315);
#21800=AXIS2_PLACEMENT_3D('',#62067,#26316,#26317);
#21801=AXIS2_PLACEMENT_3D('',#62068,#26318,#26319);
#21802=AXIS2_PLACEMENT_3D('',#62072,#26321,#26322);
#21803=AXIS2_PLACEMENT_3D('',#62075,#26324,#26325);
#21804=AXIS2_PLACEMENT_3D('',#62076,#26326,#26327);
#21805=AXIS2_PLACEMENT_3D('',#62079,#26330,#26331);
#21806=AXIS2_PLACEMENT_3D('',#62081,#26333,#26334);
#21807=AXIS2_PLACEMENT_3D('',#62082,#26335,#26336);
#21808=AXIS2_PLACEMENT_3D('',#62086,#26338,#26339);
#21809=AXIS2_PLACEMENT_3D('',#62088,#26341,#26342);
#21810=AXIS2_PLACEMENT_3D('',#62090,#26343,#26344);
#21811=AXIS2_PLACEMENT_3D('',#62091,#26345,#26346);
#21812=AXIS2_PLACEMENT_3D('',#62092,#26347,#26348);
#21813=AXIS2_PLACEMENT_3D('',#62094,#26350,#26351);
#21814=AXIS2_PLACEMENT_3D('',#62097,#26354,#26355);
#21815=AXIS2_PLACEMENT_3D('',#62098,#26356,#26357);
#21816=AXIS2_PLACEMENT_3D('',#62100,#26358,#26359);
#21817=AXIS2_PLACEMENT_3D('',#62102,#26361,#26362);
#21818=AXIS2_PLACEMENT_3D('',#62123,#26364,#26365);
#21819=AXIS2_PLACEMENT_3D('',#62127,#26367,#26368);
#21820=AXIS2_PLACEMENT_3D('',#62129,#26370,#26371);
#21821=AXIS2_PLACEMENT_3D('',#62132,#26372,#26373);
#21822=AXIS2_PLACEMENT_3D('',#62136,#26375,#26376);
#21823=AXIS2_PLACEMENT_3D('',#62138,#26378,#26379);
#21824=AXIS2_PLACEMENT_3D('',#62140,#26380,#26381);
#21825=AXIS2_PLACEMENT_3D('',#62141,#26382,#26383);
#21826=AXIS2_PLACEMENT_3D('',#62142,#26384,#26385);
#21827=AXIS2_PLACEMENT_3D('',#62146,#26387,#26388);
#21828=AXIS2_PLACEMENT_3D('',#62149,#26390,#26391);
#21829=AXIS2_PLACEMENT_3D('',#62150,#26392,#26393);
#21830=AXIS2_PLACEMENT_3D('',#62153,#26395,#26396);
#21831=AXIS2_PLACEMENT_3D('',#62155,#26398,#26399);
#21832=AXIS2_PLACEMENT_3D('',#62156,#26400,#26401);
#21833=AXIS2_PLACEMENT_3D('',#62157,#26402,#26403);
#21834=AXIS2_PLACEMENT_3D('',#62158,#26404,#26405);
#21835=AXIS2_PLACEMENT_3D('',#62159,#26406,#26407);
#21836=AXIS2_PLACEMENT_3D('',#62163,#26409,#26410);
#21837=AXIS2_PLACEMENT_3D('',#62166,#26412,#26413);
#21838=AXIS2_PLACEMENT_3D('',#62167,#26414,#26415);
#21839=AXIS2_PLACEMENT_3D('',#62170,#26418,#26419);
#21840=AXIS2_PLACEMENT_3D('',#62172,#26421,#26422);
#21841=AXIS2_PLACEMENT_3D('',#62175,#26423,#26424);
#21842=AXIS2_PLACEMENT_3D('',#62177,#26425,#26426);
#21843=AXIS2_PLACEMENT_3D('',#62178,#26427,#26428);
#21844=AXIS2_PLACEMENT_3D('',#62179,#26429,#26430);
#21845=AXIS2_PLACEMENT_3D('',#62182,#26431,#26432);
#21846=AXIS2_PLACEMENT_3D('',#62185,#26435,#26436);
#21847=AXIS2_PLACEMENT_3D('',#62187,#26437,#26438);
#21848=AXIS2_PLACEMENT_3D('',#62188,#26439,#26440);
#21849=AXIS2_PLACEMENT_3D('',#62189,#26441,#26442);
#21850=AXIS2_PLACEMENT_3D('',#62191,#26444,#26445);
#21851=AXIS2_PLACEMENT_3D('',#62194,#26448,#26449);
#21852=AXIS2_PLACEMENT_3D('',#62197,#26452,#26453);
#21853=AXIS2_PLACEMENT_3D('',#62198,#26454,#26455);
#21854=AXIS2_PLACEMENT_3D('',#62200,#26456,#26457);
#21855=AXIS2_PLACEMENT_3D('',#62202,#26458,#26459);
#21856=AXIS2_PLACEMENT_3D('',#62204,#26461,#26462);
#21857=AXIS2_PLACEMENT_3D('',#62207,#26463,#26464);
#21858=AXIS2_PLACEMENT_3D('',#62211,#26466,#26467);
#21859=AXIS2_PLACEMENT_3D('',#62213,#26469,#26470);
#21860=AXIS2_PLACEMENT_3D('',#62215,#26471,#26472);
#21861=AXIS2_PLACEMENT_3D('',#62216,#26473,#26474);
#21862=AXIS2_PLACEMENT_3D('',#62217,#26475,#26476);
#21863=AXIS2_PLACEMENT_3D('',#62219,#26477,#26478);
#21864=AXIS2_PLACEMENT_3D('',#62220,#26479,#26480);
#21865=AXIS2_PLACEMENT_3D('',#62221,#26481,#26482);
#21866=AXIS2_PLACEMENT_3D('',#62225,#26484,#26485);
#21867=AXIS2_PLACEMENT_3D('',#62227,#26487,#26488);
#21868=AXIS2_PLACEMENT_3D('',#62231,#26490,#26491);
#21869=AXIS2_PLACEMENT_3D('',#62233,#26493,#26494);
#21870=AXIS2_PLACEMENT_3D('',#62237,#26497,#26498);
#21871=AXIS2_PLACEMENT_3D('',#62257,#26500,#26501);
#21872=AXIS2_PLACEMENT_3D('',#62261,#26503,#26504);
#21873=AXIS2_PLACEMENT_3D('',#62263,#26506,#26507);
#21874=AXIS2_PLACEMENT_3D('',#62264,#26508,#26509);
#21875=AXIS2_PLACEMENT_3D('',#62268,#26511,#26512);
#21876=AXIS2_PLACEMENT_3D('',#62270,#26514,#26515);
#21877=AXIS2_PLACEMENT_3D('',#62273,#26516,#26517);
#21878=AXIS2_PLACEMENT_3D('',#62276,#26519,#26520);
#21879=AXIS2_PLACEMENT_3D('',#62296,#26523,#26524);
#21880=AXIS2_PLACEMENT_3D('',#62297,#26525,#26526);
#21881=AXIS2_PLACEMENT_3D('',#62298,#26527,#26528);
#21882=AXIS2_PLACEMENT_3D('',#62299,#26529,#26530);
#21883=AXIS2_PLACEMENT_3D('',#62302,#26532,#26533);
#21884=AXIS2_PLACEMENT_3D('',#62305,#26535,#26536);
#21885=AXIS2_PLACEMENT_3D('',#62306,#26537,#26538);
#21886=AXIS2_PLACEMENT_3D('',#62307,#26539,#26540);
#21887=AXIS2_PLACEMENT_3D('',#62309,#26542,#26543);
#21888=AXIS2_PLACEMENT_3D('',#62311,#26545,#26546);
#21889=AXIS2_PLACEMENT_3D('',#62315,#26549,#26550);
#21890=AXIS2_PLACEMENT_3D('',#62317,#26551,#26552);
#21891=AXIS2_PLACEMENT_3D('',#62320,#26554,#26555);
#21892=AXIS2_PLACEMENT_3D('',#62321,#26556,#26557);
#21893=AXIS2_PLACEMENT_3D('',#62330,#26558,#26559);
#21894=AXIS2_PLACEMENT_3D('',#62332,#26560,#26561);
#21895=AXIS2_PLACEMENT_3D('',#62333,#26562,#26563);
#21896=AXIS2_PLACEMENT_3D('',#62334,#26564,#26565);
#21897=AXIS2_PLACEMENT_3D('',#62335,#26566,#26567);
#21898=AXIS2_PLACEMENT_3D('',#62337,#26568,#26569);
#21899=AXIS2_PLACEMENT_3D('',#62361,#26570,#26571);
#21900=AXIS2_PLACEMENT_3D('',#62385,#26572,#26573);
#21901=AXIS2_PLACEMENT_3D('',#62392,#26574,#26575);
#21902=AXIS2_PLACEMENT_3D('',#62393,#26576,#26577);
#21903=AXIS2_PLACEMENT_3D('',#62397,#26579,#26580);
#21904=AXIS2_PLACEMENT_3D('',#62401,#26582,#26583);
#21905=AXIS2_PLACEMENT_3D('',#62409,#26590,#26591);
#21906=AXIS2_PLACEMENT_3D('',#62410,#26592,#26593);
#21907=AXIS2_PLACEMENT_3D('',#62414,#26595,#26596);
#21908=AXIS2_PLACEMENT_3D('',#62415,#26597,#26598);
#21909=AXIS2_PLACEMENT_3D('',#62416,#26599,#26600);
#21910=AXIS2_PLACEMENT_3D('',#62418,#26601,#26602);
#21911=AXIS2_PLACEMENT_3D('',#62420,#26603,#26604);
#21912=AXIS2_PLACEMENT_3D('',#62422,#26605,#26606);
#21913=AXIS2_PLACEMENT_3D('',#62423,#26607,#26608);
#21914=AXIS2_PLACEMENT_3D('',#62424,#26609,#26610);
#21915=AXIS2_PLACEMENT_3D('',#62428,#26612,#26613);
#21916=AXIS2_PLACEMENT_3D('',#62429,#26614,#26615);
#21917=AXIS2_PLACEMENT_3D('',#62430,#26616,#26617);
#21918=AXIS2_PLACEMENT_3D('',#62432,#26618,#26619);
#21919=AXIS2_PLACEMENT_3D('',#62433,#26620,#26621);
#21920=AXIS2_PLACEMENT_3D('',#62434,#26622,#26623);
#21921=AXIS2_PLACEMENT_3D('',#62435,#26624,#26625);
#21922=AXIS2_PLACEMENT_3D('',#62436,#26626,#26627);
#21923=AXIS2_PLACEMENT_3D('',#62437,#26628,#26629);
#21924=AXIS2_PLACEMENT_3D('',#62439,#26631,#26632);
#21925=AXIS2_PLACEMENT_3D('',#62440,#26633,#26634);
#21926=AXIS2_PLACEMENT_3D('',#62441,#26635,#26636);
#21927=AXIS2_PLACEMENT_3D('',#62442,#26637,#26638);
#21928=AXIS2_PLACEMENT_3D('',#62443,#26639,#26640);
#21929=AXIS2_PLACEMENT_3D('',#62445,#26641,#26642);
#21930=AXIS2_PLACEMENT_3D('',#62449,#26644,#26645);
#21931=AXIS2_PLACEMENT_3D('',#62451,#26647,#26648);
#21932=AXIS2_PLACEMENT_3D('',#62453,#26649,#26650);
#21933=AXIS2_PLACEMENT_3D('',#62457,#26652,#26653);
#21934=AXIS2_PLACEMENT_3D('',#62459,#26655,#26656);
#21935=AXIS2_PLACEMENT_3D('',#62461,#26657,#26658);
#21936=AXIS2_PLACEMENT_3D('',#62465,#26660,#26661);
#21937=AXIS2_PLACEMENT_3D('',#62467,#26663,#26664);
#21938=AXIS2_PLACEMENT_3D('',#62469,#26665,#26666);
#21939=AXIS2_PLACEMENT_3D('',#62470,#26667,#26668);
#21940=AXIS2_PLACEMENT_3D('',#62471,#26669,#26670);
#21941=AXIS2_PLACEMENT_3D('',#62472,#26671,#26672);
#21942=AXIS2_PLACEMENT_3D('',#62473,#26673,#26674);
#21943=AXIS2_PLACEMENT_3D('',#62474,#26675,#26676);
#21944=AXIS2_PLACEMENT_3D('',#62475,#26677,#26678);
#21945=AXIS2_PLACEMENT_3D('',#62479,#26681,#26682);
#21946=AXIS2_PLACEMENT_3D('',#62482,#26684,#26685);
#21947=AXIS2_PLACEMENT_3D('',#62483,#26686,#26687);
#21948=AXIS2_PLACEMENT_3D('',#62487,#26690,#26691);
#21949=AXIS2_PLACEMENT_3D('',#62490,#26693,#26694);
#21950=AXIS2_PLACEMENT_3D('',#62491,#26695,#26696);
#21951=AXIS2_PLACEMENT_3D('',#62495,#26699,#26700);
#21952=AXIS2_PLACEMENT_3D('',#62497,#26701,#26702);
#21953=AXIS2_PLACEMENT_3D('',#62499,#26703,#26704);
#21954=AXIS2_PLACEMENT_3D('',#62500,#26705,#26706);
#21955=AXIS2_PLACEMENT_3D('',#62501,#26707,#26708);
#21956=AXIS2_PLACEMENT_3D('',#62505,#26710,#26711);
#21957=AXIS2_PLACEMENT_3D('',#62506,#26712,#26713);
#21958=AXIS2_PLACEMENT_3D('',#62507,#26714,#26715);
#21959=AXIS2_PLACEMENT_3D('',#62509,#26716,#26717);
#21960=AXIS2_PLACEMENT_3D('',#62511,#26718,#26719);
#21961=AXIS2_PLACEMENT_3D('',#62512,#26720,#26721);
#21962=AXIS2_PLACEMENT_3D('',#62513,#26722,#26723);
#21963=AXIS2_PLACEMENT_3D('',#62515,#26725,#26726);
#21964=AXIS2_PLACEMENT_3D('',#62517,#26727,#26728);
#21965=AXIS2_PLACEMENT_3D('',#62518,#26729,#26730);
#21966=AXIS2_PLACEMENT_3D('',#62519,#26731,#26732);
#21967=AXIS2_PLACEMENT_3D('',#62521,#26733,#26734);
#21968=AXIS2_PLACEMENT_3D('',#62522,#26735,#26736);
#21969=AXIS2_PLACEMENT_3D('',#62523,#26737,#26738);
#21970=AXIS2_PLACEMENT_3D('',#62525,#26739,#26740);
#21971=AXIS2_PLACEMENT_3D('',#62526,#26741,#26742);
#21972=AXIS2_PLACEMENT_3D('',#62528,#26743,#26744);
#21973=AXIS2_PLACEMENT_3D('',#62531,#26746,#26747);
#21974=AXIS2_PLACEMENT_3D('',#62532,#26748,#26749);
#21975=AXIS2_PLACEMENT_3D('',#62533,#26750,#26751);
#21976=AXIS2_PLACEMENT_3D('',#62534,#26752,#26753);
#21977=AXIS2_PLACEMENT_3D('',#62538,#26755,#26756);
#21978=AXIS2_PLACEMENT_3D('',#62540,#26758,#26759);
#21979=AXIS2_PLACEMENT_3D('',#62544,#26762,#26763);
#21980=AXIS2_PLACEMENT_3D('',#62545,#26764,#26765);
#21981=AXIS2_PLACEMENT_3D('',#62546,#26766,#26767);
#21982=AXIS2_PLACEMENT_3D('',#62548,#26769,#26770);
#21983=AXIS2_PLACEMENT_3D('',#62549,#26771,#26772);
#21984=AXIS2_PLACEMENT_3D('',#62550,#26773,#26774);
#21985=AXIS2_PLACEMENT_3D('',#62552,#26776,#26777);
#21986=AXIS2_PLACEMENT_3D('',#62553,#26778,#26779);
#21987=AXIS2_PLACEMENT_3D('',#62554,#26780,#26781);
#21988=AXIS2_PLACEMENT_3D('',#62555,#26782,#26783);
#21989=AXIS2_PLACEMENT_3D('',#62556,#26784,#26785);
#21990=AXIS2_PLACEMENT_3D('',#62558,#26787,#26788);
#21991=AXIS2_PLACEMENT_3D('',#62560,#26789,#26790);
#21992=AXIS2_PLACEMENT_3D('',#62562,#26791,#26792);
#21993=AXIS2_PLACEMENT_3D('',#62563,#26793,#26794);
#21994=AXIS2_PLACEMENT_3D('',#62564,#26795,#26796);
#21995=AXIS2_PLACEMENT_3D('',#62567,#26797,#26798);
#21996=AXIS2_PLACEMENT_3D('',#62569,#26800,#26801);
#21997=AXIS2_PLACEMENT_3D('',#62570,#26802,#26803);
#21998=AXIS2_PLACEMENT_3D('',#62572,#26804,#26805);
#21999=AXIS2_PLACEMENT_3D('',#62573,#26806,#26807);
#22000=AXIS2_PLACEMENT_3D('',#62574,#26808,#26809);
#22001=AXIS2_PLACEMENT_3D('',#62576,#26810,#26811);
#22002=AXIS2_PLACEMENT_3D('',#62577,#26812,#26813);
#22003=AXIS2_PLACEMENT_3D('',#62579,#26815,#26816);
#22004=AXIS2_PLACEMENT_3D('',#62580,#26817,#26818);
#22005=AXIS2_PLACEMENT_3D('',#62581,#26819,#26820);
#22006=AXIS2_PLACEMENT_3D('',#62582,#26821,#26822);
#22007=AXIS2_PLACEMENT_3D('',#62583,#26823,#26824);
#22008=AXIS2_PLACEMENT_3D('',#62584,#26825,#26826);
#22009=AXIS2_PLACEMENT_3D('',#62585,#26827,#26828);
#22010=AXIS2_PLACEMENT_3D('',#62586,#26829,#26830);
#22011=AXIS2_PLACEMENT_3D('',#62593,#26834,#26835);
#22012=AXIS2_PLACEMENT_3D('',#62600,#26839,#26840);
#22013=AXIS2_PLACEMENT_3D('',#62607,#26844,#26845);
#22014=AXIS2_PLACEMENT_3D('',#62614,#26849,#26850);
#22015=AXIS2_PLACEMENT_3D('',#62617,#26853,#26854);
#22016=AXIS2_PLACEMENT_3D('',#62624,#26858,#26859);
#22017=AXIS2_PLACEMENT_3D('',#62631,#26863,#26864);
#22018=AXIS2_PLACEMENT_3D('',#62634,#26867,#26868);
#22019=AXIS2_PLACEMENT_3D('',#62641,#26872,#26873);
#22020=AXIS2_PLACEMENT_3D('',#62644,#26876,#26877);
#22021=AXIS2_PLACEMENT_3D('',#62647,#26880,#26881);
#22022=AXIS2_PLACEMENT_3D('',#62654,#26885,#26886);
#22023=AXIS2_PLACEMENT_3D('',#62657,#26889,#26890);
#22024=AXIS2_PLACEMENT_3D('',#62660,#26893,#26894);
#22025=AXIS2_PLACEMENT_3D('',#62663,#26897,#26898);
#22026=AXIS2_PLACEMENT_3D('',#62666,#26901,#26902);
#22027=AXIS2_PLACEMENT_3D('',#62669,#26905,#26906);
#22028=AXIS2_PLACEMENT_3D('',#62672,#26909,#26910);
#22029=AXIS2_PLACEMENT_3D('',#62675,#26913,#26914);
#22030=AXIS2_PLACEMENT_3D('',#62678,#26917,#26918);
#22031=AXIS2_PLACEMENT_3D('',#62679,#26919,#26920);
#22032=AXIS2_PLACEMENT_3D('',#62680,#26921,#26922);
#22033=AXIS2_PLACEMENT_3D('',#62681,#26923,#26924);
#22034=AXIS2_PLACEMENT_3D('',#62682,#26925,#26926);
#22035=AXIS2_PLACEMENT_3D('',#62683,#26927,#26928);
#22036=AXIS2_PLACEMENT_3D('',#62684,#26929,#26930);
#22037=AXIS2_PLACEMENT_3D('',#63446,#26931,#26932);
#22038=AXIS2_PLACEMENT_3D('',#63524,#26933,#26934);
#22039=AXIS2_PLACEMENT_3D('',#63525,#26935,#26936);
#22040=AXIS2_PLACEMENT_3D('',#63526,#26937,#26938);
#22041=AXIS2_PLACEMENT_3D('',#63527,#26939,#26940);
#22042=AXIS2_PLACEMENT_3D('',#63528,#26941,#26942);
#22043=AXIS2_PLACEMENT_3D('',#63530,#26943,#26944);
#22044=AXIS2_PLACEMENT_3D('',#63532,#26945,#26946);
#22045=AXIS2_PLACEMENT_3D('',#63534,#26947,#26948);
#22046=AXIS2_PLACEMENT_3D('',#63535,#26949,#26950);
#22047=AXIS2_PLACEMENT_3D('',#63536,#26951,#26952);
#22048=AXIS2_PLACEMENT_3D('',#63539,#26953,#26954);
#22049=AXIS2_PLACEMENT_3D('',#63540,#26955,#26956);
#22050=AXIS2_PLACEMENT_3D('',#63542,#26958,#26959);
#22051=AXIS2_PLACEMENT_3D('',#63547,#26961,#26962);
#22052=AXIS2_PLACEMENT_3D('',#63549,#26963,#26964);
#22053=AXIS2_PLACEMENT_3D('',#63551,#26965,#26966);
#22054=AXIS2_PLACEMENT_3D('',#63559,#26970,#26971);
#22055=AXIS2_PLACEMENT_3D('',#63561,#26972,#26973);
#22056=AXIS2_PLACEMENT_3D('',#63563,#26974,#26975);
#22057=AXIS2_PLACEMENT_3D('',#63565,#26976,#26977);
#22058=AXIS2_PLACEMENT_3D('',#63573,#26981,#26982);
#22059=AXIS2_PLACEMENT_3D('',#63575,#26983,#26984);
#22060=AXIS2_PLACEMENT_3D('',#63577,#26985,#26986);
#22061=AXIS2_PLACEMENT_3D('',#63585,#26990,#26991);
#22062=AXIS2_PLACEMENT_3D('',#63587,#26992,#26993);
#22063=AXIS2_PLACEMENT_3D('',#63589,#26994,#26995);
#22064=AXIS2_PLACEMENT_3D('',#63593,#26998,#26999);
#22065=AXIS2_PLACEMENT_3D('',#63595,#27000,#27001);
#22066=AXIS2_PLACEMENT_3D('',#63596,#27002,#27003);
#22067=AXIS2_PLACEMENT_3D('',#63597,#27004,#27005);
#22068=AXIS2_PLACEMENT_3D('',#63602,#27007,#27008);
#22069=AXIS2_PLACEMENT_3D('',#63610,#27012,#27013);
#22070=AXIS2_PLACEMENT_3D('',#63618,#27017,#27018);
#22071=AXIS2_PLACEMENT_3D('',#63620,#27019,#27020);
#22072=AXIS2_PLACEMENT_3D('',#63628,#27024,#27025);
#22073=AXIS2_PLACEMENT_3D('',#63630,#27026,#27027);
#22074=AXIS2_PLACEMENT_3D('',#63634,#27030,#27031);
#22075=AXIS2_PLACEMENT_3D('',#63636,#27032,#27033);
#22076=AXIS2_PLACEMENT_3D('',#63639,#27035,#27036);
#22077=AXIS2_PLACEMENT_3D('',#63640,#27037,#27038);
#22078=AXIS2_PLACEMENT_3D('',#63646,#27042,#27043);
#22079=AXIS2_PLACEMENT_3D('',#63647,#27044,#27045);
#22080=AXIS2_PLACEMENT_3D('',#63648,#27046,#27047);
#22081=AXIS2_PLACEMENT_3D('',#63649,#27048,#27049);
#22082=AXIS2_PLACEMENT_3D('',#63651,#27050,#27051);
#22083=AXIS2_PLACEMENT_3D('',#63654,#27053,#27054);
#22084=AXIS2_PLACEMENT_3D('',#63655,#27055,#27056);
#22085=AXIS2_PLACEMENT_3D('',#63661,#27060,#27061);
#22086=AXIS2_PLACEMENT_3D('',#63662,#27062,#27063);
#22087=AXIS2_PLACEMENT_3D('',#63663,#27064,#27065);
#22088=AXIS2_PLACEMENT_3D('',#63664,#27066,#27067);
#22089=AXIS2_PLACEMENT_3D('',#63666,#27068,#27069);
#22090=AXIS2_PLACEMENT_3D('',#63669,#27071,#27072);
#22091=AXIS2_PLACEMENT_3D('',#63670,#27073,#27074);
#22092=AXIS2_PLACEMENT_3D('',#63676,#27078,#27079);
#22093=AXIS2_PLACEMENT_3D('',#63677,#27080,#27081);
#22094=AXIS2_PLACEMENT_3D('',#63678,#27082,#27083);
#22095=AXIS2_PLACEMENT_3D('',#63679,#27084,#27085);
#22096=AXIS2_PLACEMENT_3D('',#63682,#27086,#27087);
#22097=AXIS2_PLACEMENT_3D('',#63684,#27088,#27089);
#22098=AXIS2_PLACEMENT_3D('',#63686,#27090,#27091);
#22099=AXIS2_PLACEMENT_3D('',#63687,#27092,#27093);
#22100=AXIS2_PLACEMENT_3D('',#63688,#27094,#27095);
#22101=AXIS2_PLACEMENT_3D('',#63690,#27096,#27097);
#22102=AXIS2_PLACEMENT_3D('',#63691,#27098,#27099);
#22103=AXIS2_PLACEMENT_3D('',#63692,#27100,#27101);
#22104=AXIS2_PLACEMENT_3D('',#63694,#27102,#27103);
#22105=AXIS2_PLACEMENT_3D('',#63698,#27105,#27106);
#22106=AXIS2_PLACEMENT_3D('',#63700,#27108,#27109);
#22107=AXIS2_PLACEMENT_3D('',#63702,#27110,#27111);
#22108=AXIS2_PLACEMENT_3D('',#63703,#27112,#27113);
#22109=AXIS2_PLACEMENT_3D('',#63704,#27114,#27115);
#22110=AXIS2_PLACEMENT_3D('',#63705,#27116,#27117);
#22111=AXIS2_PLACEMENT_3D('',#63706,#27118,#27119);
#22112=AXIS2_PLACEMENT_3D('',#63710,#27121,#27122);
#22113=AXIS2_PLACEMENT_3D('',#63742,#27124,#27125);
#22114=AXIS2_PLACEMENT_3D('',#63747,#27126,#27127);
#22115=AXIS2_PLACEMENT_3D('',#63753,#27128,#27129);
#22116=AXIS2_PLACEMENT_3D('',#63783,#27130,#27131);
#22117=AXIS2_PLACEMENT_3D('',#63784,#27132,#27133);
#22118=AXIS2_PLACEMENT_3D('',#63795,#27137,#27138);
#22119=AXIS2_PLACEMENT_3D('',#63814,#27140,#27141);
#22120=AXIS2_PLACEMENT_3D('',#63815,#27142,#27143);
#22121=AXIS2_PLACEMENT_3D('',#63816,#27144,#27145);
#22122=AXIS2_PLACEMENT_3D('',#63817,#27146,#27147);
#22123=AXIS2_PLACEMENT_3D('',#63818,#27148,#27149);
#22124=AXIS2_PLACEMENT_3D('',#63819,#27150,#27151);
#22125=AXIS2_PLACEMENT_3D('',#63820,#27152,#27153);
#22126=AXIS2_PLACEMENT_3D('',#63822,#27154,#27155);
#22127=AXIS2_PLACEMENT_3D('',#63823,#27156,#27157);
#22128=AXIS2_PLACEMENT_3D('',#63824,#27158,#27159);
#22129=AXIS2_PLACEMENT_3D('',#63827,#27160,#27161);
#22130=AXIS2_PLACEMENT_3D('',#63831,#27163,#27164);
#22131=AXIS2_PLACEMENT_3D('',#63835,#27166,#27167);
#22132=AXIS2_PLACEMENT_3D('',#63839,#27169,#27170);
#22133=AXIS2_PLACEMENT_3D('',#63843,#27172,#27173);
#22134=AXIS2_PLACEMENT_3D('',#63847,#27175,#27176);
#22135=AXIS2_PLACEMENT_3D('',#63851,#27178,#27179);
#22136=AXIS2_PLACEMENT_3D('',#63855,#27181,#27182);
#22137=AXIS2_PLACEMENT_3D('',#63857,#27184,#27185);
#22138=AXIS2_PLACEMENT_3D('',#63858,#27186,#27187);
#22139=AXIS2_PLACEMENT_3D('',#63859,#27188,#27189);
#22140=AXIS2_PLACEMENT_3D('',#63862,#27190,#27191);
#22141=AXIS2_PLACEMENT_3D('',#63865,#27193,#27194);
#22142=AXIS2_PLACEMENT_3D('',#63880,#27195,#27196);
#22143=AXIS2_PLACEMENT_3D('',#63882,#27197,#27198);
#22144=AXIS2_PLACEMENT_3D('',#63883,#27199,#27200);
#22145=AXIS2_PLACEMENT_3D('',#63884,#27201,#27202);
#22146=AXIS2_PLACEMENT_3D('',#63887,#27203,#27204);
#22147=AXIS2_PLACEMENT_3D('',#63889,#27205,#27206);
#22148=AXIS2_PLACEMENT_3D('',#63890,#27207,#27208);
#22149=AXIS2_PLACEMENT_3D('',#63923,#27209,#27210);
#22150=AXIS2_PLACEMENT_3D('',#63925,#27211,#27212);
#22151=AXIS2_PLACEMENT_3D('',#63926,#27213,#27214);
#22152=AXIS2_PLACEMENT_3D('',#63927,#27215,#27216);
#22153=AXIS2_PLACEMENT_3D('',#63929,#27217,#27218);
#22154=AXIS2_PLACEMENT_3D('',#63934,#27219,#27220);
#22155=AXIS2_PLACEMENT_3D('',#63936,#27221,#27222);
#22156=AXIS2_PLACEMENT_3D('',#63937,#27223,#27224);
#22157=AXIS2_PLACEMENT_3D('',#63938,#27225,#27226);
#22158=AXIS2_PLACEMENT_3D('',#63954,#27227,#27228);
#22159=AXIS2_PLACEMENT_3D('',#63955,#27229,#27230);
#22160=AXIS2_PLACEMENT_3D('',#63957,#27231,#27232);
#22161=AXIS2_PLACEMENT_3D('',#63961,#27234,#27235);
#22162=AXIS2_PLACEMENT_3D('',#63963,#27237,#27238);
#22163=AXIS2_PLACEMENT_3D('',#63966,#27239,#27240);
#22164=AXIS2_PLACEMENT_3D('',#63968,#27241,#27242);
#22165=AXIS2_PLACEMENT_3D('',#63969,#27243,#27244);
#22166=AXIS2_PLACEMENT_3D('',#63970,#27245,#27246);
#22167=AXIS2_PLACEMENT_3D('',#63972,#27247,#27248);
#22168=AXIS2_PLACEMENT_3D('',#63974,#27249,#27250);
#22169=AXIS2_PLACEMENT_3D('',#63975,#27251,#27252);
#22170=AXIS2_PLACEMENT_3D('',#63976,#27253,#27254);
#22171=AXIS2_PLACEMENT_3D('',#63978,#27255,#27256);
#22172=AXIS2_PLACEMENT_3D('',#63979,#27257,#27258);
#22173=AXIS2_PLACEMENT_3D('',#63980,#27259,#27260);
#22174=AXIS2_PLACEMENT_3D('',#63982,#27261,#27262);
#22175=AXIS2_PLACEMENT_3D('',#63983,#27263,#27264);
#22176=AXIS2_PLACEMENT_3D('',#63984,#27265,#27266);
#22177=AXIS2_PLACEMENT_3D('',#63987,#27267,#27268);
#22178=AXIS2_PLACEMENT_3D('',#63989,#27269,#27270);
#22179=AXIS2_PLACEMENT_3D('',#63990,#27271,#27272);
#22180=AXIS2_PLACEMENT_3D('',#64055,#27273,#27274);
#22181=AXIS2_PLACEMENT_3D('',#64072,#27275,#27276);
#22182=AXIS2_PLACEMENT_3D('',#64074,#27278,#27279);
#22183=AXIS2_PLACEMENT_3D('',#64076,#27281,#27282);
#22184=AXIS2_PLACEMENT_3D('',#64085,#27285,#27286);
#22185=AXIS2_PLACEMENT_3D('',#64088,#27288,#27289);
#22186=AXIS2_PLACEMENT_3D('',#64089,#27290,#27291);
#22187=AXIS2_PLACEMENT_3D('',#64091,#27292,#27293);
#22188=AXIS2_PLACEMENT_3D('',#64106,#27294,#27295);
#22189=AXIS2_PLACEMENT_3D('',#64108,#27296,#27297);
#22190=AXIS2_PLACEMENT_3D('',#64111,#27299,#27300);
#22191=AXIS2_PLACEMENT_3D('',#64112,#27301,#27302);
#22192=AXIS2_PLACEMENT_3D('',#64113,#27303,#27304);
#22193=AXIS2_PLACEMENT_3D('',#64114,#27305,#27306);
#22194=AXIS2_PLACEMENT_3D('',#64116,#27307,#27308);
#22195=AXIS2_PLACEMENT_3D('',#64117,#27309,#27310);
#22196=AXIS2_PLACEMENT_3D('',#64118,#27311,#27312);
#22197=AXIS2_PLACEMENT_3D('',#64135,#27315,#27316);
#22198=AXIS2_PLACEMENT_3D('',#64144,#27319,#27320);
#22199=AXIS2_PLACEMENT_3D('',#64162,#27321,#27322);
#22200=AXIS2_PLACEMENT_3D('',#64163,#27323,#27324);
#22201=AXIS2_PLACEMENT_3D('',#64165,#27325,#27326);
#22202=AXIS2_PLACEMENT_3D('',#64166,#27327,#27328);
#22203=AXIS2_PLACEMENT_3D('',#64192,#27329,#27330);
#22204=AXIS2_PLACEMENT_3D('',#64197,#27331,#27332);
#22205=AXIS2_PLACEMENT_3D('',#64198,#27333,#27334);
#22206=AXIS2_PLACEMENT_3D('',#64202,#27336,#27337);
#22207=AXIS2_PLACEMENT_3D('',#64217,#27338,#27339);
#22208=AXIS2_PLACEMENT_3D('',#64218,#27340,#27341);
#22209=AXIS2_PLACEMENT_3D('',#64219,#27342,#27343);
#22210=AXIS2_PLACEMENT_3D('',#64220,#27344,#27345);
#22211=AXIS2_PLACEMENT_3D('',#64231,#27349,#27350);
#22212=AXIS2_PLACEMENT_3D('',#64234,#27352,#27353);
#22213=AXIS2_PLACEMENT_3D('',#64235,#27354,#27355);
#22214=AXIS2_PLACEMENT_3D('',#64238,#27357,#27358);
#22215=AXIS2_PLACEMENT_3D('',#64239,#27359,#27360);
#22216=AXIS2_PLACEMENT_3D('',#64242,#27362,#27363);
#22217=AXIS2_PLACEMENT_3D('',#64243,#27364,#27365);
#22218=AXIS2_PLACEMENT_3D('',#64245,#27366,#27367);
#22219=AXIS2_PLACEMENT_3D('',#64246,#27368,#27369);
#22220=AXIS2_PLACEMENT_3D('',#64247,#27370,#27371);
#22221=AXIS2_PLACEMENT_3D('',#64263,#27372,#27373);
#22222=AXIS2_PLACEMENT_3D('',#64264,#27374,#27375);
#22223=AXIS2_PLACEMENT_3D('',#64266,#27376,#27377);
#22224=AXIS2_PLACEMENT_3D('',#64270,#27379,#27380);
#22225=AXIS2_PLACEMENT_3D('',#64272,#27382,#27383);
#22226=AXIS2_PLACEMENT_3D('',#64288,#27384,#27385);
#22227=AXIS2_PLACEMENT_3D('',#64310,#27386,#27387);
#22228=AXIS2_PLACEMENT_3D('',#64312,#27388,#27389);
#22229=AXIS2_PLACEMENT_3D('',#64313,#27390,#27391);
#22230=AXIS2_PLACEMENT_3D('',#64314,#27392,#27393);
#22231=AXIS2_PLACEMENT_3D('',#64331,#27396,#27397);
#22232=AXIS2_PLACEMENT_3D('',#64345,#27398,#27399);
#22233=AXIS2_PLACEMENT_3D('',#64350,#27400,#27401);
#22234=AXIS2_PLACEMENT_3D('',#64351,#27402,#27403);
#22235=AXIS2_PLACEMENT_3D('',#64352,#27404,#27405);
#22236=AXIS2_PLACEMENT_3D('',#64367,#27407,#27408);
#22237=AXIS2_PLACEMENT_3D('',#64373,#27411,#27412);
#22238=AXIS2_PLACEMENT_3D('',#64378,#27415,#27416);
#22239=AXIS2_PLACEMENT_3D('',#64383,#27419,#27420);
#22240=AXIS2_PLACEMENT_3D('',#64385,#27422,#27423);
#22241=AXIS2_PLACEMENT_3D('',#64386,#27424,#27425);
#22242=AXIS2_PLACEMENT_3D('',#64390,#27427,#27428);
#22243=AXIS2_PLACEMENT_3D('',#64395,#27431,#27432);
#22244=AXIS2_PLACEMENT_3D('',#64398,#27434,#27435);
#22245=AXIS2_PLACEMENT_3D('',#64402,#27437,#27438);
#22246=AXIS2_PLACEMENT_3D('',#64406,#27441,#27442);
#22247=AXIS2_PLACEMENT_3D('',#64407,#27443,#27444);
#22248=AXIS2_PLACEMENT_3D('',#64422,#27446,#27447);
#22249=AXIS2_PLACEMENT_3D('',#64442,#27448,#27449);
#22250=AXIS2_PLACEMENT_3D('',#64447,#27450,#27451);
#22251=AXIS2_PLACEMENT_3D('',#64453,#27455,#27456);
#22252=AXIS2_PLACEMENT_3D('',#64468,#27458,#27459);
#22253=AXIS2_PLACEMENT_3D('',#64488,#27460,#27461);
#22254=AXIS2_PLACEMENT_3D('',#64493,#27462,#27463);
#22255=AXIS2_PLACEMENT_3D('',#64499,#27467,#27468);
#22256=AXIS2_PLACEMENT_3D('',#64512,#27469,#27470);
#22257=AXIS2_PLACEMENT_3D('',#64514,#27471,#27472);
#22258=AXIS2_PLACEMENT_3D('',#64516,#27473,#27474);
#22259=AXIS2_PLACEMENT_3D('',#64534,#27475,#27476);
#22260=AXIS2_PLACEMENT_3D('',#64536,#27477,#27478);
#22261=AXIS2_PLACEMENT_3D('',#64537,#27479,#27480);
#22262=AXIS2_PLACEMENT_3D('',#64538,#27481,#27482);
#22263=AXIS2_PLACEMENT_3D('',#64553,#27484,#27485);
#22264=AXIS2_PLACEMENT_3D('',#64558,#27486,#27487);
#22265=AXIS2_PLACEMENT_3D('',#64559,#27488,#27489);
#22266=AXIS2_PLACEMENT_3D('',#64560,#27490,#27491);
#22267=AXIS2_PLACEMENT_3D('',#64561,#27492,#27493);
#22268=AXIS2_PLACEMENT_3D('',#64562,#27494,#27495);
#22269=AXIS2_PLACEMENT_3D('',#64564,#27497,#27498);
#22270=AXIS2_PLACEMENT_3D('',#64568,#27500,#27501);
#22271=AXIS2_PLACEMENT_3D('',#64570,#27503,#27504);
#22272=AXIS2_PLACEMENT_3D('',#64592,#27505,#27506);
#22273=AXIS2_PLACEMENT_3D('',#64593,#27507,#27508);
#22274=AXIS2_PLACEMENT_3D('',#64595,#27510,#27511);
#22275=AXIS2_PLACEMENT_3D('',#64596,#27512,#27513);
#22276=AXIS2_PLACEMENT_3D('',#64597,#27514,#27515);
#22277=AXIS2_PLACEMENT_3D('',#64598,#27516,#27517);
#22278=AXIS2_PLACEMENT_3D('',#64599,#27518,#27519);
#22279=AXIS2_PLACEMENT_3D('',#64602,#27521,#27522);
#22280=AXIS2_PLACEMENT_3D('',#64603,#27523,#27524);
#22281=AXIS2_PLACEMENT_3D('',#64606,#27526,#27527);
#22282=AXIS2_PLACEMENT_3D('',#64607,#27528,#27529);
#22283=AXIS2_PLACEMENT_3D('',#64608,#27530,#27531);
#22284=AXIS2_PLACEMENT_3D('',#64609,#27532,#27533);
#22285=AXIS2_PLACEMENT_3D('',#64610,#27534,#27535);
#22286=AXIS2_PLACEMENT_3D('',#64611,#27536,#27537);
#22287=AXIS2_PLACEMENT_3D('',#64612,#27538,#27539);
#22288=AXIS2_PLACEMENT_3D('',#64613,#27540,#27541);
#22289=AXIS2_PLACEMENT_3D('',#64614,#27542,#27543);
#22290=AXIS2_PLACEMENT_3D('',#64615,#27544,#27545);
#22291=AXIS2_PLACEMENT_3D('',#64617,#27547,#27548);
#22292=AXIS2_PLACEMENT_3D('',#64618,#27549,#27550);
#22293=AXIS2_PLACEMENT_3D('',#64620,#27551,#27552);
#22294=AXIS2_PLACEMENT_3D('',#64622,#27553,#27554);
#22295=AXIS2_PLACEMENT_3D('',#64624,#27556,#27557);
#22296=AXIS2_PLACEMENT_3D('',#64638,#27559,#27560);
#22297=AXIS2_PLACEMENT_3D('',#64639,#27561,#27562);
#22298=AXIS2_PLACEMENT_3D('',#64654,#27564,#27565);
#22299=AXIS2_PLACEMENT_3D('',#64751,#27570,#27571);
#22300=AXIS2_PLACEMENT_3D('',#64758,#27572,#27573);
#22301=AXIS2_PLACEMENT_3D('',#64771,#27574,#27575);
#22302=AXIS2_PLACEMENT_3D('',#64775,#27578,#27579);
#22303=AXIS2_PLACEMENT_3D('',#64778,#27580,#27581);
#22304=AXIS2_PLACEMENT_3D('',#64779,#27582,#27583);
#22305=AXIS2_PLACEMENT_3D('',#64780,#27584,#27585);
#22306=AXIS2_PLACEMENT_3D('',#64781,#27586,#27587);
#22307=AXIS2_PLACEMENT_3D('',#64788,#27588,#27589);
#22308=AXIS2_PLACEMENT_3D('',#64791,#27591,#27592);
#22309=AXIS2_PLACEMENT_3D('',#64805,#27593,#27594);
#22310=AXIS2_PLACEMENT_3D('',#64816,#27595,#27596);
#22311=AXIS2_PLACEMENT_3D('',#64825,#27597,#27598);
#22312=AXIS2_PLACEMENT_3D('',#64827,#27600,#27601);
#22313=AXIS2_PLACEMENT_3D('',#64912,#27605,#27606);
#22314=AXIS2_PLACEMENT_3D('',#64914,#27608,#27609);
#22315=AXIS2_PLACEMENT_3D('',#64999,#27613,#27614);
#22316=AXIS2_PLACEMENT_3D('',#65001,#27616,#27617);
#22317=AXIS2_PLACEMENT_3D('',#65086,#27621,#27622);
#22318=AXIS2_PLACEMENT_3D('',#65098,#27624,#27625);
#22319=AXIS2_PLACEMENT_3D('',#65101,#27627,#27628);
#22320=AXIS2_PLACEMENT_3D('',#65102,#27629,#27630);
#22321=AXIS2_PLACEMENT_3D('',#65104,#27631,#27632);
#22322=AXIS2_PLACEMENT_3D('',#65105,#27633,#27634);
#22323=AXIS2_PLACEMENT_3D('',#65106,#27635,#27636);
#22324=AXIS2_PLACEMENT_3D('',#65107,#27637,#27638);
#22325=AXIS2_PLACEMENT_3D('',#65108,#27639,#27640);
#22326=AXIS2_PLACEMENT_3D('',#65109,#27641,#27642);
#22327=AXIS2_PLACEMENT_3D('',#65112,#27645,#27646);
#22328=AXIS2_PLACEMENT_3D('',#65113,#27647,#27648);
#22329=AXIS2_PLACEMENT_3D('',#65114,#27649,#27650);
#22330=AXIS2_PLACEMENT_3D('',#65209,#27651,#27652);
#22331=AXIS2_PLACEMENT_3D('',#65211,#27654,#27655);
#22332=AXIS2_PLACEMENT_3D('',#65219,#27656,#27657);
#22333=AXIS2_PLACEMENT_3D('',#65220,#27658,#27659);
#22334=AXIS2_PLACEMENT_3D('',#65223,#27661,#27662);
#22335=AXIS2_PLACEMENT_3D('',#65224,#27663,#27664);
#22336=AXIS2_PLACEMENT_3D('',#65226,#27665,#27666);
#22337=AXIS2_PLACEMENT_3D('',#65269,#27667,#27668);
#22338=AXIS2_PLACEMENT_3D('',#65270,#27669,#27670);
#22339=AXIS2_PLACEMENT_3D('',#65271,#27671,#27672);
#22340=AXIS2_PLACEMENT_3D('',#65272,#27673,#27674);
#22341=AXIS2_PLACEMENT_3D('',#65273,#27675,#27676);
#22342=AXIS2_PLACEMENT_3D('',#65274,#27677,#27678);
#22343=AXIS2_PLACEMENT_3D('',#65275,#27679,#27680);
#22344=AXIS2_PLACEMENT_3D('',#65370,#27681,#27682);
#22345=AXIS2_PLACEMENT_3D('',#65372,#27684,#27685);
#22346=AXIS2_PLACEMENT_3D('',#65377,#27687,#27688);
#22347=AXIS2_PLACEMENT_3D('',#65380,#27690,#27691);
#22348=AXIS2_PLACEMENT_3D('',#65381,#27692,#27693);
#22349=AXIS2_PLACEMENT_3D('',#65394,#27694,#27695);
#22350=AXIS2_PLACEMENT_3D('',#65395,#27696,#27697);
#22351=AXIS2_PLACEMENT_3D('',#65396,#27698,#27699);
#22352=AXIS2_PLACEMENT_3D('',#65405,#27700,#27701);
#22353=AXIS2_PLACEMENT_3D('',#65408,#27703,#27704);
#22354=AXIS2_PLACEMENT_3D('',#65409,#27705,#27706);
#22355=AXIS2_PLACEMENT_3D('',#65410,#27707,#27708);
#22356=AXIS2_PLACEMENT_3D('',#65411,#27709,#27710);
#22357=AXIS2_PLACEMENT_3D('',#65414,#27713,#27714);
#22358=AXIS2_PLACEMENT_3D('',#65416,#27716,#27717);
#22359=AXIS2_PLACEMENT_3D('',#65428,#27721,#27722);
#22360=AXIS2_PLACEMENT_3D('',#65431,#27724,#27725);
#22361=AXIS2_PLACEMENT_3D('',#65432,#27726,#27727);
#22362=AXIS2_PLACEMENT_3D('',#65455,#27728,#27729);
#22363=AXIS2_PLACEMENT_3D('',#65457,#27731,#27732);
#22364=AXIS2_PLACEMENT_3D('',#65459,#27733,#27734);
#22365=AXIS2_PLACEMENT_3D('',#65462,#27736,#27737);
#22366=AXIS2_PLACEMENT_3D('',#65473,#27741,#27742);
#22367=AXIS2_PLACEMENT_3D('',#65475,#27744,#27745);
#22368=AXIS2_PLACEMENT_3D('',#65477,#27747,#27748);
#22369=AXIS2_PLACEMENT_3D('',#65479,#27750,#27751);
#22370=AXIS2_PLACEMENT_3D('',#65480,#27752,#27753);
#22371=AXIS2_PLACEMENT_3D('',#65493,#27754,#27755);
#22372=AXIS2_PLACEMENT_3D('',#65506,#27756,#27757);
#22373=AXIS2_PLACEMENT_3D('',#65507,#27758,#27759);
#22374=AXIS2_PLACEMENT_3D('',#65508,#27760,#27761);
#22375=AXIS2_PLACEMENT_3D('',#65509,#27762,#27763);
#22376=AXIS2_PLACEMENT_3D('',#65510,#27764,#27765);
#22377=AXIS2_PLACEMENT_3D('',#65512,#27767,#27768);
#22378=AXIS2_PLACEMENT_3D('',#65513,#27769,#27770);
#22379=AXIS2_PLACEMENT_3D('',#65514,#27771,#27772);
#22380=AXIS2_PLACEMENT_3D('',#65515,#27773,#27774);
#22381=AXIS2_PLACEMENT_3D('',#65516,#27775,#27776);
#22382=AXIS2_PLACEMENT_3D('',#65517,#27777,#27778);
#22383=AXIS2_PLACEMENT_3D('',#65518,#27779,#27780);
#22384=AXIS2_PLACEMENT_3D('',#65519,#27781,#27782);
#22385=AXIS2_PLACEMENT_3D('',#65520,#27783,#27784);
#22386=AXIS2_PLACEMENT_3D('',#65521,#27785,#27786);
#22387=AXIS2_PLACEMENT_3D('',#65522,#27787,#27788);
#22388=AXIS2_PLACEMENT_3D('',#65523,#27789,#27790);
#22389=AXIS2_PLACEMENT_3D('',#65524,#27791,#27792);
#22390=AXIS2_PLACEMENT_3D('',#65525,#27793,#27794);
#22391=AXIS2_PLACEMENT_3D('',#65526,#27795,#27796);
#22392=AXIS2_PLACEMENT_3D('',#65527,#27797,#27798);
#22393=AXIS2_PLACEMENT_3D('',#65528,#27799,#27800);
#22394=AXIS2_PLACEMENT_3D('',#65529,#27801,#27802);
#22395=AXIS2_PLACEMENT_3D('',#65530,#27803,#27804);
#22396=AXIS2_PLACEMENT_3D('',#65531,#27805,#27806);
#22397=AXIS2_PLACEMENT_3D('',#65532,#27807,#27808);
#22398=AXIS2_PLACEMENT_3D('',#65533,#27809,#27810);
#22399=AXIS2_PLACEMENT_3D('',#65534,#27811,#27812);
#22400=AXIS2_PLACEMENT_3D('',#65535,#27813,#27814);
#22401=AXIS2_PLACEMENT_3D('',#65536,#27815,#27816);
#22402=AXIS2_PLACEMENT_3D('',#65537,#27817,#27818);
#22403=DIRECTION('axis',(0.,0.,1.));
#22404=DIRECTION('refdir',(1.,0.,0.));
#22405=DIRECTION('axis',(0.,0.,1.));
#22406=DIRECTION('refdir',(1.,0.,0.));
#22407=DIRECTION('center_axis',(1.,0.,0.));
#22408=DIRECTION('ref_axis',(0.,1.,0.));
#22409=DIRECTION('',(-1.,0.,0.));
#22410=DIRECTION('center_axis',(-1.,0.,0.));
#22411=DIRECTION('ref_axis',(0.,1.,0.));
#22412=DIRECTION('',(-1.,0.,0.));
#22413=DIRECTION('center_axis',(1.,0.,0.));
#22414=DIRECTION('ref_axis',(0.,1.,0.));
#22415=DIRECTION('',(-1.,0.,0.));
#22416=DIRECTION('center_axis',(-1.,0.,0.));
#22417=DIRECTION('ref_axis',(0.,1.,0.));
#22418=DIRECTION('',(-1.,0.,0.));
#22419=DIRECTION('center_axis',(-1.,0.,0.));
#22420=DIRECTION('ref_axis',(0.,1.,0.));
#22421=DIRECTION('center_axis',(-1.,0.,0.));
#22422=DIRECTION('ref_axis',(0.,1.,0.));
#22423=DIRECTION('',(1.,0.,0.));
#22424=DIRECTION('center_axis',(1.,0.,0.));
#22425=DIRECTION('ref_axis',(0.,1.,0.));
#22426=DIRECTION('center_axis',(-1.,0.,0.));
#22427=DIRECTION('ref_axis',(0.,1.,0.));
#22428=DIRECTION('',(1.,0.,0.));
#22429=DIRECTION('center_axis',(1.,0.,0.));
#22430=DIRECTION('ref_axis',(0.,1.,0.));
#22431=DIRECTION('',(-1.,0.,0.));
#22432=DIRECTION('center_axis',(-1.,0.,0.));
#22433=DIRECTION('ref_axis',(0.,1.,0.));
#22434=DIRECTION('center_axis',(1.,0.,0.));
#22435=DIRECTION('ref_axis',(0.,1.,0.));
#22436=DIRECTION('',(-1.,0.,0.));
#22437=DIRECTION('center_axis',(1.,0.,0.));
#22438=DIRECTION('ref_axis',(0.,1.,0.));
#22439=DIRECTION('',(-1.,0.,0.));
#22440=DIRECTION('center_axis',(1.,0.,0.));
#22441=DIRECTION('ref_axis',(0.,1.,0.));
#22442=DIRECTION('',(-1.,0.,0.));
#22443=DIRECTION('center_axis',(1.,0.,0.));
#22444=DIRECTION('ref_axis',(0.,1.,0.));
#22445=DIRECTION('',(-1.,0.,0.));
#22446=DIRECTION('center_axis',(1.,0.,0.));
#22447=DIRECTION('ref_axis',(0.,1.,0.));
#22448=DIRECTION('',(-1.,0.,0.));
#22449=DIRECTION('center_axis',(1.,0.,0.));
#22450=DIRECTION('ref_axis',(0.,1.,0.));
#22451=DIRECTION('',(-1.,0.,0.));
#22452=DIRECTION('center_axis',(1.,0.,0.));
#22453=DIRECTION('ref_axis',(0.,1.,0.));
#22454=DIRECTION('',(-1.,0.,0.));
#22455=DIRECTION('center_axis',(1.,0.,0.));
#22456=DIRECTION('ref_axis',(0.,1.,0.));
#22457=DIRECTION('',(-1.,0.,0.));
#22458=DIRECTION('center_axis',(1.,0.,0.));
#22459=DIRECTION('ref_axis',(0.,1.,0.));
#22460=DIRECTION('',(-1.,0.,0.));
#22461=DIRECTION('center_axis',(1.,0.,0.));
#22462=DIRECTION('ref_axis',(0.,1.,0.));
#22463=DIRECTION('',(-1.,0.,0.));
#22464=DIRECTION('center_axis',(1.,0.,0.));
#22465=DIRECTION('ref_axis',(0.,1.,0.));
#22466=DIRECTION('',(-1.,0.,0.));
#22467=DIRECTION('center_axis',(1.,0.,0.));
#22468=DIRECTION('ref_axis',(0.,1.,0.));
#22469=DIRECTION('',(-1.,0.,0.));
#22470=DIRECTION('center_axis',(1.,0.,0.));
#22471=DIRECTION('ref_axis',(0.,1.,0.));
#22472=DIRECTION('',(-1.,0.,0.));
#22473=DIRECTION('center_axis',(1.,0.,0.));
#22474=DIRECTION('ref_axis',(0.,1.,0.));
#22475=DIRECTION('',(-1.,0.,0.));
#22476=DIRECTION('center_axis',(1.,0.,0.));
#22477=DIRECTION('ref_axis',(0.,1.,0.));
#22478=DIRECTION('',(-1.,0.,0.));
#22479=DIRECTION('center_axis',(1.,0.,0.));
#22480=DIRECTION('ref_axis',(0.,1.,0.));
#22481=DIRECTION('',(-1.,0.,0.));
#22482=DIRECTION('center_axis',(1.,0.,0.));
#22483=DIRECTION('ref_axis',(0.,1.,0.));
#22484=DIRECTION('',(-1.,0.,0.));
#22485=DIRECTION('center_axis',(1.,0.,0.));
#22486=DIRECTION('ref_axis',(0.,1.,0.));
#22487=DIRECTION('',(-1.,0.,0.));
#22488=DIRECTION('center_axis',(1.,0.,0.));
#22489=DIRECTION('ref_axis',(0.,1.,0.));
#22490=DIRECTION('',(-1.,0.,0.));
#22491=DIRECTION('center_axis',(1.,0.,0.));
#22492=DIRECTION('ref_axis',(0.,1.,0.));
#22493=DIRECTION('',(-1.,0.,0.));
#22494=DIRECTION('center_axis',(1.,0.,0.));
#22495=DIRECTION('ref_axis',(0.,1.,0.));
#22496=DIRECTION('',(-1.,0.,0.));
#22497=DIRECTION('center_axis',(1.,0.,0.));
#22498=DIRECTION('ref_axis',(0.,1.,0.));
#22499=DIRECTION('',(-1.,0.,0.));
#22500=DIRECTION('center_axis',(1.,0.,0.));
#22501=DIRECTION('ref_axis',(0.,1.,0.));
#22502=DIRECTION('',(-1.,0.,0.));
#22503=DIRECTION('center_axis',(1.,0.,0.));
#22504=DIRECTION('ref_axis',(0.,1.,0.));
#22505=DIRECTION('',(-1.,0.,0.));
#22506=DIRECTION('center_axis',(1.,0.,0.));
#22507=DIRECTION('ref_axis',(0.,1.,0.));
#22508=DIRECTION('',(-1.,0.,0.));
#22509=DIRECTION('center_axis',(1.,0.,0.));
#22510=DIRECTION('ref_axis',(0.,1.,0.));
#22511=DIRECTION('',(-1.,0.,0.));
#22512=DIRECTION('center_axis',(1.,0.,0.));
#22513=DIRECTION('ref_axis',(0.,1.,0.));
#22514=DIRECTION('',(-1.,0.,0.));
#22515=DIRECTION('center_axis',(1.,0.,0.));
#22516=DIRECTION('ref_axis',(0.,1.,0.));
#22517=DIRECTION('',(-1.,0.,0.));
#22518=DIRECTION('center_axis',(1.,0.,0.));
#22519=DIRECTION('ref_axis',(0.,1.,0.));
#22520=DIRECTION('',(-1.,0.,0.));
#22521=DIRECTION('center_axis',(1.,0.,0.));
#22522=DIRECTION('ref_axis',(0.,1.,0.));
#22523=DIRECTION('',(-1.,0.,0.));
#22524=DIRECTION('center_axis',(1.,0.,0.));
#22525=DIRECTION('ref_axis',(0.,1.,0.));
#22526=DIRECTION('',(-1.,0.,0.));
#22527=DIRECTION('center_axis',(1.,0.,0.));
#22528=DIRECTION('ref_axis',(0.,1.,0.));
#22529=DIRECTION('',(-1.,0.,0.));
#22530=DIRECTION('center_axis',(1.,0.,0.));
#22531=DIRECTION('ref_axis',(0.,1.,0.));
#22532=DIRECTION('',(-1.,0.,0.));
#22533=DIRECTION('center_axis',(1.,0.,0.));
#22534=DIRECTION('ref_axis',(0.,1.,0.));
#22535=DIRECTION('',(-1.,0.,0.));
#22536=DIRECTION('center_axis',(1.,0.,0.));
#22537=DIRECTION('ref_axis',(0.,1.,0.));
#22538=DIRECTION('',(-1.,0.,0.));
#22539=DIRECTION('center_axis',(1.,0.,0.));
#22540=DIRECTION('ref_axis',(0.,1.,0.));
#22541=DIRECTION('',(-1.,0.,0.));
#22542=DIRECTION('center_axis',(1.,0.,0.));
#22543=DIRECTION('ref_axis',(0.,1.,0.));
#22544=DIRECTION('',(-1.,0.,0.));
#22545=DIRECTION('center_axis',(1.,0.,0.));
#22546=DIRECTION('ref_axis',(0.,1.,0.));
#22547=DIRECTION('',(-1.,0.,0.));
#22548=DIRECTION('center_axis',(1.,0.,0.));
#22549=DIRECTION('ref_axis',(0.,1.,0.));
#22550=DIRECTION('',(-1.,0.,0.));
#22551=DIRECTION('center_axis',(1.,0.,0.));
#22552=DIRECTION('ref_axis',(0.,1.,0.));
#22553=DIRECTION('',(-1.,0.,0.));
#22554=DIRECTION('center_axis',(1.,0.,0.));
#22555=DIRECTION('ref_axis',(0.,1.,0.));
#22556=DIRECTION('',(-1.,0.,0.));
#22557=DIRECTION('center_axis',(1.,0.,0.));
#22558=DIRECTION('ref_axis',(0.,1.,0.));
#22559=DIRECTION('',(-1.,0.,0.));
#22560=DIRECTION('center_axis',(1.,0.,0.));
#22561=DIRECTION('ref_axis',(0.,1.,0.));
#22562=DIRECTION('',(-1.,0.,0.));
#22563=DIRECTION('center_axis',(1.,0.,0.));
#22564=DIRECTION('ref_axis',(0.,1.,0.));
#22565=DIRECTION('',(-1.,0.,0.));
#22566=DIRECTION('center_axis',(1.,0.,0.));
#22567=DIRECTION('ref_axis',(0.,1.,0.));
#22568=DIRECTION('',(-1.,0.,0.));
#22569=DIRECTION('center_axis',(1.,0.,0.));
#22570=DIRECTION('ref_axis',(0.,1.,0.));
#22571=DIRECTION('',(-1.,0.,0.));
#22572=DIRECTION('center_axis',(1.,0.,0.));
#22573=DIRECTION('ref_axis',(0.,1.,0.));
#22574=DIRECTION('',(-1.,0.,0.));
#22575=DIRECTION('center_axis',(1.,0.,0.));
#22576=DIRECTION('ref_axis',(0.,1.,0.));
#22577=DIRECTION('',(-1.,0.,0.));
#22578=DIRECTION('center_axis',(1.,0.,0.));
#22579=DIRECTION('ref_axis',(0.,1.,0.));
#22580=DIRECTION('',(-1.,0.,0.));
#22581=DIRECTION('center_axis',(1.,0.,0.));
#22582=DIRECTION('ref_axis',(0.,1.,0.));
#22583=DIRECTION('',(-1.,0.,0.));
#22584=DIRECTION('center_axis',(1.,0.,0.));
#22585=DIRECTION('ref_axis',(0.,1.,0.));
#22586=DIRECTION('',(-1.,0.,0.));
#22587=DIRECTION('center_axis',(1.,0.,0.));
#22588=DIRECTION('ref_axis',(0.,1.,0.));
#22589=DIRECTION('',(-1.,0.,0.));
#22590=DIRECTION('center_axis',(1.,0.,0.));
#22591=DIRECTION('ref_axis',(0.,1.,0.));
#22592=DIRECTION('',(-1.,0.,0.));
#22593=DIRECTION('center_axis',(1.,0.,0.));
#22594=DIRECTION('ref_axis',(0.,1.,0.));
#22595=DIRECTION('',(-1.,0.,0.));
#22596=DIRECTION('center_axis',(1.,0.,0.));
#22597=DIRECTION('ref_axis',(0.,1.,0.));
#22598=DIRECTION('',(-1.,0.,0.));
#22599=DIRECTION('center_axis',(1.,0.,0.));
#22600=DIRECTION('ref_axis',(0.,1.,0.));
#22601=DIRECTION('',(-1.,0.,0.));
#22602=DIRECTION('center_axis',(1.,0.,0.));
#22603=DIRECTION('ref_axis',(0.,1.,0.));
#22604=DIRECTION('',(-1.,0.,0.));
#22605=DIRECTION('center_axis',(1.,0.,0.));
#22606=DIRECTION('ref_axis',(0.,1.,0.));
#22607=DIRECTION('',(-1.,0.,0.));
#22608=DIRECTION('center_axis',(1.,0.,0.));
#22609=DIRECTION('ref_axis',(0.,1.,0.));
#22610=DIRECTION('',(-1.,0.,0.));
#22611=DIRECTION('center_axis',(1.,0.,0.));
#22612=DIRECTION('ref_axis',(0.,1.,0.));
#22613=DIRECTION('',(-1.,0.,0.));
#22614=DIRECTION('center_axis',(1.,0.,0.));
#22615=DIRECTION('ref_axis',(0.,1.,0.));
#22616=DIRECTION('',(-1.,0.,0.));
#22617=DIRECTION('center_axis',(1.,0.,0.));
#22618=DIRECTION('ref_axis',(0.,1.,0.));
#22619=DIRECTION('',(-1.,0.,0.));
#22620=DIRECTION('center_axis',(-1.,0.,0.));
#22621=DIRECTION('ref_axis',(0.,1.,0.));
#22622=DIRECTION('',(-1.,0.,0.));
#22623=DIRECTION('center_axis',(1.,0.,0.));
#22624=DIRECTION('ref_axis',(0.,1.,0.));
#22625=DIRECTION('center_axis',(-1.,0.,0.));
#22626=DIRECTION('ref_axis',(0.,1.,0.));
#22627=DIRECTION('center_axis',(1.,0.,0.));
#22628=DIRECTION('ref_axis',(0.,1.,0.));
#22629=DIRECTION('',(-1.,0.,0.));
#22630=DIRECTION('center_axis',(1.,0.,0.));
#22631=DIRECTION('ref_axis',(0.,1.,0.));
#22632=DIRECTION('',(-1.,0.,0.));
#22633=DIRECTION('center_axis',(1.,0.,0.));
#22634=DIRECTION('ref_axis',(0.,1.,0.));
#22635=DIRECTION('',(-1.,0.,0.));
#22636=DIRECTION('center_axis',(1.,0.,0.));
#22637=DIRECTION('ref_axis',(0.,1.,0.));
#22638=DIRECTION('',(-1.,0.,0.));
#22639=DIRECTION('center_axis',(1.,0.,0.));
#22640=DIRECTION('ref_axis',(0.,1.,0.));
#22641=DIRECTION('',(-1.,0.,0.));
#22642=DIRECTION('center_axis',(1.,0.,0.));
#22643=DIRECTION('ref_axis',(0.,1.,0.));
#22644=DIRECTION('',(-1.,0.,0.));
#22645=DIRECTION('center_axis',(1.,0.,0.));
#22646=DIRECTION('ref_axis',(0.,1.,0.));
#22647=DIRECTION('',(-1.,0.,0.));
#22648=DIRECTION('center_axis',(1.,0.,0.));
#22649=DIRECTION('ref_axis',(0.,1.,0.));
#22650=DIRECTION('',(-1.,0.,0.));
#22651=DIRECTION('center_axis',(1.,0.,0.));
#22652=DIRECTION('ref_axis',(0.,1.,0.));
#22653=DIRECTION('',(-1.,0.,0.));
#22654=DIRECTION('center_axis',(1.,0.,0.));
#22655=DIRECTION('ref_axis',(0.,1.,0.));
#22656=DIRECTION('',(-1.,0.,0.));
#22657=DIRECTION('center_axis',(1.,0.,0.));
#22658=DIRECTION('ref_axis',(0.,1.,0.));
#22659=DIRECTION('',(-1.,0.,0.));
#22660=DIRECTION('center_axis',(1.,0.,0.));
#22661=DIRECTION('ref_axis',(0.,1.,0.));
#22662=DIRECTION('',(-1.,0.,0.));
#22663=DIRECTION('center_axis',(1.,0.,0.));
#22664=DIRECTION('ref_axis',(0.,1.,0.));
#22665=DIRECTION('',(-1.,0.,0.));
#22666=DIRECTION('center_axis',(1.,0.,0.));
#22667=DIRECTION('ref_axis',(0.,1.,0.));
#22668=DIRECTION('',(-1.,0.,0.));
#22669=DIRECTION('center_axis',(1.,0.,0.));
#22670=DIRECTION('ref_axis',(0.,1.,0.));
#22671=DIRECTION('',(-1.,0.,0.));
#22672=DIRECTION('center_axis',(1.,0.,0.));
#22673=DIRECTION('ref_axis',(0.,-0.328007595378459,-0.944675085610942));
#22674=DIRECTION('',(1.,0.,0.));
#22675=DIRECTION('center_axis',(1.,0.,0.));
#22676=DIRECTION('ref_axis',(0.,1.,9.92840284004976E-14));
#22677=DIRECTION('center_axis',(1.,0.,0.));
#22678=DIRECTION('ref_axis',(0.,1.,9.92840284004976E-14));
#22679=DIRECTION('',(1.,0.,0.));
#22680=DIRECTION('center_axis',(1.,0.,0.));
#22681=DIRECTION('ref_axis',(0.,1.,9.92840284004976E-14));
#22682=DIRECTION('',(1.,0.,0.));
#22683=DIRECTION('center_axis',(1.,0.,0.));
#22684=DIRECTION('ref_axis',(0.,1.,9.92840284004976E-14));
#22685=DIRECTION('',(1.,0.,0.));
#22686=DIRECTION('center_axis',(1.,0.,0.));
#22687=DIRECTION('ref_axis',(0.,1.,9.92840284004976E-14));
#22688=DIRECTION('',(1.,0.,0.));
#22689=DIRECTION('center_axis',(1.,0.,0.));
#22690=DIRECTION('ref_axis',(0.,1.,9.92840284004976E-14));
#22691=DIRECTION('',(1.,0.,0.));
#22692=DIRECTION('center_axis',(1.,0.,0.));
#22693=DIRECTION('ref_axis',(0.,1.,9.92840284004976E-14));
#22694=DIRECTION('',(1.,0.,0.));
#22695=DIRECTION('center_axis',(1.,0.,0.));
#22696=DIRECTION('ref_axis',(0.,1.,9.92840284004976E-14));
#22697=DIRECTION('',(1.,0.,0.));
#22698=DIRECTION('center_axis',(1.,0.,0.));
#22699=DIRECTION('ref_axis',(0.,1.,9.92840284004976E-14));
#22700=DIRECTION('',(1.,0.,0.));
#22701=DIRECTION('center_axis',(1.,0.,0.));
#22702=DIRECTION('ref_axis',(0.,1.,9.92840284004976E-14));
#22703=DIRECTION('',(1.,0.,0.));
#22704=DIRECTION('center_axis',(1.,0.,0.));
#22705=DIRECTION('ref_axis',(0.,1.,9.92840284004976E-14));
#22706=DIRECTION('',(1.,0.,0.));
#22707=DIRECTION('center_axis',(1.,0.,0.));
#22708=DIRECTION('ref_axis',(0.,1.,9.92840284004976E-14));
#22709=DIRECTION('',(1.,0.,0.));
#22710=DIRECTION('center_axis',(1.,0.,0.));
#22711=DIRECTION('ref_axis',(0.,1.,9.92840284004976E-14));
#22712=DIRECTION('',(1.,0.,0.));
#22713=DIRECTION('center_axis',(1.,0.,0.));
#22714=DIRECTION('ref_axis',(0.,1.,9.92840284004976E-14));
#22715=DIRECTION('',(1.,0.,0.));
#22716=DIRECTION('center_axis',(1.,0.,0.));
#22717=DIRECTION('ref_axis',(0.,1.,9.92840284004976E-14));
#22718=DIRECTION('',(1.,0.,0.));
#22719=DIRECTION('center_axis',(1.,0.,0.));
#22720=DIRECTION('ref_axis',(0.,1.,9.92840284004976E-14));
#22721=DIRECTION('',(1.,0.,0.));
#22722=DIRECTION('center_axis',(1.,0.,0.));
#22723=DIRECTION('ref_axis',(0.,1.,-9.14588507257614E-13));
#22724=DIRECTION('',(1.,0.,0.));
#22725=DIRECTION('center_axis',(1.,0.,0.));
#22726=DIRECTION('ref_axis',(0.,1.,-9.14588507257614E-13));
#22727=DIRECTION('center_axis',(1.,0.,0.));
#22728=DIRECTION('ref_axis',(0.,1.,-9.14588507257614E-13));
#22729=DIRECTION('',(1.,0.,0.));
#22730=DIRECTION('center_axis',(1.,0.,0.));
#22731=DIRECTION('ref_axis',(0.,1.,-9.14588507257614E-13));
#22732=DIRECTION('center_axis',(1.,0.,0.));
#22733=DIRECTION('ref_axis',(0.,1.,-9.14588507257614E-13));
#22734=DIRECTION('',(1.,0.,0.));
#22735=DIRECTION('center_axis',(1.,0.,0.));
#22736=DIRECTION('ref_axis',(0.,1.,-9.14588507257614E-13));
#22737=DIRECTION('',(1.,0.,0.));
#22738=DIRECTION('center_axis',(1.,0.,0.));
#22739=DIRECTION('ref_axis',(0.,1.,-9.14588507257614E-13));
#22740=DIRECTION('',(1.,0.,0.));
#22741=DIRECTION('center_axis',(1.,0.,0.));
#22742=DIRECTION('ref_axis',(0.,1.,-9.14588507257614E-13));
#22743=DIRECTION('',(1.,0.,0.));
#22744=DIRECTION('center_axis',(1.,0.,0.));
#22745=DIRECTION('ref_axis',(0.,1.,-9.14588507257614E-13));
#22746=DIRECTION('',(1.,0.,0.));
#22747=DIRECTION('center_axis',(1.,0.,0.));
#22748=DIRECTION('ref_axis',(0.,1.,-9.14588507257614E-13));
#22749=DIRECTION('',(1.,0.,0.));
#22750=DIRECTION('center_axis',(1.,0.,0.));
#22751=DIRECTION('ref_axis',(0.,1.,-9.14588507257614E-13));
#22752=DIRECTION('',(1.,0.,0.));
#22753=DIRECTION('center_axis',(1.,0.,0.));
#22754=DIRECTION('ref_axis',(0.,1.,-9.14588507257614E-13));
#22755=DIRECTION('',(1.,0.,0.));
#22756=DIRECTION('center_axis',(1.,0.,0.));
#22757=DIRECTION('ref_axis',(0.,1.,-9.14588507257614E-13));
#22758=DIRECTION('',(1.,0.,0.));
#22759=DIRECTION('center_axis',(1.,0.,0.));
#22760=DIRECTION('ref_axis',(0.,1.,-9.14588507257614E-13));
#22761=DIRECTION('',(1.,0.,0.));
#22762=DIRECTION('center_axis',(1.,0.,0.));
#22763=DIRECTION('ref_axis',(0.,1.,-9.14588507257614E-13));
#22764=DIRECTION('',(1.,0.,0.));
#22765=DIRECTION('center_axis',(1.,0.,0.));
#22766=DIRECTION('ref_axis',(0.,1.,-9.14588507257614E-13));
#22767=DIRECTION('',(1.,0.,0.));
#22768=DIRECTION('center_axis',(1.,0.,0.));
#22769=DIRECTION('ref_axis',(0.,1.,-9.14588507257614E-13));
#22770=DIRECTION('',(1.,0.,0.));
#22771=DIRECTION('center_axis',(1.,0.,0.));
#22772=DIRECTION('ref_axis',(0.,1.,-9.14588507257614E-13));
#22773=DIRECTION('',(1.,0.,0.));
#22774=DIRECTION('center_axis',(1.,0.,0.));
#22775=DIRECTION('ref_axis',(0.,1.,-9.14588507257614E-13));
#22776=DIRECTION('',(1.,0.,0.));
#22777=DIRECTION('center_axis',(1.,0.,0.));
#22778=DIRECTION('ref_axis',(0.,1.,-9.14588507257614E-13));
#22779=DIRECTION('',(1.,0.,0.));
#22780=DIRECTION('center_axis',(1.,0.,0.));
#22781=DIRECTION('ref_axis',(0.,1.,-9.14588507257614E-13));
#22782=DIRECTION('',(1.,0.,0.));
#22783=DIRECTION('center_axis',(1.,0.,0.));
#22784=DIRECTION('ref_axis',(0.,1.,-9.14588507257614E-13));
#22785=DIRECTION('',(1.,0.,0.));
#22786=DIRECTION('center_axis',(1.,0.,0.));
#22787=DIRECTION('ref_axis',(0.,1.,-9.14588507257614E-13));
#22788=DIRECTION('',(1.,0.,0.));
#22789=DIRECTION('center_axis',(1.,0.,0.));
#22790=DIRECTION('ref_axis',(0.,1.,-9.14588507257614E-13));
#22791=DIRECTION('',(1.,0.,0.));
#22792=DIRECTION('center_axis',(1.,0.,0.));
#22793=DIRECTION('ref_axis',(0.,1.,-9.14588507257614E-13));
#22794=DIRECTION('',(1.,0.,0.));
#22795=DIRECTION('center_axis',(1.,0.,0.));
#22796=DIRECTION('ref_axis',(0.,1.,-9.14588507257614E-13));
#22797=DIRECTION('',(1.,0.,0.));
#22798=DIRECTION('center_axis',(1.,0.,0.));
#22799=DIRECTION('ref_axis',(0.,1.,-9.14588507257614E-13));
#22800=DIRECTION('',(1.,0.,0.));
#22801=DIRECTION('center_axis',(1.,0.,0.));
#22802=DIRECTION('ref_axis',(0.,1.,-9.14588507257614E-13));
#22803=DIRECTION('',(1.,0.,0.));
#22804=DIRECTION('center_axis',(1.,0.,0.));
#22805=DIRECTION('ref_axis',(0.,1.,-9.14588507257614E-13));
#22806=DIRECTION('',(1.,0.,0.));
#22807=DIRECTION('center_axis',(1.,0.,0.));
#22808=DIRECTION('ref_axis',(0.,1.,-9.14588507257614E-13));
#22809=DIRECTION('',(1.,0.,0.));
#22810=DIRECTION('center_axis',(1.,0.,0.));
#22811=DIRECTION('ref_axis',(0.,1.,-9.14588507257614E-13));
#22812=DIRECTION('',(1.,0.,0.));
#22813=DIRECTION('center_axis',(1.,0.,0.));
#22814=DIRECTION('ref_axis',(0.,1.,-9.14588507257614E-13));
#22815=DIRECTION('',(1.,0.,0.));
#22816=DIRECTION('center_axis',(1.,0.,0.));
#22817=DIRECTION('ref_axis',(0.,1.,-9.14588507257614E-13));
#22818=DIRECTION('',(1.,0.,0.));
#22819=DIRECTION('center_axis',(1.,0.,0.));
#22820=DIRECTION('ref_axis',(0.,1.,-9.14588507257614E-13));
#22821=DIRECTION('',(1.,0.,0.));
#22822=DIRECTION('center_axis',(1.,0.,0.));
#22823=DIRECTION('ref_axis',(0.,1.,-9.14588507257614E-13));
#22824=DIRECTION('',(1.,0.,0.));
#22825=DIRECTION('center_axis',(1.,0.,0.));
#22826=DIRECTION('ref_axis',(0.,1.,-9.14588507257614E-13));
#22827=DIRECTION('',(1.,0.,0.));
#22828=DIRECTION('center_axis',(1.,0.,0.));
#22829=DIRECTION('ref_axis',(0.,1.,-9.14588507257614E-13));
#22830=DIRECTION('',(1.,0.,0.));
#22831=DIRECTION('center_axis',(1.,0.,0.));
#22832=DIRECTION('ref_axis',(0.,1.,-9.14588507257614E-13));
#22833=DIRECTION('',(1.,0.,0.));
#22834=DIRECTION('center_axis',(1.,0.,0.));
#22835=DIRECTION('ref_axis',(0.,1.,-9.14588507257614E-13));
#22836=DIRECTION('',(1.,0.,0.));
#22837=DIRECTION('center_axis',(1.,0.,0.));
#22838=DIRECTION('ref_axis',(0.,1.,-9.14588507257614E-13));
#22839=DIRECTION('',(1.,0.,0.));
#22840=DIRECTION('center_axis',(1.,0.,0.));
#22841=DIRECTION('ref_axis',(0.,1.,-9.14588507257614E-13));
#22842=DIRECTION('',(1.,0.,0.));
#22843=DIRECTION('center_axis',(1.,0.,0.));
#22844=DIRECTION('ref_axis',(0.,1.,-9.14588507257614E-13));
#22845=DIRECTION('',(1.,0.,0.));
#22846=DIRECTION('center_axis',(1.,0.,0.));
#22847=DIRECTION('ref_axis',(0.,1.,-9.14588507257614E-13));
#22848=DIRECTION('',(1.,0.,0.));
#22849=DIRECTION('center_axis',(1.,0.,0.));
#22850=DIRECTION('ref_axis',(0.,1.,-9.14588507257614E-13));
#22851=DIRECTION('',(1.,0.,0.));
#22852=DIRECTION('center_axis',(1.,0.,0.));
#22853=DIRECTION('ref_axis',(0.,1.,-9.14588507257614E-13));
#22854=DIRECTION('',(1.,0.,0.));
#22855=DIRECTION('center_axis',(1.,0.,0.));
#22856=DIRECTION('ref_axis',(0.,1.,-9.14588507257614E-13));
#22857=DIRECTION('',(1.,0.,0.));
#22858=DIRECTION('center_axis',(1.,0.,0.));
#22859=DIRECTION('ref_axis',(0.,1.,-9.14588507257614E-13));
#22860=DIRECTION('',(1.,0.,0.));
#22861=DIRECTION('center_axis',(1.,0.,0.));
#22862=DIRECTION('ref_axis',(0.,1.,-9.14588507257614E-13));
#22863=DIRECTION('',(1.,0.,0.));
#22864=DIRECTION('center_axis',(1.,0.,0.));
#22865=DIRECTION('ref_axis',(0.,1.,-9.14588507257614E-13));
#22866=DIRECTION('',(1.,0.,0.));
#22867=DIRECTION('center_axis',(1.,0.,0.));
#22868=DIRECTION('ref_axis',(0.,1.,-9.14588507257614E-13));
#22869=DIRECTION('',(1.,0.,0.));
#22870=DIRECTION('center_axis',(1.,0.,0.));
#22871=DIRECTION('ref_axis',(0.,1.,-9.14588507257614E-13));
#22872=DIRECTION('',(1.,0.,0.));
#22873=DIRECTION('center_axis',(1.,0.,0.));
#22874=DIRECTION('ref_axis',(0.,1.,-9.14588507257614E-13));
#22875=DIRECTION('',(1.,0.,0.));
#22876=DIRECTION('center_axis',(1.,0.,0.));
#22877=DIRECTION('ref_axis',(0.,1.,-9.14588507257614E-13));
#22878=DIRECTION('',(1.,0.,0.));
#22879=DIRECTION('center_axis',(1.,0.,0.));
#22880=DIRECTION('ref_axis',(0.,1.,-9.14588507257614E-13));
#22881=DIRECTION('',(1.,0.,0.));
#22882=DIRECTION('center_axis',(1.,0.,0.));
#22883=DIRECTION('ref_axis',(0.,1.,-9.14588507257614E-13));
#22884=DIRECTION('',(1.,0.,0.));
#22885=DIRECTION('center_axis',(1.,0.,0.));
#22886=DIRECTION('ref_axis',(0.,1.,-9.14588507257614E-13));
#22887=DIRECTION('',(1.,0.,0.));
#22888=DIRECTION('center_axis',(1.,0.,0.));
#22889=DIRECTION('ref_axis',(0.,1.,-9.14588507257614E-13));
#22890=DIRECTION('',(1.,0.,0.));
#22891=DIRECTION('center_axis',(1.,0.,0.));
#22892=DIRECTION('ref_axis',(0.,1.,-9.14588507257614E-13));
#22893=DIRECTION('',(1.,0.,0.));
#22894=DIRECTION('center_axis',(1.,0.,0.));
#22895=DIRECTION('ref_axis',(0.,1.,-9.14588507257614E-13));
#22896=DIRECTION('',(1.,0.,0.));
#22897=DIRECTION('center_axis',(1.,0.,0.));
#22898=DIRECTION('ref_axis',(0.,1.,-9.14588507257614E-13));
#22899=DIRECTION('',(1.,0.,0.));
#22900=DIRECTION('center_axis',(1.,0.,0.));
#22901=DIRECTION('ref_axis',(0.,1.,-9.14588507257614E-13));
#22902=DIRECTION('',(1.,0.,0.));
#22903=DIRECTION('center_axis',(1.,0.,0.));
#22904=DIRECTION('ref_axis',(0.,1.,-9.14588507257614E-13));
#22905=DIRECTION('',(1.,0.,0.));
#22906=DIRECTION('center_axis',(1.,0.,0.));
#22907=DIRECTION('ref_axis',(0.,1.,-9.14588507257614E-13));
#22908=DIRECTION('',(1.,0.,0.));
#22909=DIRECTION('center_axis',(1.,0.,0.));
#22910=DIRECTION('ref_axis',(0.,1.,-9.14588507257614E-13));
#22911=DIRECTION('',(1.,0.,0.));
#22912=DIRECTION('center_axis',(1.,0.,0.));
#22913=DIRECTION('ref_axis',(0.,1.,-9.14588507257614E-13));
#22914=DIRECTION('',(1.,0.,0.));
#22915=DIRECTION('center_axis',(0.,0.,1.));
#22916=DIRECTION('ref_axis',(1.,0.,0.));
#22917=DIRECTION('',(0.,1.,0.));
#22918=DIRECTION('',(0.,-1.,0.));
#22919=DIRECTION('center_axis',(-1.,0.,0.));
#22920=DIRECTION('ref_axis',(0.,-1.,0.));
#22921=DIRECTION('',(0.,1.,0.));
#22922=DIRECTION('center_axis',(0.,0.,-1.));
#22923=DIRECTION('ref_axis',(-1.,0.,0.));
#22924=DIRECTION('',(0.,-1.,0.));
#22925=DIRECTION('center_axis',(1.,0.,0.));
#22926=DIRECTION('ref_axis',(0.,1.,0.));
#22927=DIRECTION('center_axis',(1.,0.,0.));
#22928=DIRECTION('ref_axis',(0.,0.,-1.));
#22929=DIRECTION('center_axis',(-1.,0.,0.));
#22930=DIRECTION('ref_axis',(0.,1.,0.));
#22931=DIRECTION('center_axis',(-1.,0.,0.));
#22932=DIRECTION('ref_axis',(0.,1.,0.));
#22933=DIRECTION('center_axis',(1.,0.,0.));
#22934=DIRECTION('ref_axis',(0.,0.,-1.));
#22935=DIRECTION('center_axis',(-1.,0.,0.));
#22936=DIRECTION('ref_axis',(0.,1.,-9.14588507257614E-13));
#22937=DIRECTION('center_axis',(1.,0.,0.));
#22938=DIRECTION('ref_axis',(0.,-0.298235389366233,0.95449235331121));
#22939=DIRECTION('center_axis',(1.,0.,0.));
#22940=DIRECTION('ref_axis',(0.,0.,-1.));
#22941=DIRECTION('center_axis',(1.,0.,0.));
#22942=DIRECTION('ref_axis',(0.,1.,0.));
#22943=DIRECTION('center_axis',(1.,0.,0.));
#22944=DIRECTION('ref_axis',(0.,1.,0.));
#22945=DIRECTION('center_axis',(1.,0.,0.));
#22946=DIRECTION('ref_axis',(0.,0.,-1.));
#22947=DIRECTION('center_axis',(-1.,0.,0.));
#22948=DIRECTION('ref_axis',(0.,1.,9.92840284004976E-14));
#22949=DIRECTION('center_axis',(1.,0.,0.));
#22950=DIRECTION('ref_axis',(0.,0.815561733925156,0.578670077122528));
#22951=DIRECTION('center_axis',(1.,0.,0.));
#22952=DIRECTION('ref_axis',(0.,1.,0.));
#22953=DIRECTION('center_axis',(1.,0.,0.));
#22954=DIRECTION('ref_axis',(0.,1.,0.));
#22955=DIRECTION('center_axis',(1.,0.,0.));
#22956=DIRECTION('ref_axis',(0.,-0.406736643075801,-0.913545457642601));
#22957=DIRECTION('center_axis',(1.,0.,0.));
#22958=DIRECTION('ref_axis',(0.,0.,-1.));
#22959=DIRECTION('center_axis',(1.,0.,0.));
#22960=DIRECTION('ref_axis',(0.,0.954766869449684,-0.297355385021442));
#22961=DIRECTION('',(1.,0.,0.));
#22962=DIRECTION('center_axis',(1.,0.,0.));
#22963=DIRECTION('ref_axis',(0.,0.954766869449684,-0.297355385021442));
#22964=DIRECTION('',(1.,0.,0.));
#22965=DIRECTION('center_axis',(-1.,0.,0.));
#22966=DIRECTION('ref_axis',(0.,0.954766869449684,-0.297355385021442));
#22967=DIRECTION('center_axis',(1.,0.,0.));
#22968=DIRECTION('ref_axis',(0.,-0.406736643075801,-0.913545457642601));
#22969=DIRECTION('center_axis',(1.,0.,0.));
#22970=DIRECTION('ref_axis',(0.,0.,-1.));
#22971=DIRECTION('center_axis',(1.,0.,0.));
#22972=DIRECTION('ref_axis',(0.,1.,0.));
#22973=DIRECTION('center_axis',(1.,0.,0.));
#22974=DIRECTION('ref_axis',(0.,0.,-1.));
#22975=DIRECTION('center_axis',(1.,0.,0.));
#22976=DIRECTION('ref_axis',(0.,0.,-1.));
#22977=DIRECTION('center_axis',(1.,0.,0.));
#22978=DIRECTION('ref_axis',(0.,1.,0.));
#22979=DIRECTION('center_axis',(1.,0.,0.));
#22980=DIRECTION('ref_axis',(0.,0.,-1.));
#22981=DIRECTION('center_axis',(1.,0.,0.));
#22982=DIRECTION('ref_axis',(0.,0.,-1.));
#22983=DIRECTION('center_axis',(1.,0.,0.));
#22984=DIRECTION('ref_axis',(0.,1.,0.));
#22985=DIRECTION('center_axis',(1.,0.,0.));
#22986=DIRECTION('ref_axis',(0.,0.,-1.));
#22987=DIRECTION('center_axis',(-1.,0.,0.));
#22988=DIRECTION('ref_axis',(0.,1.,0.));
#22989=DIRECTION('center_axis',(1.,0.,0.));
#22990=DIRECTION('ref_axis',(0.,0.,-1.));
#22991=DIRECTION('center_axis',(1.,0.,0.));
#22992=DIRECTION('ref_axis',(0.,-0.743144825477395,-0.669130606358858));
#22993=DIRECTION('center_axis',(1.,0.,0.));
#22994=DIRECTION('ref_axis',(0.,0.,-1.));
#22995=DIRECTION('center_axis',(1.,0.,0.));
#22996=DIRECTION('ref_axis',(0.,0.751277605589271,-0.65998633269186));
#22997=DIRECTION('',(1.,0.,0.));
#22998=DIRECTION('center_axis',(1.,0.,0.));
#22999=DIRECTION('ref_axis',(0.,0.751277605589271,-0.65998633269186));
#23000=DIRECTION('',(1.,0.,0.));
#23001=DIRECTION('center_axis',(-1.,0.,0.));
#23002=DIRECTION('ref_axis',(0.,0.751277605589271,-0.65998633269186));
#23003=DIRECTION('center_axis',(1.,0.,0.));
#23004=DIRECTION('ref_axis',(0.,-0.743144825477395,-0.669130606358858));
#23005=DIRECTION('center_axis',(1.,0.,0.));
#23006=DIRECTION('ref_axis',(0.,0.,-1.));
#23007=DIRECTION('center_axis',(1.,0.,0.));
#23008=DIRECTION('ref_axis',(0.,1.,0.));
#23009=DIRECTION('center_axis',(1.,0.,0.));
#23010=DIRECTION('ref_axis',(0.,0.,-1.));
#23011=DIRECTION('center_axis',(1.,0.,0.));
#23012=DIRECTION('ref_axis',(0.,0.,-1.));
#23013=DIRECTION('center_axis',(1.,0.,0.));
#23014=DIRECTION('ref_axis',(0.,1.,0.));
#23015=DIRECTION('center_axis',(1.,0.,0.));
#23016=DIRECTION('ref_axis',(0.,0.,-1.));
#23017=DIRECTION('center_axis',(-1.,0.,0.));
#23018=DIRECTION('ref_axis',(0.,1.,0.));
#23019=DIRECTION('center_axis',(1.,0.,0.));
#23020=DIRECTION('ref_axis',(0.,0.,-1.));
#23021=DIRECTION('center_axis',(1.,0.,0.));
#23022=DIRECTION('ref_axis',(0.,-0.951056516295154,-0.309016994374947));
#23023=DIRECTION('center_axis',(1.,0.,0.));
#23024=DIRECTION('ref_axis',(0.,0.,-1.));
#23025=DIRECTION('center_axis',(1.,0.,0.));
#23026=DIRECTION('ref_axis',(0.,0.417885618579693,-0.908499647652253));
#23027=DIRECTION('',(1.,0.,0.));
#23028=DIRECTION('center_axis',(1.,0.,0.));
#23029=DIRECTION('ref_axis',(0.,0.417885618579693,-0.908499647652253));
#23030=DIRECTION('',(1.,0.,0.));
#23031=DIRECTION('center_axis',(-1.,0.,0.));
#23032=DIRECTION('ref_axis',(0.,0.417885618579693,-0.908499647652253));
#23033=DIRECTION('center_axis',(1.,0.,0.));
#23034=DIRECTION('ref_axis',(0.,-0.951056516295154,-0.309016994374947));
#23035=DIRECTION('center_axis',(1.,0.,0.));
#23036=DIRECTION('ref_axis',(0.,0.,-1.));
#23037=DIRECTION('center_axis',(1.,0.,0.));
#23038=DIRECTION('ref_axis',(0.,1.,0.));
#23039=DIRECTION('center_axis',(1.,0.,0.));
#23040=DIRECTION('ref_axis',(0.,0.,-1.));
#23041=DIRECTION('center_axis',(1.,0.,0.));
#23042=DIRECTION('ref_axis',(0.,0.,-1.));
#23043=DIRECTION('center_axis',(1.,0.,0.));
#23044=DIRECTION('ref_axis',(0.,1.,0.));
#23045=DIRECTION('center_axis',(1.,0.,0.));
#23046=DIRECTION('ref_axis',(0.,0.,-1.));
#23047=DIRECTION('center_axis',(-1.,0.,0.));
#23048=DIRECTION('ref_axis',(0.,1.,0.));
#23049=DIRECTION('center_axis',(1.,0.,0.));
#23050=DIRECTION('ref_axis',(0.,0.,-1.));
#23051=DIRECTION('center_axis',(1.,0.,0.));
#23052=DIRECTION('ref_axis',(0.,-0.994521895368273,0.104528463267654));
#23053=DIRECTION('center_axis',(1.,0.,0.));
#23054=DIRECTION('ref_axis',(0.,0.,-1.));
#23055=DIRECTION('center_axis',(1.,0.,0.));
#23056=DIRECTION('ref_axis',(0.,0.0122374117460222,-0.999925120073377));
#23057=DIRECTION('',(1.,0.,0.));
#23058=DIRECTION('center_axis',(1.,0.,0.));
#23059=DIRECTION('ref_axis',(0.,0.0122374117460222,-0.999925120073377));
#23060=DIRECTION('',(1.,0.,0.));
#23061=DIRECTION('center_axis',(-1.,0.,0.));
#23062=DIRECTION('ref_axis',(0.,0.0122374117460222,-0.999925120073377));
#23063=DIRECTION('center_axis',(1.,0.,0.));
#23064=DIRECTION('ref_axis',(0.,-0.994521895368273,0.104528463267654));
#23065=DIRECTION('center_axis',(1.,0.,0.));
#23066=DIRECTION('ref_axis',(0.,0.,-1.));
#23067=DIRECTION('center_axis',(1.,0.,0.));
#23068=DIRECTION('ref_axis',(0.,1.,0.));
#23069=DIRECTION('center_axis',(1.,0.,0.));
#23070=DIRECTION('ref_axis',(0.,0.,-1.));
#23071=DIRECTION('center_axis',(1.,0.,0.));
#23072=DIRECTION('ref_axis',(0.,0.,-1.));
#23073=DIRECTION('center_axis',(1.,0.,0.));
#23074=DIRECTION('ref_axis',(0.,1.,0.));
#23075=DIRECTION('center_axis',(1.,0.,0.));
#23076=DIRECTION('ref_axis',(0.,0.,-1.));
#23077=DIRECTION('center_axis',(-1.,0.,0.));
#23078=DIRECTION('ref_axis',(0.,1.,0.));
#23079=DIRECTION('center_axis',(1.,0.,0.));
#23080=DIRECTION('ref_axis',(0.,0.,-1.));
#23081=DIRECTION('center_axis',(1.,0.,0.));
#23082=DIRECTION('ref_axis',(0.,-0.866025403784438,0.5));
#23083=DIRECTION('center_axis',(1.,0.,0.));
#23084=DIRECTION('ref_axis',(0.,0.,-1.));
#23085=DIRECTION('center_axis',(1.,0.,0.));
#23086=DIRECTION('ref_axis',(0.,-0.395526754751931,-0.91845445519928));
#23087=DIRECTION('',(1.,0.,0.));
#23088=DIRECTION('center_axis',(1.,0.,0.));
#23089=DIRECTION('ref_axis',(0.,-0.395526754751931,-0.91845445519928));
#23090=DIRECTION('',(1.,0.,0.));
#23091=DIRECTION('center_axis',(-1.,0.,0.));
#23092=DIRECTION('ref_axis',(0.,-0.395526754751931,-0.91845445519928));
#23093=DIRECTION('center_axis',(1.,0.,0.));
#23094=DIRECTION('ref_axis',(0.,-0.866025403784438,0.5));
#23095=DIRECTION('center_axis',(1.,0.,0.));
#23096=DIRECTION('ref_axis',(0.,0.,-1.));
#23097=DIRECTION('center_axis',(1.,0.,0.));
#23098=DIRECTION('ref_axis',(0.,1.,0.));
#23099=DIRECTION('center_axis',(1.,0.,0.));
#23100=DIRECTION('ref_axis',(0.,0.,-1.));
#23101=DIRECTION('center_axis',(1.,0.,0.));
#23102=DIRECTION('ref_axis',(0.,0.,-1.));
#23103=DIRECTION('center_axis',(1.,0.,0.));
#23104=DIRECTION('ref_axis',(0.,1.,0.));
#23105=DIRECTION('center_axis',(1.,0.,0.));
#23106=DIRECTION('ref_axis',(0.,0.,-1.));
#23107=DIRECTION('center_axis',(-1.,0.,0.));
#23108=DIRECTION('ref_axis',(0.,1.,0.));
#23109=DIRECTION('center_axis',(1.,0.,0.));
#23110=DIRECTION('ref_axis',(0.,0.,-1.));
#23111=DIRECTION('center_axis',(1.,0.,0.));
#23112=DIRECTION('ref_axis',(0.,-0.587785252292473,0.809016994374947));
#23113=DIRECTION('center_axis',(1.,0.,0.));
#23114=DIRECTION('ref_axis',(0.,0.,-1.));
#23115=DIRECTION('center_axis',(1.,0.,0.));
#23116=DIRECTION('ref_axis',(0.,-0.734900752105513,-0.678174671124446));
#23117=DIRECTION('',(1.,0.,0.));
#23118=DIRECTION('center_axis',(1.,0.,0.));
#23119=DIRECTION('ref_axis',(0.,-0.734900752105513,-0.678174671124446));
#23120=DIRECTION('',(1.,0.,0.));
#23121=DIRECTION('center_axis',(-1.,0.,0.));
#23122=DIRECTION('ref_axis',(0.,-0.734900752105513,-0.678174671124446));
#23123=DIRECTION('center_axis',(1.,0.,0.));
#23124=DIRECTION('ref_axis',(0.,-0.587785252292473,0.809016994374947));
#23125=DIRECTION('center_axis',(1.,0.,0.));
#23126=DIRECTION('ref_axis',(0.,0.,-1.));
#23127=DIRECTION('center_axis',(1.,0.,0.));
#23128=DIRECTION('ref_axis',(0.,1.,0.));
#23129=DIRECTION('center_axis',(1.,0.,0.));
#23130=DIRECTION('ref_axis',(0.,0.,-1.));
#23131=DIRECTION('center_axis',(1.,0.,0.));
#23132=DIRECTION('ref_axis',(0.,0.,-1.));
#23133=DIRECTION('center_axis',(1.,0.,0.));
#23134=DIRECTION('ref_axis',(0.,1.,0.));
#23135=DIRECTION('center_axis',(1.,0.,0.));
#23136=DIRECTION('ref_axis',(0.,0.,-1.));
#23137=DIRECTION('center_axis',(-1.,0.,0.));
#23138=DIRECTION('ref_axis',(0.,1.,0.));
#23139=DIRECTION('center_axis',(1.,0.,0.));
#23140=DIRECTION('ref_axis',(0.,0.,-1.));
#23141=DIRECTION('center_axis',(1.,0.,0.));
#23142=DIRECTION('ref_axis',(0.,-0.207911690817759,0.978147600733806));
#23143=DIRECTION('center_axis',(1.,0.,0.));
#23144=DIRECTION('ref_axis',(0.,0.,-1.));
#23145=DIRECTION('center_axis',(1.,0.,0.));
#23146=DIRECTION('ref_axis',(0.,-0.947203733056315,-0.320632325388725));
#23147=DIRECTION('',(1.,0.,0.));
#23148=DIRECTION('center_axis',(1.,0.,0.));
#23149=DIRECTION('ref_axis',(0.,-0.947203733056315,-0.320632325388725));
#23150=DIRECTION('',(1.,0.,0.));
#23151=DIRECTION('center_axis',(-1.,0.,0.));
#23152=DIRECTION('ref_axis',(0.,-0.947203733056315,-0.320632325388725));
#23153=DIRECTION('center_axis',(1.,0.,0.));
#23154=DIRECTION('ref_axis',(0.,-0.207911690817759,0.978147600733806));
#23155=DIRECTION('center_axis',(1.,0.,0.));
#23156=DIRECTION('ref_axis',(0.,0.,-1.));
#23157=DIRECTION('center_axis',(1.,0.,0.));
#23158=DIRECTION('ref_axis',(0.,1.,0.));
#23159=DIRECTION('center_axis',(1.,0.,0.));
#23160=DIRECTION('ref_axis',(0.,0.,-1.));
#23161=DIRECTION('center_axis',(1.,0.,0.));
#23162=DIRECTION('ref_axis',(0.,0.,-1.));
#23163=DIRECTION('center_axis',(1.,0.,0.));
#23164=DIRECTION('ref_axis',(0.,1.,0.));
#23165=DIRECTION('center_axis',(1.,0.,0.));
#23166=DIRECTION('ref_axis',(0.,0.,-1.));
#23167=DIRECTION('center_axis',(-1.,0.,0.));
#23168=DIRECTION('ref_axis',(0.,1.,0.));
#23169=DIRECTION('center_axis',(1.,0.,0.));
#23170=DIRECTION('ref_axis',(0.,0.,-1.));
#23171=DIRECTION('center_axis',(1.,0.,0.));
#23172=DIRECTION('ref_axis',(0.,0.20791169081776,0.978147600733805));
#23173=DIRECTION('center_axis',(1.,0.,0.));
#23174=DIRECTION('ref_axis',(0.,0.,-1.));
#23175=DIRECTION('center_axis',(1.,0.,0.));
#23176=DIRECTION('ref_axis',(0.,0.,-1.));
#23177=DIRECTION('center_axis',(1.,0.,0.));
#23178=DIRECTION('ref_axis',(0.,-0.995726583485909,0.0923502622599377));
#23179=DIRECTION('',(1.,0.,0.));
#23180=DIRECTION('center_axis',(1.,0.,0.));
#23181=DIRECTION('ref_axis',(0.,-0.995726583485909,0.0923502622599377));
#23182=DIRECTION('',(1.,0.,0.));
#23183=DIRECTION('center_axis',(-1.,0.,0.));
#23184=DIRECTION('ref_axis',(0.,-0.995726583485909,0.0923502622599377));
#23185=DIRECTION('center_axis',(1.,0.,0.));
#23186=DIRECTION('ref_axis',(0.,0.20791169081776,0.978147600733805));
#23187=DIRECTION('center_axis',(1.,0.,0.));
#23188=DIRECTION('ref_axis',(0.,0.,-1.));
#23189=DIRECTION('center_axis',(1.,0.,0.));
#23190=DIRECTION('ref_axis',(0.,0.,-1.));
#23191=DIRECTION('center_axis',(1.,0.,0.));
#23192=DIRECTION('ref_axis',(0.,1.,0.));
#23193=DIRECTION('center_axis',(1.,0.,0.));
#23194=DIRECTION('ref_axis',(0.,0.,-1.));
#23195=DIRECTION('center_axis',(1.,0.,0.));
#23196=DIRECTION('ref_axis',(0.,0.,-1.));
#23197=DIRECTION('center_axis',(1.,0.,0.));
#23198=DIRECTION('ref_axis',(0.,1.,0.));
#23199=DIRECTION('center_axis',(1.,0.,0.));
#23200=DIRECTION('ref_axis',(0.,0.,-1.));
#23201=DIRECTION('center_axis',(-1.,0.,0.));
#23202=DIRECTION('ref_axis',(0.,1.,0.));
#23203=DIRECTION('center_axis',(1.,0.,0.));
#23204=DIRECTION('ref_axis',(0.,0.,-1.));
#23205=DIRECTION('center_axis',(1.,0.,0.));
#23206=DIRECTION('ref_axis',(0.,0.587785252292473,0.809016994374947));
#23207=DIRECTION('center_axis',(1.,0.,0.));
#23208=DIRECTION('ref_axis',(0.,0.,-1.));
#23209=DIRECTION('center_axis',(1.,0.,0.));
#23210=DIRECTION('ref_axis',(0.,-0.872079261738761,0.489364650588063));
#23211=DIRECTION('',(1.,0.,0.));
#23212=DIRECTION('center_axis',(1.,0.,0.));
#23213=DIRECTION('ref_axis',(0.,-0.872079261738761,0.489364650588063));
#23214=DIRECTION('',(1.,0.,0.));
#23215=DIRECTION('center_axis',(-1.,0.,0.));
#23216=DIRECTION('ref_axis',(0.,-0.872079261738761,0.489364650588063));
#23217=DIRECTION('center_axis',(1.,0.,0.));
#23218=DIRECTION('ref_axis',(0.,0.587785252292473,0.809016994374947));
#23219=DIRECTION('center_axis',(1.,0.,0.));
#23220=DIRECTION('ref_axis',(0.,0.,-1.));
#23221=DIRECTION('center_axis',(1.,0.,0.));
#23222=DIRECTION('ref_axis',(0.,1.,0.));
#23223=DIRECTION('center_axis',(1.,0.,0.));
#23224=DIRECTION('ref_axis',(0.,0.,-1.));
#23225=DIRECTION('center_axis',(1.,0.,0.));
#23226=DIRECTION('ref_axis',(0.,0.,-1.));
#23227=DIRECTION('center_axis',(1.,0.,0.));
#23228=DIRECTION('ref_axis',(0.,1.,0.));
#23229=DIRECTION('center_axis',(1.,0.,0.));
#23230=DIRECTION('ref_axis',(0.,0.,-1.));
#23231=DIRECTION('center_axis',(-1.,0.,0.));
#23232=DIRECTION('ref_axis',(0.,1.,0.));
#23233=DIRECTION('center_axis',(1.,0.,0.));
#23234=DIRECTION('ref_axis',(0.,0.,-1.));
#23235=DIRECTION('center_axis',(1.,0.,0.));
#23236=DIRECTION('ref_axis',(0.,0.866025403784439,0.5));
#23237=DIRECTION('center_axis',(1.,0.,0.));
#23238=DIRECTION('ref_axis',(0.,0.,-1.));
#23239=DIRECTION('center_axis',(1.,0.,0.));
#23240=DIRECTION('ref_axis',(0.,-0.597641513045608,0.801763445091229));
#23241=DIRECTION('',(1.,0.,0.));
#23242=DIRECTION('center_axis',(1.,0.,0.));
#23243=DIRECTION('ref_axis',(0.,-0.597641513045608,0.801763445091229));
#23244=DIRECTION('',(1.,0.,0.));
#23245=DIRECTION('center_axis',(-1.,0.,0.));
#23246=DIRECTION('ref_axis',(0.,-0.597641513045608,0.801763445091229));
#23247=DIRECTION('center_axis',(1.,0.,0.));
#23248=DIRECTION('ref_axis',(0.,0.866025403784439,0.5));
#23249=DIRECTION('center_axis',(1.,0.,0.));
#23250=DIRECTION('ref_axis',(0.,0.,-1.));
#23251=DIRECTION('center_axis',(1.,0.,0.));
#23252=DIRECTION('ref_axis',(0.,1.,0.));
#23253=DIRECTION('center_axis',(1.,0.,0.));
#23254=DIRECTION('ref_axis',(0.,0.,-1.));
#23255=DIRECTION('center_axis',(1.,0.,0.));
#23256=DIRECTION('ref_axis',(0.,0.,-1.));
#23257=DIRECTION('center_axis',(1.,0.,0.));
#23258=DIRECTION('ref_axis',(0.,1.,0.));
#23259=DIRECTION('center_axis',(1.,0.,0.));
#23260=DIRECTION('ref_axis',(0.,0.,-1.));
#23261=DIRECTION('center_axis',(-1.,0.,0.));
#23262=DIRECTION('ref_axis',(0.,1.,0.));
#23263=DIRECTION('center_axis',(1.,0.,0.));
#23264=DIRECTION('ref_axis',(0.,0.,-1.));
#23265=DIRECTION('center_axis',(1.,0.,0.));
#23266=DIRECTION('ref_axis',(0.,0.994521895368273,0.104528463267653));
#23267=DIRECTION('center_axis',(1.,0.,0.));
#23268=DIRECTION('ref_axis',(0.,0.,-1.));
#23269=DIRECTION('center_axis',(1.,0.,0.));
#23270=DIRECTION('ref_axis',(0.,-0.219866117344171,0.975530056145888));
#23271=DIRECTION('',(1.,0.,0.));
#23272=DIRECTION('center_axis',(1.,0.,0.));
#23273=DIRECTION('ref_axis',(0.,-0.219866117344171,0.975530056145888));
#23274=DIRECTION('',(1.,0.,0.));
#23275=DIRECTION('center_axis',(-1.,0.,0.));
#23276=DIRECTION('ref_axis',(0.,-0.219866117344171,0.975530056145888));
#23277=DIRECTION('center_axis',(1.,0.,0.));
#23278=DIRECTION('ref_axis',(0.,0.994521895368273,0.104528463267653));
#23279=DIRECTION('center_axis',(1.,0.,0.));
#23280=DIRECTION('ref_axis',(0.,0.,-1.));
#23281=DIRECTION('center_axis',(1.,0.,0.));
#23282=DIRECTION('ref_axis',(0.,1.,0.));
#23283=DIRECTION('center_axis',(1.,0.,0.));
#23284=DIRECTION('ref_axis',(0.,0.,-1.));
#23285=DIRECTION('center_axis',(1.,0.,0.));
#23286=DIRECTION('ref_axis',(0.,0.,-1.));
#23287=DIRECTION('center_axis',(1.,0.,0.));
#23288=DIRECTION('ref_axis',(0.,1.,0.));
#23289=DIRECTION('center_axis',(1.,0.,0.));
#23290=DIRECTION('ref_axis',(0.,0.,-1.));
#23291=DIRECTION('center_axis',(-1.,0.,0.));
#23292=DIRECTION('ref_axis',(0.,1.,0.));
#23293=DIRECTION('center_axis',(1.,0.,0.));
#23294=DIRECTION('ref_axis',(0.,0.,-1.));
#23295=DIRECTION('center_axis',(1.,0.,0.));
#23296=DIRECTION('ref_axis',(0.,0.951056516295154,-0.309016994374948));
#23297=DIRECTION('center_axis',(1.,0.,0.));
#23298=DIRECTION('ref_axis',(0.,0.,-1.));
#23299=DIRECTION('center_axis',(1.,0.,0.));
#23300=DIRECTION('ref_axis',(0.,0.195926127467043,0.980618658080585));
#23301=DIRECTION('',(1.,0.,0.));
#23302=DIRECTION('center_axis',(1.,0.,0.));
#23303=DIRECTION('ref_axis',(0.,0.195926127467043,0.980618658080585));
#23304=DIRECTION('',(1.,0.,0.));
#23305=DIRECTION('center_axis',(-1.,0.,0.));
#23306=DIRECTION('ref_axis',(0.,0.195926127467043,0.980618658080585));
#23307=DIRECTION('center_axis',(1.,0.,0.));
#23308=DIRECTION('ref_axis',(0.,0.951056516295154,-0.309016994374948));
#23309=DIRECTION('center_axis',(1.,0.,0.));
#23310=DIRECTION('ref_axis',(0.,0.,-1.));
#23311=DIRECTION('center_axis',(1.,0.,0.));
#23312=DIRECTION('ref_axis',(0.,1.,0.));
#23313=DIRECTION('center_axis',(1.,0.,0.));
#23314=DIRECTION('ref_axis',(0.,0.,-1.));
#23315=DIRECTION('center_axis',(1.,0.,0.));
#23316=DIRECTION('ref_axis',(0.,0.,-1.));
#23317=DIRECTION('center_axis',(1.,0.,0.));
#23318=DIRECTION('ref_axis',(0.,1.,0.));
#23319=DIRECTION('center_axis',(1.,0.,0.));
#23320=DIRECTION('ref_axis',(0.,0.,-1.));
#23321=DIRECTION('center_axis',(-1.,0.,0.));
#23322=DIRECTION('ref_axis',(0.,1.,0.));
#23323=DIRECTION('center_axis',(1.,0.,0.));
#23324=DIRECTION('ref_axis',(0.,0.,-1.));
#23325=DIRECTION('center_axis',(1.,0.,0.));
#23326=DIRECTION('ref_axis',(0.,0.743144825477394,-0.669130606358858));
#23327=DIRECTION('center_axis',(1.,0.,0.));
#23328=DIRECTION('ref_axis',(0.,0.,-1.));
#23329=DIRECTION('center_axis',(1.,0.,0.));
#23330=DIRECTION('ref_axis',(0.,0.577840964906216,0.816149385392315));
#23331=DIRECTION('',(1.,0.,0.));
#23332=DIRECTION('center_axis',(1.,0.,0.));
#23333=DIRECTION('ref_axis',(0.,0.577840964906216,0.816149385392315));
#23334=DIRECTION('',(1.,0.,0.));
#23335=DIRECTION('center_axis',(-1.,0.,0.));
#23336=DIRECTION('ref_axis',(0.,0.577840964906216,0.816149385392315));
#23337=DIRECTION('center_axis',(1.,0.,0.));
#23338=DIRECTION('ref_axis',(0.,0.743144825477394,-0.669130606358858));
#23339=DIRECTION('center_axis',(1.,0.,0.));
#23340=DIRECTION('ref_axis',(0.,0.,-1.));
#23341=DIRECTION('center_axis',(1.,0.,0.));
#23342=DIRECTION('ref_axis',(0.,1.,0.));
#23343=DIRECTION('center_axis',(1.,0.,0.));
#23344=DIRECTION('ref_axis',(0.,0.,-1.));
#23345=DIRECTION('center_axis',(1.,0.,0.));
#23346=DIRECTION('ref_axis',(0.,0.,-1.));
#23347=DIRECTION('center_axis',(1.,0.,0.));
#23348=DIRECTION('ref_axis',(0.,1.,0.));
#23349=DIRECTION('center_axis',(1.,0.,0.));
#23350=DIRECTION('ref_axis',(0.,0.,-1.));
#23351=DIRECTION('center_axis',(-1.,0.,0.));
#23352=DIRECTION('ref_axis',(0.,1.,0.));
#23353=DIRECTION('center_axis',(1.,0.,0.));
#23354=DIRECTION('ref_axis',(0.,0.,-1.));
#23355=DIRECTION('center_axis',(1.,0.,0.));
#23356=DIRECTION('ref_axis',(0.,0.4067366430758,-0.913545457642601));
#23357=DIRECTION('center_axis',(1.,0.,0.));
#23358=DIRECTION('ref_axis',(0.,0.,-1.));
#23359=DIRECTION('center_axis',(1.,0.,0.));
#23360=DIRECTION('ref_axis',(0.,0.859841849992738,0.510560469485315));
#23361=DIRECTION('',(1.,0.,0.));
#23362=DIRECTION('center_axis',(1.,0.,0.));
#23363=DIRECTION('ref_axis',(0.,0.859841849992738,0.510560469485315));
#23364=DIRECTION('',(1.,0.,0.));
#23365=DIRECTION('center_axis',(-1.,0.,0.));
#23366=DIRECTION('ref_axis',(0.,0.859841849992738,0.510560469485315));
#23367=DIRECTION('center_axis',(1.,0.,0.));
#23368=DIRECTION('ref_axis',(0.,0.4067366430758,-0.913545457642601));
#23369=DIRECTION('center_axis',(1.,0.,0.));
#23370=DIRECTION('ref_axis',(0.,0.,-1.));
#23371=DIRECTION('center_axis',(1.,0.,0.));
#23372=DIRECTION('ref_axis',(0.,1.,0.));
#23373=DIRECTION('center_axis',(1.,0.,0.));
#23374=DIRECTION('ref_axis',(0.,0.,-1.));
#23375=DIRECTION('center_axis',(1.,0.,0.));
#23376=DIRECTION('ref_axis',(0.,0.,-1.));
#23377=DIRECTION('center_axis',(1.,0.,0.));
#23378=DIRECTION('ref_axis',(0.,1.,0.));
#23379=DIRECTION('center_axis',(1.,0.,0.));
#23380=DIRECTION('ref_axis',(0.,0.,-1.));
#23381=DIRECTION('center_axis',(-1.,0.,0.));
#23382=DIRECTION('ref_axis',(0.,1.,0.));
#23383=DIRECTION('center_axis',(1.,0.,0.));
#23384=DIRECTION('ref_axis',(0.,0.,-1.));
#23385=DIRECTION('',(1.,0.,0.));
#23386=DIRECTION('center_axis',(1.,0.,0.));
#23387=DIRECTION('ref_axis',(0.,0.,-1.));
#23388=DIRECTION('center_axis',(1.,0.,0.));
#23389=DIRECTION('ref_axis',(0.,0.,-1.));
#23390=DIRECTION('center_axis',(1.,0.,0.));
#23391=DIRECTION('ref_axis',(0.,0.993168267797538,0.116691010108051));
#23392=DIRECTION('center_axis',(1.,0.,0.));
#23393=DIRECTION('ref_axis',(0.,0.993168267797538,0.116691010108051));
#23394=DIRECTION('center_axis',(-1.,0.,0.));
#23395=DIRECTION('ref_axis',(0.,0.993168267797538,0.116691010108051));
#23396=DIRECTION('',(1.,0.,0.));
#23397=DIRECTION('center_axis',(1.,0.,0.));
#23398=DIRECTION('ref_axis',(0.,0.,-1.));
#23399=DIRECTION('center_axis',(1.,0.,0.));
#23400=DIRECTION('ref_axis',(0.,0.,-1.));
#23401=DIRECTION('center_axis',(-1.,0.,0.));
#23402=DIRECTION('ref_axis',(0.,1.,0.));
#23403=DIRECTION('center_axis',(1.,0.,0.));
#23404=DIRECTION('ref_axis',(0.,0.,-1.));
#23405=DIRECTION('center_axis',(1.,0.,0.));
#23406=DIRECTION('ref_axis',(0.,0.,-1.));
#23407=DIRECTION('center_axis',(1.,0.,0.));
#23408=DIRECTION('ref_axis',(0.,1.,0.));
#23409=DIRECTION('center_axis',(-1.,0.,0.));
#23410=DIRECTION('ref_axis',(0.,0.,1.));
#23411=DIRECTION('center_axis',(1.,0.,0.));
#23412=DIRECTION('ref_axis',(0.,0.,-1.));
#23413=DIRECTION('center_axis',(1.,0.,0.));
#23414=DIRECTION('ref_axis',(0.,1.,0.));
#23415=DIRECTION('',(-0.707106781186546,0.707106781186549,8.65956056235495E-17));
#23416=DIRECTION('center_axis',(1.,0.,0.));
#23417=DIRECTION('ref_axis',(0.,1.,0.));
#23418=DIRECTION('',(-0.157990501106675,0.987440631916705,1.20926600922483E-16));
#23419=DIRECTION('center_axis',(-1.,0.,0.));
#23420=DIRECTION('ref_axis',(0.,1.,0.));
#23421=DIRECTION('',(-0.157990501106672,-0.987440631916706,-1.20926600922483E-16));
#23422=DIRECTION('center_axis',(1.,0.,0.));
#23423=DIRECTION('ref_axis',(0.,1.,0.));
#23424=DIRECTION('center_axis',(-1.,0.,0.));
#23425=DIRECTION('ref_axis',(0.,1.,0.));
#23426=DIRECTION('center_axis',(-1.,0.,0.));
#23427=DIRECTION('ref_axis',(0.,1.,0.));
#23428=DIRECTION('center_axis',(1.,0.,0.));
#23429=DIRECTION('ref_axis',(0.,0.,-1.));
#23430=DIRECTION('',(-0.707106781186546,-0.707106781186549,-8.65956056235495E-17));
#23431=DIRECTION('center_axis',(1.,0.,0.));
#23432=DIRECTION('ref_axis',(0.,0.,-1.));
#23433=DIRECTION('axis',(0.,0.,1.));
#23434=DIRECTION('refdir',(1.,0.,0.));
#23435=DIRECTION('center_axis',(0.,-0.707106781186548,-0.707106781186547));
#23436=DIRECTION('ref_axis',(0.38268343236509,-0.653281482438183,0.653281482438193));
#23437=DIRECTION('center_axis',(-8.8931018167636E-15,0.707106781186548,
0.707106781186548));
#23438=DIRECTION('ref_axis',(2.22044604925032E-15,-0.707106781186548,0.707106781186548));
#23439=DIRECTION('',(0.,0.707106781186548,0.707106781186547));
#23440=DIRECTION('center_axis',(-3.6799042000401E-15,-0.707106781186556,
-0.707106781186539));
#23441=DIRECTION('ref_axis',(0.707106781186546,-0.499999999999997,0.500000000000005));
#23442=DIRECTION('',(0.,-0.707106781186548,-0.707106781186547));
#23443=DIRECTION('center_axis',(-3.5527136788005E-15,-1.,-7.105427357601E-15));
#23444=DIRECTION('ref_axis',(0.505449465124414,-7.10542735760101E-15,0.862856209461022));
#23445=DIRECTION('center_axis',(0.,-0.707106781186547,0.707106781186548));
#23446=DIRECTION('ref_axis',(0.382683432365091,0.653281482438193,0.653281482438184));
#23447=DIRECTION('center_axis',(1.,0.,0.));
#23448=DIRECTION('ref_axis',(0.,0.,1.));
#23449=DIRECTION('center_axis',(-0.577350269189627,4.48691293489498E-16,
0.816496580927725));
#23450=DIRECTION('ref_axis',(0.816496580927726,0.,0.577350269189626));
#23451=DIRECTION('center_axis',(0.577350269189627,0.816496580927725,0.));
#23452=DIRECTION('ref_axis',(0.816496580927726,-0.577350269189625,0.));
#23453=DIRECTION('center_axis',(-0.577350269189625,-0.816496580927727,1.25192883228097E-15));
#23454=DIRECTION('ref_axis',(0.707106781186548,-0.5,-0.5));
#23455=DIRECTION('',(-0.577350269189627,-0.816496580927725,-2.7755575615629E-17));
#23456=DIRECTION('center_axis',(-0.577350269189627,-0.816496580927725,1.25192883228098E-15));
#23457=DIRECTION('ref_axis',(0.707106781186547,-0.5,-0.5));
#23458=DIRECTION('',(0.577350269189627,0.816496580927725,-2.7755575615629E-17));
#23459=DIRECTION('center_axis',(0.,-0.707106781186548,0.707106781186547));
#23460=DIRECTION('ref_axis',(0.923879532511285,-0.270598050073102,-0.270598050073102));
#23461=DIRECTION('center_axis',(0.,-0.707106781186548,0.707106781186548));
#23462=DIRECTION('ref_axis',(0.707106781186546,-0.500000000000001,-0.500000000000001));
#23463=DIRECTION('',(0.,-0.707106781186548,0.707106781186547));
#23464=DIRECTION('center_axis',(0.,0.707106781186548,-0.707106781186548));
#23465=DIRECTION('ref_axis',(1.,0.,0.));
#23466=DIRECTION('',(0.,0.707106781186548,-0.707106781186547));
#23467=DIRECTION('center_axis',(0.,0.,1.));
#23468=DIRECTION('ref_axis',(1.,0.,0.));
#23469=DIRECTION('center_axis',(0.,-0.707106781186548,-0.707106781186547));
#23470=DIRECTION('ref_axis',(0.923879532511286,-0.270598050073101,0.270598050073101));
#23471=DIRECTION('center_axis',(0.,0.,1.));
#23472=DIRECTION('ref_axis',(1.,0.,0.));
#23473=DIRECTION('center_axis',(0.,-0.707106781186547,0.707106781186548));
#23474=DIRECTION('ref_axis',(0.382683432365089,0.653281482438189,0.653281482438189));
#23475=DIRECTION('center_axis',(-0.577350269189627,0.816496580927725,-1.92296268638356E-16));
#23476=DIRECTION('ref_axis',(0.816496580927725,0.577350269189628,0.));
#23477=DIRECTION('center_axis',(0.,0.707106781186548,0.707106781186548));
#23478=DIRECTION('ref_axis',(0.707106781186548,0.5,-0.5));
#23479=DIRECTION('center_axis',(1.,0.,0.));
#23480=DIRECTION('ref_axis',(0.,1.,0.));
#23481=DIRECTION('center_axis',(0.,0.707106781186548,0.707106781186548));
#23482=DIRECTION('ref_axis',(0.382683432365087,0.653281482438192,-0.653281482438187));
#23483=DIRECTION('center_axis',(3.12791857003412E-15,0.707106781186545,
0.70710678118655));
#23484=DIRECTION('ref_axis',(0.707106781186547,0.5,-0.5));
#23485=DIRECTION('',(0.,0.707106781186547,0.707106781186547));
#23486=DIRECTION('',(0.,-0.707106781186547,-0.707106781186547));
#23487=DIRECTION('center_axis',(0.577350269189627,-1.92296268638356E-16,
0.816496580927725));
#23488=DIRECTION('ref_axis',(0.816496580927726,0.,-0.577350269189626));
#23489=DIRECTION('center_axis',(-0.577350269189628,4.90756102254141E-15,
-0.816496580927725));
#23490=DIRECTION('ref_axis',(0.707106781186548,0.5,-0.5));
#23491=DIRECTION('',(-0.577350269189627,1.92296268638356E-16,-0.816496580927725));
#23492=DIRECTION('center_axis',(-0.577350269189625,0.,-0.816496580927726));
#23493=DIRECTION('ref_axis',(0.707106781186548,0.5,-0.5));
#23494=DIRECTION('',(0.577350269189627,-1.92296268638356E-16,0.816496580927725));
#23495=DIRECTION('center_axis',(0.,0.,1.));
#23496=DIRECTION('ref_axis',(1.,0.,0.));
#23497=DIRECTION('center_axis',(0.,-0.707106781186548,-0.707106781186548));
#23498=DIRECTION('ref_axis',(0.92387953251129,0.270598050073092,-0.270598050073092));
#23499=DIRECTION('center_axis',(-0.577350269189627,4.48691293489498E-16,
0.816496580927725));
#23500=DIRECTION('ref_axis',(0.816496580927726,0.,0.577350269189626));
#23501=DIRECTION('',(0.577350269189627,-4.76446869105127E-16,-0.816496580927725));
#23502=DIRECTION('center_axis',(-0.577350269189626,0.,0.816496580927726));
#23503=DIRECTION('ref_axis',(0.707106781186547,-0.5,0.5));
#23504=DIRECTION('',(-0.577350269189627,4.20935717873869E-16,0.816496580927725));
#23505=DIRECTION('center_axis',(0.707106781186546,-0.5,0.500000000000001));
#23506=DIRECTION('ref_axis',(0.577350269189627,0.,-0.816496580927725));
#23507=DIRECTION('',(0.,-0.707106781186548,-0.707106781186547));
#23508=DIRECTION('center_axis',(0.,0.707106781186548,0.707106781186547));
#23509=DIRECTION('ref_axis',(0.923879532511287,-0.270598050073103,0.270598050073094));
#23510=DIRECTION('',(0.,0.707106781186548,0.707106781186547));
#23511=DIRECTION('center_axis',(0.,-0.707106781186548,-0.707106781186548));
#23512=DIRECTION('ref_axis',(1.,0.,0.));
#23513=DIRECTION('center_axis',(1.,0.,0.));
#23514=DIRECTION('ref_axis',(0.,0.,-1.));
#23515=DIRECTION('',(0.,-0.707106781186548,-0.707106781186548));
#23516=DIRECTION('',(0.,0.707106781186547,-0.707106781186548));
#23517=DIRECTION('center_axis',(0.,-0.707106781186548,-0.707106781186548));
#23518=DIRECTION('ref_axis',(0.923879532511289,0.270598050073094,-0.270598050073094));
#23519=DIRECTION('',(0.,0.707106781186548,0.707106781186548));
#23520=DIRECTION('center_axis',(0.,0.707106781186548,0.707106781186548));
#23521=DIRECTION('ref_axis',(0.92387953251129,0.270598050073092,-0.270598050073092));
#23522=DIRECTION('center_axis',(0.707106781186547,0.500000000000001,-0.500000000000001));
#23523=DIRECTION('ref_axis',(-0.577350269189627,0.,-0.816496580927725));
#23524=DIRECTION('',(-0.577350269189627,0.816496580927725,-1.99733352710025E-16));
#23525=DIRECTION('center_axis',(0.,-0.707106781186547,0.707106781186548));
#23526=DIRECTION('ref_axis',(0.38268343236509,0.653281482438193,0.653281482438183));
#23527=DIRECTION('',(0.,0.707106781186547,-0.707106781186548));
#23528=DIRECTION('',(0.,-0.707106781186547,0.707106781186548));
#23529=DIRECTION('center_axis',(-0.577350269189627,0.816496580927725,-1.92296268638356E-16));
#23530=DIRECTION('ref_axis',(0.816496580927726,0.577350269189626,0.));
#23531=DIRECTION('',(0.577350269189627,-0.816496580927725,1.99733352710025E-16));
#23532=DIRECTION('center_axis',(-0.577350269189624,0.816496580927727,-2.55393481785316E-15));
#23533=DIRECTION('ref_axis',(0.707106781186548,0.5,0.5));
#23534=DIRECTION('center_axis',(0.,0.,1.));
#23535=DIRECTION('ref_axis',(1.,0.,0.));
#23536=DIRECTION('center_axis',(0.,-0.707106781186547,0.707106781186548));
#23537=DIRECTION('ref_axis',(0.923879532511285,0.270598050073101,0.270598050073101));
#23538=DIRECTION('center_axis',(0.707106781186547,0.500000000000001,0.500000000000001));
#23539=DIRECTION('ref_axis',(0.577350269189627,0.,-0.816496580927725));
#23540=DIRECTION('',(0.,-0.707106781186547,0.707106781186548));
#23541=DIRECTION('center_axis',(0.,0.707106781186547,-0.707106781186548));
#23542=DIRECTION('ref_axis',(0.923879532511286,0.270598050073098,0.270598050073103));
#23543=DIRECTION('center_axis',(0.,-0.707106781186548,0.707106781186548));
#23544=DIRECTION('ref_axis',(1.,0.,0.));
#23545=DIRECTION('center_axis',(0.707106781186547,-0.500000000000001,-0.500000000000001));
#23546=DIRECTION('ref_axis',(-0.577350269189627,0.,-0.816496580927725));
#23547=DIRECTION('',(0.,-0.707106781186548,0.707106781186547));
#23548=DIRECTION('center_axis',(1.,0.,0.));
#23549=DIRECTION('ref_axis',(0.,-1.,0.));
#23550=DIRECTION('center_axis',(-0.707106781186547,0.5,0.5));
#23551=DIRECTION('ref_axis',(-0.707106781186548,-0.5,-0.5));
#23552=DIRECTION('center_axis',(-0.707106781186547,-0.500000000000001,0.500000000000001));
#23553=DIRECTION('ref_axis',(0.707106781186549,-0.499999999999999,0.499999999999999));
#23554=DIRECTION('',(1.,0.,0.));
#23555=DIRECTION('center_axis',(-1.,0.,0.));
#23556=DIRECTION('ref_axis',(0.,-0.707106781186548,-0.707106781186548));
#23557=DIRECTION('',(-1.,0.,0.));
#23558=DIRECTION('center_axis',(0.,0.,1.));
#23559=DIRECTION('ref_axis',(1.,0.,0.));
#23560=DIRECTION('center_axis',(0.,-0.707106781186548,0.707106781186547));
#23561=DIRECTION('ref_axis',(0.382683432365089,-0.653281482438189,-0.653281482438189));
#23562=DIRECTION('center_axis',(0.,-0.707106781186547,0.707106781186548));
#23563=DIRECTION('ref_axis',(0.,-0.707106781186548,-0.707106781186547));
#23564=DIRECTION('',(1.,0.,0.));
#23565=DIRECTION('center_axis',(0.,0.707106781186547,-0.707106781186548));
#23566=DIRECTION('ref_axis',(0.923879532511285,0.270598050073101,0.270598050073101));
#23567=DIRECTION('',(0.,-0.707106781186548,-0.707106781186547));
#23568=DIRECTION('center_axis',(0.,0.707106781186547,-0.707106781186548));
#23569=DIRECTION('ref_axis',(0.923879532511289,-0.270598050073094,-0.270598050073094));
#23570=DIRECTION('center_axis',(0.,0.707106781186548,-0.707106781186547));
#23571=DIRECTION('ref_axis',(0.38268343236509,-0.653281482438183,-0.653281482438193));
#23572=DIRECTION('',(0.,0.707106781186548,-0.707106781186547));
#23573=DIRECTION('center_axis',(0.,-0.707106781186548,0.707106781186548));
#23574=DIRECTION('ref_axis',(0.,-0.707106781186548,-0.707106781186548));
#23575=DIRECTION('center_axis',(-0.0824635143087527,-0.971269669085139,
0.223237538785696));
#23576=DIRECTION('ref_axis',(0.336556770590777,-0.237981574738982,-0.91109511592054));
#23577=DIRECTION('center_axis',(1.,0.,0.));
#23578=DIRECTION('ref_axis',(0.,0.,-1.));
#23579=DIRECTION('center_axis',(1.,0.,0.));
#23580=DIRECTION('ref_axis',(0.,0.,-1.));
#23581=DIRECTION('',(-1.,0.,0.));
#23582=DIRECTION('center_axis',(-1.,0.,0.));
#23583=DIRECTION('ref_axis',(0.,0.,-1.));
#23584=DIRECTION('',(1.,0.,0.));
#23585=DIRECTION('center_axis',(0.,-0.707106781186547,-0.707106781186548));
#23586=DIRECTION('ref_axis',(0.,0.707106781186548,-0.707106781186547));
#23587=DIRECTION('',(-7.85046229341888E-17,0.707106781186548,-0.707106781186547));
#23588=DIRECTION('',(1.,0.,0.));
#23589=DIRECTION('',(0.,-0.707106781186548,0.707106781186547));
#23590=DIRECTION('center_axis',(0.,0.,1.));
#23591=DIRECTION('ref_axis',(1.,0.,0.));
#23592=DIRECTION('center_axis',(0.,-0.707106781186547,-0.707106781186548));
#23593=DIRECTION('ref_axis',(0.382683432365089,-0.653281482438189,0.653281482438189));
#23594=DIRECTION('center_axis',(1.,0.,0.));
#23595=DIRECTION('ref_axis',(0.,-1.,0.));
#23596=DIRECTION('center_axis',(0.,-0.707106781186548,0.707106781186548));
#23597=DIRECTION('ref_axis',(0.,-0.707106781186548,-0.707106781186548));
#23598=DIRECTION('center_axis',(-0.577350269189626,-0.816496580927726,-3.20493781063927E-16));
#23599=DIRECTION('ref_axis',(0.816496580927727,-0.577350269189625,0.));
#23600=DIRECTION('center_axis',(-7.85046229341888E-17,0.707106781186548,
-0.707106781186547));
#23601=DIRECTION('ref_axis',(0.382683432365086,-0.653281482438194,-0.653281482438185));
#23602=DIRECTION('',(-7.85046229341888E-17,0.707106781186548,-0.707106781186547));
#23603=DIRECTION('center_axis',(1.,0.,0.));
#23604=DIRECTION('ref_axis',(0.,-1.,0.));
#23605=DIRECTION('',(-1.,0.,0.));
#23606=DIRECTION('center_axis',(-1.,0.,0.));
#23607=DIRECTION('ref_axis',(0.,-1.,0.));
#23608=DIRECTION('center_axis',(0.,-0.707106781186547,-0.707106781186548));
#23609=DIRECTION('ref_axis',(0.38268343236509,-0.653281482438193,0.653281482438183));
#23610=DIRECTION('',(-3.92523114670944E-17,0.707106781186547,0.707106781186548));
#23611=DIRECTION('center_axis',(0.,-0.707106781186548,-0.707106781186548));
#23612=DIRECTION('ref_axis',(0.707106781186548,-0.5,0.5));
#23613=DIRECTION('',(0.,-0.707106781186547,-0.707106781186548));
#23614=DIRECTION('center_axis',(-0.577350269189626,-0.816496580927726,-3.20493781063927E-16));
#23615=DIRECTION('ref_axis',(0.816496580927726,-0.577350269189626,0.));
#23616=DIRECTION('',(0.577350269189626,0.816496580927726,3.51392638260461E-16));
#23617=DIRECTION('center_axis',(-0.577350269189628,-0.816496580927725,0.));
#23618=DIRECTION('ref_axis',(0.707106781186546,-0.500000000000001,-0.500000000000001));
#23619=DIRECTION('',(-0.577350269189626,-0.816496580927726,-3.23637062644832E-16));
#23620=DIRECTION('center_axis',(0.,-0.707106781186548,0.707106781186547));
#23621=DIRECTION('ref_axis',(0.923879532511289,-0.270598050073094,-0.270598050073094));
#23622=DIRECTION('center_axis',(0.,0.707106781186548,-0.707106781186548));
#23623=DIRECTION('ref_axis',(1.,0.,0.));
#23624=DIRECTION('',(0.,0.707106781186548,-0.707106781186547));
#23625=DIRECTION('',(0.,-0.707106781186548,0.707106781186547));
#23626=DIRECTION('center_axis',(0.,0.,1.));
#23627=DIRECTION('ref_axis',(1.,0.,0.));
#23628=DIRECTION('center_axis',(0.,-0.707106781186547,-0.707106781186548));
#23629=DIRECTION('ref_axis',(0.92387953251129,-0.270598050073093,0.270598050073093));
#23630=DIRECTION('center_axis',(0.707106781186547,-0.5,0.5));
#23631=DIRECTION('ref_axis',(0.577350269189626,0.,-0.816496580927726));
#23632=DIRECTION('',(0.,-0.707106781186547,-0.707106781186548));
#23633=DIRECTION('',(0.577350269189623,-5.15565607263847E-15,-0.816496580927728));
#23634=DIRECTION('center_axis',(0.,0.707106781186547,0.707106781186548));
#23635=DIRECTION('ref_axis',(0.923879532511287,-0.270598050073094,0.270598050073103));
#23636=DIRECTION('',(0.,0.707106781186547,0.707106781186548));
#23637=DIRECTION('center_axis',(0.,0.707106781186547,0.707106781186548));
#23638=DIRECTION('ref_axis',(0.923879532511286,-0.270598050073101,0.270598050073101));
#23639=DIRECTION('center_axis',(1.,0.,0.));
#23640=DIRECTION('ref_axis',(0.,0.,-1.));
#23641=DIRECTION('',(0.,0.707106781186547,-0.707106781186548));
#23642=DIRECTION('center_axis',(0.,0.,1.));
#23643=DIRECTION('ref_axis',(1.,0.,0.));
#23644=DIRECTION('center_axis',(1.,0.,0.));
#23645=DIRECTION('ref_axis',(0.,1.,0.));
#23646=DIRECTION('',(-1.,0.,0.));
#23647=DIRECTION('center_axis',(-1.,0.,0.));
#23648=DIRECTION('ref_axis',(0.,1.,0.));
#23649=DIRECTION('',(1.,0.,0.));
#23650=DIRECTION('center_axis',(0.,0.707106781186548,0.707106781186547));
#23651=DIRECTION('ref_axis',(0.,-0.707106781186547,0.707106781186548));
#23652=DIRECTION('',(0.,0.707106781186547,-0.707106781186548));
#23653=DIRECTION('',(-1.,0.,0.));
#23654=DIRECTION('',(0.,-0.707106781186547,0.707106781186548));
#23655=DIRECTION('',(-1.,0.,0.));
#23656=DIRECTION('center_axis',(1.,0.,0.));
#23657=DIRECTION('ref_axis',(0.,0.,1.));
#23658=DIRECTION('center_axis',(-0.707106781186547,-0.500000000000001,0.500000000000001));
#23659=DIRECTION('ref_axis',(0.707106781186549,-0.499999999999999,0.499999999999999));
#23660=DIRECTION('center_axis',(-0.707106781186552,-0.499999999999997,-0.499999999999997));
#23661=DIRECTION('ref_axis',(-0.707106781186543,0.500000000000003,0.500000000000003));
#23662=DIRECTION('center_axis',(0.,0.707106781186547,-0.707106781186548));
#23663=DIRECTION('ref_axis',(0.923879532511285,0.270598050073101,0.270598050073101));
#23664=DIRECTION('center_axis',(0.,0.707106781186548,-0.707106781186548));
#23665=DIRECTION('ref_axis',(0.707106781186552,0.499999999999996,0.499999999999996));
#23666=DIRECTION('',(0.,0.707106781186547,-0.707106781186548));
#23667=DIRECTION('center_axis',(0.,0.,1.));
#23668=DIRECTION('ref_axis',(1.,0.,0.));
#23669=DIRECTION('center_axis',(0.577350269189624,-7.66180445355954E-15,
-0.816496580927727));
#23670=DIRECTION('ref_axis',(0.707106781186552,0.499999999999996,0.499999999999996));
#23671=DIRECTION('center_axis',(-0.577350269189623,5.12790049702284E-15,
0.816496580927728));
#23672=DIRECTION('ref_axis',(0.816496580927727,0.,0.577350269189624));
#23673=DIRECTION('center_axis',(-0.577350269189629,-7.26118722722956E-15,
0.816496580927724));
#23674=DIRECTION('ref_axis',(0.707106781186548,-0.5,0.5));
#23675=DIRECTION('',(-0.577350269189623,5.12790049702284E-15,0.816496580927728));
#23676=DIRECTION('center_axis',(0.,-0.707106781186548,0.707106781186547));
#23677=DIRECTION('ref_axis',(0.,-0.707106781186547,-0.707106781186548));
#23678=DIRECTION('',(1.,0.,0.));
#23679=DIRECTION('',(0.,0.707106781186547,0.707106781186548));
#23680=DIRECTION('center_axis',(0.707106781186547,-0.5,-0.5));
#23681=DIRECTION('ref_axis',(-0.577350269189626,0.,-0.816496580927726));
#23682=DIRECTION('center_axis',(0.,-0.707106781186547,0.707106781186548));
#23683=DIRECTION('ref_axis',(0.382683432365095,0.653281482438189,0.653281482438184));
#23684=DIRECTION('center_axis',(6.31716887673553E-15,0.707106781186543,
-0.707106781186552));
#23685=DIRECTION('ref_axis',(0.,0.707106781186552,0.707106781186543));
#23686=DIRECTION('',(7.85046229341892E-17,0.707106781186547,-0.707106781186548));
#23687=DIRECTION('center_axis',(0.0824635143087527,-0.971269669085139,0.223237538785696));
#23688=DIRECTION('ref_axis',(0.336556770590777,0.23798157473898,0.91109511592054));
#23689=DIRECTION('center_axis',(1.,0.,0.));
#23690=DIRECTION('ref_axis',(0.,0.,1.));
#23691=DIRECTION('center_axis',(1.,0.,0.));
#23692=DIRECTION('ref_axis',(0.,0.,1.));
#23693=DIRECTION('center_axis',(-1.,0.,0.));
#23694=DIRECTION('ref_axis',(0.,0.,1.));
#23695=DIRECTION('center_axis',(0.707106781186552,0.499999999999997,0.499999999999997));
#23696=DIRECTION('ref_axis',(0.577350269189621,0.,-0.816496580927729));
#23697=DIRECTION('center_axis',(1.,0.,0.));
#23698=DIRECTION('ref_axis',(0.,0.,-1.));
#23699=DIRECTION('center_axis',(-1.,0.,0.));
#23700=DIRECTION('ref_axis',(0.,0.707106781186548,-0.707106781186548));
#23701=DIRECTION('',(-1.,0.,0.));
#23702=DIRECTION('center_axis',(-1.,0.,0.));
#23703=DIRECTION('ref_axis',(0.,0.,-1.));
#23704=DIRECTION('',(1.,0.,0.));
#23705=DIRECTION('center_axis',(0.,0.707106781186547,0.707106781186548));
#23706=DIRECTION('ref_axis',(0.382683432365089,0.653281482438191,-0.653281482438186));
#23707=DIRECTION('center_axis',(0.,0.707106781186548,0.707106781186548));
#23708=DIRECTION('ref_axis',(0.707106781186544,0.500000000000003,-0.500000000000003));
#23709=DIRECTION('',(0.,0.707106781186547,0.707106781186548));
#23710=DIRECTION('center_axis',(0.,-0.707106781186548,-0.707106781186548));
#23711=DIRECTION('ref_axis',(0.,0.707106781186548,-0.707106781186548));
#23712=DIRECTION('',(0.,-0.707106781186547,-0.707106781186548));
#23713=DIRECTION('center_axis',(0.,0.,1.));
#23714=DIRECTION('ref_axis',(1.,0.,0.));
#23715=DIRECTION('center_axis',(0.,-0.707106781186548,0.707106781186548));
#23716=DIRECTION('ref_axis',(0.382683432365089,0.653281482438189,0.653281482438189));
#23717=DIRECTION('center_axis',(-0.577350269189627,0.816496580927725,3.84592537276713E-16));
#23718=DIRECTION('ref_axis',(0.816496580927727,0.577350269189625,0.));
#23719=DIRECTION('center_axis',(1.,0.,0.));
#23720=DIRECTION('ref_axis',(0.,1.,0.));
#23721=DIRECTION('center_axis',(0.,-0.707106781186548,-0.707106781186548));
#23722=DIRECTION('ref_axis',(0.,0.707106781186548,-0.707106781186548));
#23723=DIRECTION('',(0.,0.707106781186547,-0.707106781186547));
#23724=DIRECTION('',(1.,0.,0.));
#23725=DIRECTION('',(0.,-0.707106781186548,0.707106781186548));
#23726=DIRECTION('center_axis',(0.707106781186547,0.500000000000001,-0.5));
#23727=DIRECTION('ref_axis',(-0.577350269189626,0.,-0.816496580927726));
#23728=DIRECTION('',(-0.577350269189627,0.816496580927725,3.43955554188792E-16));
#23729=DIRECTION('',(0.,0.707106781186547,0.707106781186548));
#23730=DIRECTION('',(0.577350269189627,-4.76446869105127E-16,0.816496580927725));
#23731=DIRECTION('center_axis',(-0.577350269189627,4.48691293489498E-16,
-0.816496580927725));
#23732=DIRECTION('ref_axis',(0.816496580927726,0.,-0.577350269189626));
#23733=DIRECTION('center_axis',(0.577350269189626,2.55393481785319E-15,
0.816496580927726));
#23734=DIRECTION('ref_axis',(0.707106781186548,-0.5,-0.5));
#23735=DIRECTION('center_axis',(-0.577350269189625,-3.8559408034254E-15,
-0.816496580927727));
#23736=DIRECTION('ref_axis',(0.707106781186547,0.5,-0.5));
#23737=DIRECTION('',(-0.577350269189627,4.20935717873869E-16,-0.816496580927725));
#23738=DIRECTION('center_axis',(1.,0.,0.));
#23739=DIRECTION('ref_axis',(0.,-1.,0.));
#23740=DIRECTION('center_axis',(0.,0.707106781186548,-0.707106781186548));
#23741=DIRECTION('ref_axis',(0.382683432365087,-0.653281482438189,-0.653281482438189));
#23742=DIRECTION('center_axis',(0.,-0.707106781186547,-0.707106781186548));
#23743=DIRECTION('ref_axis',(0.923879532511286,0.270598050073102,-0.270598050073097));
#23744=DIRECTION('center_axis',(0.,-0.707106781186548,-0.707106781186548));
#23745=DIRECTION('ref_axis',(0.707106781186548,0.5,-0.5));
#23746=DIRECTION('',(0.,-0.707106781186547,-0.707106781186548));
#23747=DIRECTION('center_axis',(0.,0.707106781186548,0.707106781186548));
#23748=DIRECTION('ref_axis',(1.,0.,0.));
#23749=DIRECTION('center_axis',(0.,0.,1.));
#23750=DIRECTION('ref_axis',(1.,0.,0.));
#23751=DIRECTION('center_axis',(0.,0.707106781186548,-0.707106781186548));
#23752=DIRECTION('ref_axis',(0.92387953251129,-0.270598050073092,-0.270598050073092));
#23753=DIRECTION('center_axis',(-0.577350269189627,0.816496580927725,3.84592537276713E-16));
#23754=DIRECTION('ref_axis',(0.816496580927726,0.577350269189626,0.));
#23755=DIRECTION('',(0.577350269189627,-0.816496580927725,-4.27222281035679E-16));
#23756=DIRECTION('center_axis',(-0.577350269189625,0.816496580927726,2.55393481785319E-15));
#23757=DIRECTION('ref_axis',(0.707106781186549,0.499999999999999,0.499999999999999));
#23758=DIRECTION('center_axis',(0.,0.,1.));
#23759=DIRECTION('ref_axis',(1.,0.,0.));
#23760=DIRECTION('center_axis',(0.,0.707106781186548,-0.707106781186548));
#23761=DIRECTION('ref_axis',(0.923879532511286,0.270598050073101,0.270598050073101));
#23762=DIRECTION('center_axis',(0.,0.707106781186548,-0.707106781186548));
#23763=DIRECTION('ref_axis',(0.382683432365087,-0.653281482438187,-0.653281482438192));
#23764=DIRECTION('',(0.,-0.707106781186547,0.707106781186547));
#23765=DIRECTION('center_axis',(3.12791857003411E-15,0.70710678118655,-0.707106781186545));
#23766=DIRECTION('ref_axis',(0.707106781186547,-0.5,-0.5));
#23767=DIRECTION('center_axis',(0.707106781186547,-0.500000000000001,-0.500000000000001));
#23768=DIRECTION('ref_axis',(-0.577350269189627,0.,-0.816496580927725));
#23769=DIRECTION('',(0.,0.707106781186548,-0.707106781186548));
#23770=DIRECTION('',(0.577350269189627,0.816496580927725,-4.1978519696401E-16));
#23771=DIRECTION('center_axis',(0.,-0.707106781186548,0.707106781186548));
#23772=DIRECTION('ref_axis',(0.923879532511289,-0.270598050073094,-0.270598050073094));
#23773=DIRECTION('',(0.,-0.707106781186548,0.707106781186548));
#23774=DIRECTION('center_axis',(0.,-0.707106781186548,0.707106781186548));
#23775=DIRECTION('ref_axis',(0.92387953251129,-0.270598050073092,-0.270598050073092));
#23776=DIRECTION('center_axis',(1.,0.,0.));
#23777=DIRECTION('ref_axis',(0.,0.,-1.));
#23778=DIRECTION('',(0.,0.707106781186548,-0.707106781186548));
#23779=DIRECTION('',(0.,0.707106781186548,0.707106781186547));
#23780=DIRECTION('center_axis',(0.,0.707106781186548,-0.707106781186548));
#23781=DIRECTION('ref_axis',(0.923879532511287,0.270598050073094,0.270598050073103));
#23782=DIRECTION('',(0.,-0.707106781186548,0.707106781186548));
#23783=DIRECTION('center_axis',(0.,-0.707106781186548,0.707106781186548));
#23784=DIRECTION('ref_axis',(0.923879532511288,0.270598050073101,0.270598050073092));
#23785=DIRECTION('center_axis',(0.707106781186547,0.500000000000001,0.500000000000001));
#23786=DIRECTION('ref_axis',(0.577350269189627,0.,-0.816496580927725));
#23787=DIRECTION('',(0.,0.707106781186547,-0.707106781186547));
#23788=DIRECTION('',(-0.577350269189627,4.4010368850797E-16,0.816496580927725));
#23789=DIRECTION('center_axis',(0.,-0.707106781186548,0.707106781186548));
#23790=DIRECTION('ref_axis',(0.38268343236509,0.653281482438188,0.653281482438188));
#23791=DIRECTION('',(0.,-0.707106781186547,0.707106781186547));
#23792=DIRECTION('center_axis',(0.,0.707106781186548,-0.707106781186548));
#23793=DIRECTION('ref_axis',(-2.22044604925029E-15,0.707106781186548,0.707106781186548));
#23794=DIRECTION('center_axis',(0.,0.707106781186547,0.707106781186548));
#23795=DIRECTION('ref_axis',(0.707106781186547,0.5,-0.5));
#23796=DIRECTION('center_axis',(0.,-0.707106781186548,-0.707106781186548));
#23797=DIRECTION('ref_axis',(0.,0.707106781186548,-0.707106781186548));
#23798=DIRECTION('',(0.,-0.707106781186547,-0.707106781186548));
#23799=DIRECTION('center_axis',(0.707106781186547,-0.5,-0.5));
#23800=DIRECTION('ref_axis',(0.707106781186548,0.499999999999999,0.500000000000001));
#23801=DIRECTION('',(0.,0.707106781186547,0.707106781186548));
#23802=DIRECTION('center_axis',(1.,0.,0.));
#23803=DIRECTION('ref_axis',(0.,1.,0.));
#23804=DIRECTION('',(1.,0.,0.));
#23805=DIRECTION('center_axis',(-1.,0.,0.));
#23806=DIRECTION('ref_axis',(0.,0.707106781186548,0.707106781186548));
#23807=DIRECTION('',(-1.,0.,0.));
#23808=DIRECTION('center_axis',(-1.,0.,0.));
#23809=DIRECTION('ref_axis',(0.,1.,0.));
#23810=DIRECTION('center_axis',(0.,0.,1.));
#23811=DIRECTION('ref_axis',(1.,0.,0.));
#23812=DIRECTION('center_axis',(0.,0.707106781186548,-0.707106781186548));
#23813=DIRECTION('ref_axis',(0.707106781186548,0.5,0.5));
#23814=DIRECTION('center_axis',(1.,0.,0.));
#23815=DIRECTION('ref_axis',(0.,0.,-1.));
#23816=DIRECTION('',(0.,0.707106781186548,-0.707106781186548));
#23817=DIRECTION('',(0.,0.707106781186548,0.707106781186547));
#23818=DIRECTION('',(0.,-0.707106781186548,0.707106781186548));
#23819=DIRECTION('center_axis',(0.,-0.707106781186548,0.707106781186548));
#23820=DIRECTION('ref_axis',(0.707106781186547,0.5,0.5));
#23821=DIRECTION('',(0.,-0.707106781186548,0.707106781186548));
#23822=DIRECTION('center_axis',(0.,0.707106781186548,-0.707106781186548));
#23823=DIRECTION('ref_axis',(0.,0.707106781186548,0.707106781186548));
#23824=DIRECTION('center_axis',(0.,0.707106781186548,0.707106781186548));
#23825=DIRECTION('ref_axis',(0.,-0.707106781186548,0.707106781186548));
#23826=DIRECTION('',(0.,0.707106781186548,-0.707106781186548));
#23827=DIRECTION('',(-1.,0.,0.));
#23828=DIRECTION('center_axis',(0.,-1.,0.));
#23829=DIRECTION('ref_axis',(0.577350269189629,0.,0.816496580927724));
#23830=DIRECTION('center_axis',(1.,0.,0.));
#23831=DIRECTION('ref_axis',(0.,0.,1.));
#23832=DIRECTION('center_axis',(0.,0.707106781186548,0.707106781186547));
#23833=DIRECTION('ref_axis',(0.707106781186548,-0.5,0.5));
#23834=DIRECTION('center_axis',(0.,0.707106781186548,-0.707106781186547));
#23835=DIRECTION('ref_axis',(0.,0.707106781186547,0.707106781186548));
#23836=DIRECTION('',(0.,-0.707106781186547,-0.707106781186548));
#23837=DIRECTION('',(-1.,0.,0.));
#23838=DIRECTION('center_axis',(1.,0.,0.));
#23839=DIRECTION('ref_axis',(0.,0.,1.));
#23840=DIRECTION('center_axis',(-1.,0.,0.));
#23841=DIRECTION('ref_axis',(0.,0.,1.));
#23842=DIRECTION('',(1.,0.,0.));
#23843=DIRECTION('center_axis',(0.,-0.707106781186548,-0.707106781186547));
#23844=DIRECTION('ref_axis',(0.707106781186547,-0.5,0.5));
#23845=DIRECTION('',(0.,-0.707106781186548,-0.707106781186547));
#23846=DIRECTION('center_axis',(0.707106781186547,-0.5,-0.5));
#23847=DIRECTION('ref_axis',(0.707106781186548,0.500000000000001,0.499999999999999));
#23848=DIRECTION('center_axis',(0.577350269189627,-3.84592537276713E-16,
-0.816496580927725));
#23849=DIRECTION('ref_axis',(0.816496580927726,0.,0.577350269189626));
#23850=DIRECTION('center_axis',(-0.577350269189625,3.85594080342536E-15,
0.816496580927727));
#23851=DIRECTION('ref_axis',(0.707106781186547,-0.5,0.5));
#23852=DIRECTION('center_axis',(-0.57735026918963,7.26118722722964E-15,
0.816496580927723));
#23853=DIRECTION('ref_axis',(0.707106781186547,-0.499999999999992,0.500000000000009));
#23854=DIRECTION('',(0.577350269189627,-3.56836961661084E-16,-0.816496580927725));
#23855=DIRECTION('center_axis',(0.,0.707106781186548,0.707106781186547));
#23856=DIRECTION('ref_axis',(0.923879532511287,-0.270598050073094,0.270598050073103));
#23857=DIRECTION('center_axis',(0.,0.707106781186548,0.707106781186548));
#23858=DIRECTION('ref_axis',(0.707106781186546,-0.500000000000001,0.500000000000001));
#23859=DIRECTION('center_axis',(0.,-0.707106781186548,-0.707106781186548));
#23860=DIRECTION('ref_axis',(1.,0.,0.));
#23861=DIRECTION('',(0.,-0.707106781186548,-0.707106781186547));
#23862=DIRECTION('center_axis',(0.,0.,1.));
#23863=DIRECTION('ref_axis',(1.,0.,0.));
#23864=DIRECTION('center_axis',(0.577350269189627,0.816496580927725,-1.25192883228098E-15));
#23865=DIRECTION('ref_axis',(0.707106781186547,-0.5,0.5));
#23866=DIRECTION('center_axis',(-0.577350269189627,-0.816496580927725,4.48691293489498E-16));
#23867=DIRECTION('ref_axis',(0.816496580927725,-0.577350269189628,0.));
#23868=DIRECTION('center_axis',(0.577350269189625,0.816496580927727,-1.25192883228096E-15));
#23869=DIRECTION('ref_axis',(0.707106781186541,-0.499999999999993,0.500000000000016));
#23870=DIRECTION('',(-0.577350269189627,-0.816496580927725,4.75296348195268E-16));
#23871=DIRECTION('center_axis',(0.,0.,1.));
#23872=DIRECTION('ref_axis',(1.,0.,0.));
#23873=DIRECTION('center_axis',(0.707106781186547,-0.5,0.500000000000001));
#23874=DIRECTION('ref_axis',(0.577350269189627,0.,-0.816496580927725));
#23875=DIRECTION('',(0.,0.707106781186548,0.707106781186547));
#23876=DIRECTION('center_axis',(0.,0.707106781186548,0.707106781186548));
#23877=DIRECTION('ref_axis',(0.,-0.707106781186548,0.707106781186548));
#23878=DIRECTION('',(1.,0.,0.));
#23879=DIRECTION('',(-1.,0.,0.));
#23880=DIRECTION('center_axis',(1.,0.,0.));
#23881=DIRECTION('ref_axis',(0.,1.,0.));
#23882=DIRECTION('center_axis',(1.,0.,0.));
#23883=DIRECTION('ref_axis',(0.,0.,1.));
#23884=DIRECTION('center_axis',(-1.,0.,0.));
#23885=DIRECTION('ref_axis',(0.,-0.707106781186548,0.707106781186548));
#23886=DIRECTION('',(1.,0.,0.));
#23887=DIRECTION('center_axis',(-0.0824635143087543,-0.971269669085137,
-0.223237538785703));
#23888=DIRECTION('ref_axis',(0.336556770590775,-0.237981574738988,0.911095115920539));
#23889=DIRECTION('center_axis',(0.,0.707106781186548,0.707106781186547));
#23890=DIRECTION('ref_axis',(0.382683432365091,-0.653281482438184,0.653281482438192));
#23891=DIRECTION('center_axis',(0.,-0.707106781186548,-0.707106781186547));
#23892=DIRECTION('ref_axis',(0.38268343236509,-0.653281482438183,0.653281482438193));
#23893=DIRECTION('',(0.,-0.707106781186548,-0.707106781186547));
#23894=DIRECTION('center_axis',(-8.89310181676358E-15,0.707106781186548,
0.707106781186548));
#23895=DIRECTION('ref_axis',(0.,-0.707106781186548,0.707106781186548));
#23896=DIRECTION('center_axis',(0.,-0.707106781186547,0.707106781186548));
#23897=DIRECTION('ref_axis',(0.,-0.707106781186548,-0.707106781186547));
#23898=DIRECTION('',(0.,0.707106781186548,0.707106781186547));
#23899=DIRECTION('',(-1.,0.,0.));
#23900=DIRECTION('center_axis',(0.,0.,1.));
#23901=DIRECTION('ref_axis',(1.,0.,0.));
#23902=DIRECTION('center_axis',(1.,0.,0.));
#23903=DIRECTION('ref_axis',(0.,-1.,0.));
#23904=DIRECTION('center_axis',(1.,0.,0.));
#23905=DIRECTION('ref_axis',(0.,-1.,0.));
#23906=DIRECTION('center_axis',(-1.,0.,0.));
#23907=DIRECTION('ref_axis',(0.,-1.,0.));
#23908=DIRECTION('center_axis',(0.,-0.707106781186547,0.707106781186548));
#23909=DIRECTION('ref_axis',(0.923879532511289,-0.270598050073094,-0.270598050073094));
#23910=DIRECTION('',(0.,0.707106781186547,-0.707106781186548));
#23911=DIRECTION('center_axis',(0.,-0.707106781186548,0.707106781186548));
#23912=DIRECTION('ref_axis',(0.707106781186548,-0.5,-0.5));
#23913=DIRECTION('',(0.,-0.707106781186547,0.707106781186548));
#23914=DIRECTION('center_axis',(0.,-0.707106781186547,0.707106781186548));
#23915=DIRECTION('ref_axis',(0.923879532511289,-0.270598050073094,-0.270598050073094));
#23916=DIRECTION('center_axis',(-0.577350269189626,-1.92296268638356E-16,
-0.816496580927726));
#23917=DIRECTION('ref_axis',(0.816496580927725,0.,-0.577350269189628));
#23918=DIRECTION('center_axis',(0.627963030199555,-0.769094500660425,0.118979333316691));
#23919=DIRECTION('ref_axis',(-0.325057583671868,-0.398112608509064,-0.857813451890046));
#23920=DIRECTION('',(0.577350269189626,1.64540693022727E-16,0.816496580927726));
#23921=DIRECTION('center_axis',(-0.577350269189631,2.10324043823204E-15,
-0.816496580927722));
#23922=DIRECTION('ref_axis',(0.707106781186544,0.500000000000003,-0.500000000000003));
#23923=DIRECTION('',(-0.577350269189626,-1.92296268638356E-16,-0.816496580927726));
#23924=DIRECTION('center_axis',(0.888073833977113,0.,0.459700843380987));
#23925=DIRECTION('ref_axis',(0.459700843380987,-8.83987568720673E-17,-0.888073833977113));
#23926=DIRECTION('center_axis',(0.,0.,1.));
#23927=DIRECTION('ref_axis',(1.,0.,0.));
#23928=DIRECTION('center_axis',(0.,-0.707106781186548,-0.707106781186548));
#23929=DIRECTION('ref_axis',(0.923879532511288,0.270598050073101,-0.270598050073092));
#23930=DIRECTION('center_axis',(1.,0.,0.));
#23931=DIRECTION('ref_axis',(0.,0.,-1.));
#23932=DIRECTION('',(0.,-0.707106781186548,-0.707106781186548));
#23933=DIRECTION('',(0.,0.707106781186547,-0.707106781186548));
#23934=DIRECTION('',(0.,0.707106781186548,0.707106781186547));
#23935=DIRECTION('center_axis',(0.,-0.707106781186548,-0.707106781186548));
#23936=DIRECTION('ref_axis',(0.923879532511287,0.270598050073094,-0.270598050073103));
#23937=DIRECTION('',(0.,0.707106781186548,0.707106781186548));
#23938=DIRECTION('center_axis',(-0.499999999999998,0.853553390593274,0.146446609406731));
#23939=DIRECTION('ref_axis',(0.500000000000003,0.146446609406722,0.853553390593273));
#23940=DIRECTION('center_axis',(0.,0.,1.));
#23941=DIRECTION('ref_axis',(0.,-1.,0.));
#23942=DIRECTION('center_axis',(0.707106781186547,0.5,-0.5));
#23943=DIRECTION('ref_axis',(-0.577350269189626,0.,-0.816496580927726));
#23944=DIRECTION('',(0.,-0.707106781186548,-0.707106781186548));
#23945=DIRECTION('',(-0.707106781186548,0.5,-0.5));
#23946=DIRECTION('center_axis',(0.,0.707106781186548,0.707106781186548));
#23947=DIRECTION('ref_axis',(0.382683432365088,0.653281482438189,-0.653281482438189));
#23948=DIRECTION('center_axis',(-0.707106781186547,-0.500000000000001,-0.500000000000001));
#23949=DIRECTION('ref_axis',(0.707106781186549,-0.499999999999999,-0.499999999999999));
#23950=DIRECTION('',(0.,0.707106781186548,0.707106781186548));
#23951=DIRECTION('center_axis',(0.,-0.707106781186548,-0.707106781186548));
#23952=DIRECTION('ref_axis',(0.,0.707106781186548,-0.707106781186548));
#23953=DIRECTION('center_axis',(1.,0.,0.));
#23954=DIRECTION('ref_axis',(0.,0.,-1.));
#23955=DIRECTION('center_axis',(-0.707106781186547,0.5,0.5));
#23956=DIRECTION('ref_axis',(-0.707106781186548,-0.5,-0.5));
#23957=DIRECTION('',(-1.,0.,0.));
#23958=DIRECTION('center_axis',(-1.,0.,0.));
#23959=DIRECTION('ref_axis',(0.,0.,-1.));
#23960=DIRECTION('',(1.,0.,0.));
#23961=DIRECTION('center_axis',(7.85046229341889E-17,-0.707106781186548,
-0.707106781186547));
#23962=DIRECTION('ref_axis',(0.382683432365091,-0.653281482438185,0.65328148243819));
#23963=DIRECTION('center_axis',(0.,-0.707106781186548,-0.707106781186548));
#23964=DIRECTION('ref_axis',(0.707106781186548,-0.5,0.5));
#23965=DIRECTION('',(7.85046229341889E-17,-0.707106781186548,-0.707106781186547));
#23966=DIRECTION('center_axis',(-1.77862036335272E-14,0.707106781186548,
0.707106781186548));
#23967=DIRECTION('ref_axis',(-2.22044604925032E-15,-0.707106781186548,0.707106781186548));
#23968=DIRECTION('',(-7.85046229341889E-17,0.707106781186548,0.707106781186547));
#23969=DIRECTION('center_axis',(0.,0.,1.));
#23970=DIRECTION('ref_axis',(1.,0.,0.));
#23971=DIRECTION('center_axis',(7.85046229341887E-17,0.707106781186547,
-0.707106781186548));
#23972=DIRECTION('ref_axis',(0.382683432365087,-0.653281482438189,-0.653281482438189));
#23973=DIRECTION('center_axis',(-0.577350269189626,-0.816496580927726,-1.02558009940457E-15));
#23974=DIRECTION('ref_axis',(0.816496580927725,-0.577350269189627,-8.88178419700125E-15));
#23975=DIRECTION('center_axis',(1.,0.,0.));
#23976=DIRECTION('ref_axis',(0.,-1.,0.));
#23977=DIRECTION('center_axis',(0.,-1.,0.));
#23978=DIRECTION('ref_axis',(0.505449465124417,0.,0.862856209461021));
#23979=DIRECTION('center_axis',(7.85046229341889E-17,-0.707106781186547,
0.707106781186548));
#23980=DIRECTION('ref_axis',(0.382683432365089,0.653281482438189,0.653281482438189));
#23981=DIRECTION('center_axis',(1.,0.,0.));
#23982=DIRECTION('ref_axis',(0.,0.,1.));
#23983=DIRECTION('center_axis',(-0.577350269189627,2.56395024851142E-16,
0.816496580927725));
#23984=DIRECTION('ref_axis',(0.816496580927725,0.,0.577350269189628));
#23985=DIRECTION('center_axis',(1.,0.,0.));
#23986=DIRECTION('ref_axis',(0.,0.,1.));
#23987=DIRECTION('',(-1.,0.,0.));
#23988=DIRECTION('center_axis',(-1.,0.,0.));
#23989=DIRECTION('ref_axis',(0.,0.,1.));
#23990=DIRECTION('',(1.,0.,0.));
#23991=DIRECTION('center_axis',(7.85046229341889E-17,-0.707106781186547,
0.707106781186548));
#23992=DIRECTION('ref_axis',(0.38268343236509,0.653281482438188,0.653281482438188));
#23993=DIRECTION('',(-7.85046229341889E-17,0.707106781186547,-0.707106781186548));
#23994=DIRECTION('center_axis',(-7.85046229341889E-17,0.707106781186547,
-0.707106781186548));
#23995=DIRECTION('ref_axis',(0.382683432365089,0.653281482438189,0.653281482438189));
#23996=DIRECTION('',(7.85046229341889E-17,-0.707106781186547,0.707106781186548));
#23997=DIRECTION('center_axis',(-0.577350269189627,2.56395024851142E-16,
0.816496580927725));
#23998=DIRECTION('ref_axis',(0.816496580927726,0.,0.577350269189626));
#23999=DIRECTION('',(0.577350269189627,-2.28639449235513E-16,-0.816496580927725));
#24000=DIRECTION('center_axis',(-0.577350269189627,-1.25192883228098E-15,
0.816496580927725));
#24001=DIRECTION('ref_axis',(0.707106781186547,-0.5,0.5));
#24002=DIRECTION('',(-0.577350269189627,3.119061760824E-16,0.816496580927725));
#24003=DIRECTION('center_axis',(0.707106781186547,-0.500000000000001,0.500000000000001));
#24004=DIRECTION('ref_axis',(0.577350269189627,0.,-0.816496580927725));
#24005=DIRECTION('',(-0.577350269189626,-0.816496580927726,-9.91229679478456E-16));
#24006=DIRECTION('',(0.,-0.707106781186548,-0.707106781186547));
#24007=DIRECTION('center_axis',(-0.577350269189626,-0.816496580927726,-1.02558009940457E-15));
#24008=DIRECTION('ref_axis',(0.816496580927728,-0.577350269189623,-1.02558009940457E-14));
#24009=DIRECTION('',(0.577350269189626,0.816496580927726,1.01898525509409E-15));
#24010=DIRECTION('center_axis',(-0.577350269189626,-0.816496580927726,4.65717525608515E-15));
#24011=DIRECTION('ref_axis',(0.707106781186545,-0.500000000000002,-0.500000000000002));
#24012=DIRECTION('center_axis',(0.,-0.707106781186547,0.707106781186548));
#24013=DIRECTION('ref_axis',(0.923879532511289,-0.270598050073097,-0.270598050073093));
#24014=DIRECTION('center_axis',(0.,-0.707106781186548,0.707106781186548));
#24015=DIRECTION('ref_axis',(0.707106781186549,-0.499999999999999,-0.499999999999999));
#24016=DIRECTION('',(0.,-0.707106781186547,0.707106781186548));
#24017=DIRECTION('center_axis',(0.,0.707106781186548,-0.707106781186548));
#24018=DIRECTION('ref_axis',(1.,0.,0.));
#24019=DIRECTION('',(-3.92523114670944E-17,0.707106781186547,-0.707106781186548));
#24020=DIRECTION('center_axis',(0.,0.,1.));
#24021=DIRECTION('ref_axis',(1.,0.,0.));
#24022=DIRECTION('center_axis',(0.577350269189626,1.30200598557221E-15,
0.816496580927726));
#24023=DIRECTION('ref_axis',(0.707106781186548,-0.5,-0.5));
#24024=DIRECTION('center_axis',(0.,-0.707106781186548,-0.707106781186547));
#24025=DIRECTION('ref_axis',(0.923879532511286,0.270598050073101,-0.270598050073101));
#24026=DIRECTION('center_axis',(0.,0.,1.));
#24027=DIRECTION('ref_axis',(1.,0.,0.));
#24028=DIRECTION('center_axis',(0.,-0.707106781186548,-0.707106781186547));
#24029=DIRECTION('ref_axis',(0.923879532511288,-0.270598050073101,0.270598050073092));
#24030=DIRECTION('center_axis',(0.577350269189626,1.73066641774521E-15,
0.816496580927726));
#24031=DIRECTION('ref_axis',(0.707106781186549,-0.499999999999999,-0.499999999999999));
#24032=DIRECTION('center_axis',(0.673887338679049,-0.262323811637645,0.690696802233777));
#24033=DIRECTION('ref_axis',(0.214186495298063,-0.825340061942894,-0.522434615415204));
#24034=DIRECTION('',(0.577350269189626,1.73066641774521E-15,0.816496580927726));
#24035=DIRECTION('',(-0.577350269189626,-1.73066641774521E-15,-0.816496580927726));
#24036=DIRECTION('center_axis',(0.627963030199553,0.769094500660428,0.118979333316688));
#24037=DIRECTION('ref_axis',(-0.32505758367187,0.398112608509061,-0.857813451890046));
#24038=DIRECTION('center_axis',(0.,0.707106781186548,0.707106781186547));
#24039=DIRECTION('ref_axis',(0.923879532511287,-0.270598050073094,0.270598050073103));
#24040=DIRECTION('',(0.,0.707106781186548,0.707106781186547));
#24041=DIRECTION('center_axis',(0.,-0.707106781186548,-0.707106781186548));
#24042=DIRECTION('ref_axis',(1.,0.,0.));
#24043=DIRECTION('center_axis',(1.,0.,0.));
#24044=DIRECTION('ref_axis',(0.,0.,-1.));
#24045=DIRECTION('',(0.,-0.707106781186548,-0.707106781186547));
#24046=DIRECTION('',(0.,0.707106781186547,-0.707106781186548));
#24047=DIRECTION('center_axis',(0.,-0.707106781186548,-0.707106781186547));
#24048=DIRECTION('ref_axis',(0.923879532511287,0.270598050073094,-0.270598050073103));
#24049=DIRECTION('',(0.,0.707106781186548,0.707106781186547));
#24050=DIRECTION('center_axis',(0.,0.707106781186548,0.707106781186547));
#24051=DIRECTION('ref_axis',(0.92387953251129,0.270598050073093,-0.270598050073093));
#24052=DIRECTION('center_axis',(0.707106781186546,0.5,-0.500000000000001));
#24053=DIRECTION('ref_axis',(-0.577350269189627,0.,-0.816496580927725));
#24054=DIRECTION('',(0.,-0.707106781186548,-0.707106781186547));
#24055=DIRECTION('',(-0.577350269189627,0.816496580927725,-2.75562995485243E-16));
#24056=DIRECTION('center_axis',(-0.707106781186549,0.499999999999999,-0.499999999999999));
#24057=DIRECTION('ref_axis',(0.707106781186548,0.5,-0.5));
#24058=DIRECTION('center_axis',(0.382683432365087,-0.653281482438189,0.653281482438189));
#24059=DIRECTION('ref_axis',(0.923879532511288,0.270598050073096,-0.270598050073097));
#24060=DIRECTION('center_axis',(-0.707106781186547,0.5,-0.5));
#24061=DIRECTION('ref_axis',(0.707106781186546,0.500000000000001,-0.500000000000001));
#24062=DIRECTION('center_axis',(7.85046229341887E-17,0.707106781186547,
-0.707106781186548));
#24063=DIRECTION('ref_axis',(0.382683432365088,-0.653281482438189,-0.653281482438189));
#24064=DIRECTION('',(7.85046229341887E-17,0.707106781186547,-0.707106781186548));
#24065=DIRECTION('',(-7.85046229341887E-17,-0.707106781186547,0.707106781186548));
#24066=DIRECTION('center_axis',(0.707106781186548,-0.5,-0.5));
#24067=DIRECTION('ref_axis',(-0.577350269189626,0.,-0.816496580927726));
#24068=DIRECTION('center_axis',(1.,0.,0.));
#24069=DIRECTION('ref_axis',(0.,-1.,0.));
#24070=DIRECTION('',(-1.,0.,0.));
#24071=DIRECTION('center_axis',(-1.,0.,0.));
#24072=DIRECTION('ref_axis',(0.,-1.,0.));
#24073=DIRECTION('',(1.,0.,0.));
#24074=DIRECTION('center_axis',(0.,-0.707106781186547,0.707106781186548));
#24075=DIRECTION('ref_axis',(0.,-0.707106781186548,-0.707106781186547));
#24076=DIRECTION('',(0.,0.707106781186548,0.707106781186547));
#24077=DIRECTION('center_axis',(1.,0.,0.));
#24078=DIRECTION('ref_axis',(0.,0.,-1.));
#24079=DIRECTION('center_axis',(-1.,0.,0.));
#24080=DIRECTION('ref_axis',(0.,0.707106781186548,-0.707106781186548));
#24081=DIRECTION('',(-1.,0.,0.));
#24082=DIRECTION('center_axis',(-0.707106781186547,0.5,0.5));
#24083=DIRECTION('ref_axis',(-0.707106781186548,-0.5,-0.5));
#24084=DIRECTION('',(1.,0.,0.));
#24085=DIRECTION('center_axis',(0.0824635143087527,-0.971269669085139,-0.223237538785696));
#24086=DIRECTION('ref_axis',(0.336556770590777,0.237981574738982,-0.91109511592054));
#24087=DIRECTION('center_axis',(0.,-0.707106781186548,-0.707106781186547));
#24088=DIRECTION('ref_axis',(0.382683432365093,0.653281482438187,-0.653281482438187));
#24089=DIRECTION('center_axis',(0.,0.707106781186548,0.707106781186547));
#24090=DIRECTION('ref_axis',(0.38268343236509,0.653281482438183,-0.653281482438193));
#24091=DIRECTION('',(0.,0.707106781186548,0.707106781186547));
#24092=DIRECTION('center_axis',(0.,0.707106781186548,0.707106781186547));
#24093=DIRECTION('ref_axis',(0.382683432365093,0.653281482438187,-0.653281482438187));
#24094=DIRECTION('center_axis',(0.,0.707106781186547,-0.707106781186548));
#24095=DIRECTION('ref_axis',(0.,0.707106781186548,0.707106781186547));
#24096=DIRECTION('center_axis',(0.,-0.707106781186547,0.707106781186548));
#24097=DIRECTION('ref_axis',(0.923879532511285,0.270598050073102,0.270598050073102));
#24098=DIRECTION('',(-1.,0.,0.));
#24099=DIRECTION('center_axis',(0.,-0.707106781186548,-0.707106781186547));
#24100=DIRECTION('ref_axis',(0.,0.707106781186547,-0.707106781186548));
#24101=DIRECTION('',(0.,-0.707106781186547,0.707106781186548));
#24102=DIRECTION('',(0.,0.707106781186547,-0.707106781186548));
#24103=DIRECTION('center_axis',(0.707106781186547,-0.5,-0.5));
#24104=DIRECTION('ref_axis',(-0.577350269189626,0.,-0.816496580927726));
#24105=DIRECTION('center_axis',(0.,-0.707106781186547,0.707106781186548));
#24106=DIRECTION('ref_axis',(0.38268343236509,0.653281482438193,0.653281482438183));
#24107=DIRECTION('center_axis',(0.382683432365087,-0.653281482438189,0.653281482438189));
#24108=DIRECTION('ref_axis',(0.923879532511288,0.270598050073096,-0.270598050073097));
#24109=DIRECTION('',(0.,-0.707106781186547,0.707106781186548));
#24110=DIRECTION('center_axis',(0.707106781186547,-0.500000000000001,0.500000000000001));
#24111=DIRECTION('ref_axis',(0.707106781186549,0.499999999999999,-0.499999999999999));
#24112=DIRECTION('',(0.,0.707106781186547,-0.707106781186548));
#24113=DIRECTION('center_axis',(0.,0.707106781186548,0.707106781186547));
#24114=DIRECTION('ref_axis',(0.,-0.707106781186547,0.707106781186548));
#24115=DIRECTION('',(1.,0.,0.));
#24116=DIRECTION('',(1.,0.,0.));
#24117=DIRECTION('',(0.,0.707106781186547,-0.707106781186548));
#24118=DIRECTION('center_axis',(-0.707106781186548,0.5,-0.5));
#24119=DIRECTION('ref_axis',(0.,0.707106781186548,0.707106781186548));
#24120=DIRECTION('center_axis',(-0.707106781186547,-0.5,-0.5));
#24121=DIRECTION('ref_axis',(-0.408248290463863,0.866025403784438,-0.288675134594813));
#24122=DIRECTION('center_axis',(-0.707106781186547,0.5,-0.5));
#24123=DIRECTION('ref_axis',(0.,0.707106781186548,0.707106781186548));
#24124=DIRECTION('center_axis',(0.,0.,1.));
#24125=DIRECTION('ref_axis',(1.,0.,0.));
#24126=DIRECTION('center_axis',(1.,0.,0.));
#24127=DIRECTION('ref_axis',(0.,1.,0.));
#24128=DIRECTION('center_axis',(0.,0.707106781186547,-0.707106781186548));
#24129=DIRECTION('ref_axis',(0.923879532511285,0.270598050073102,0.270598050073102));
#24130=DIRECTION('',(0.,-0.707106781186547,0.707106781186548));
#24131=DIRECTION('center_axis',(0.,0.,1.));
#24132=DIRECTION('ref_axis',(1.,0.,0.));
#24133=DIRECTION('center_axis',(0.,-0.707106781186547,0.707106781186548));
#24134=DIRECTION('ref_axis',(0.923879532511285,0.270598050073101,0.270598050073101));
#24135=DIRECTION('center_axis',(1.,0.,0.));
#24136=DIRECTION('ref_axis',(0.,1.,0.));
#24137=DIRECTION('',(-1.,0.,0.));
#24138=DIRECTION('center_axis',(-1.,0.,0.));
#24139=DIRECTION('ref_axis',(0.,1.,0.));
#24140=DIRECTION('center_axis',(0.707106781186547,0.5,0.5));
#24141=DIRECTION('ref_axis',(0.577350269189626,0.,-0.816496580927726));
#24142=DIRECTION('center_axis',(-0.707106781186547,-0.5,-0.5));
#24143=DIRECTION('ref_axis',(-0.707106781186548,0.5,0.5));
#24144=DIRECTION('center_axis',(-0.577350269189627,0.816496580927725,-2.56395024851142E-16));
#24145=DIRECTION('ref_axis',(0.816496580927726,0.577350269189626,0.));
#24146=DIRECTION('center_axis',(-0.577350269189625,0.816496580927726,-2.55393481785319E-15));
#24147=DIRECTION('ref_axis',(0.707106781186547,0.5,0.5));
#24148=DIRECTION('center_axis',(0.577350269189627,-0.816496580927725,1.25192883228098E-15));
#24149=DIRECTION('ref_axis',(0.707106781186547,0.5,-0.5));
#24150=DIRECTION('',(0.577350269189627,-0.816496580927725,2.47807419869614E-16));
#24151=DIRECTION('center_axis',(0.,0.,1.));
#24152=DIRECTION('ref_axis',(1.,0.,0.));
#24153=DIRECTION('center_axis',(1.,-1.9721522630525E-29,3.14018491736754E-15));
#24154=DIRECTION('ref_axis',(2.22044604925032E-15,0.707106781186548,-0.707106781186548));
#24155=DIRECTION('center_axis',(1.,0.,0.));
#24156=DIRECTION('ref_axis',(0.,1.,0.));
#24157=DIRECTION('center_axis',(0.,0.707106781186547,-0.707106781186548));
#24158=DIRECTION('ref_axis',(0.923879532511285,0.270598050073102,0.270598050073102));
#24159=DIRECTION('center_axis',(0.,-0.707106781186548,0.707106781186548));
#24160=DIRECTION('ref_axis',(1.,0.,0.));
#24161=DIRECTION('',(0.,-0.707106781186547,0.707106781186548));
#24162=DIRECTION('center_axis',(0.,0.,1.));
#24163=DIRECTION('ref_axis',(1.,0.,0.));
#24164=DIRECTION('center_axis',(0.707106781186547,0.500000000000001,0.500000000000001));
#24165=DIRECTION('ref_axis',(0.577350269189627,0.,-0.816496580927725));
#24166=DIRECTION('center_axis',(-1.,0.,0.));
#24167=DIRECTION('ref_axis',(0.,0.,1.));
#24168=DIRECTION('center_axis',(1.,0.,0.));
#24169=DIRECTION('ref_axis',(0.,1.,0.));
#24170=DIRECTION('center_axis',(0.,-1.,1.22464679914735E-16));
#24171=DIRECTION('ref_axis',(0.,-1.22464679914735E-16,-1.));
#24172=DIRECTION('center_axis',(-1.,0.,0.));
#24173=DIRECTION('ref_axis',(0.,1.,0.));
#24174=DIRECTION('center_axis',(1.,0.,0.));
#24175=DIRECTION('ref_axis',(0.,1.,0.));
#24176=DIRECTION('center_axis',(1.,0.,0.));
#24177=DIRECTION('ref_axis',(0.,1.,0.));
#24178=DIRECTION('',(-1.,0.,0.));
#24179=DIRECTION('center_axis',(-1.,0.,0.));
#24180=DIRECTION('ref_axis',(0.,-0.97051674265181,-0.241033715966295));
#24181=DIRECTION('',(-1.,0.,0.));
#24182=DIRECTION('center_axis',(1.,0.,0.));
#24183=DIRECTION('ref_axis',(0.,1.,0.));
#24184=DIRECTION('',(1.,0.,0.));
#24185=DIRECTION('center_axis',(-1.,0.,0.));
#24186=DIRECTION('ref_axis',(0.,0.241033715966294,-0.97051674265181));
#24187=DIRECTION('',(-1.,0.,0.));
#24188=DIRECTION('center_axis',(1.,0.,0.));
#24189=DIRECTION('ref_axis',(0.,1.,0.));
#24190=DIRECTION('',(1.,0.,0.));
#24191=DIRECTION('center_axis',(-1.,0.,0.));
#24192=DIRECTION('ref_axis',(0.,0.969995350913823,0.24312346494234));
#24193=DIRECTION('',(-1.,0.,0.));
#24194=DIRECTION('center_axis',(1.,0.,0.));
#24195=DIRECTION('ref_axis',(0.,1.,0.));
#24196=DIRECTION('',(1.,0.,0.));
#24197=DIRECTION('center_axis',(-1.,0.,0.));
#24198=DIRECTION('ref_axis',(0.,-0.241033715966295,0.97051674265181));
#24199=DIRECTION('',(-1.,0.,0.));
#24200=DIRECTION('center_axis',(1.,0.,0.));
#24201=DIRECTION('ref_axis',(0.,1.,0.));
#24202=DIRECTION('',(1.,0.,0.));
#24203=DIRECTION('center_axis',(-1.,0.,0.));
#24204=DIRECTION('ref_axis',(0.,-0.97051674265181,-0.241033715966295));
#24205=DIRECTION('center_axis',(-1.,0.,0.));
#24206=DIRECTION('ref_axis',(0.,0.,1.));
#24207=DIRECTION('center_axis',(1.,0.,0.));
#24208=DIRECTION('ref_axis',(0.,0.,-1.));
#24209=DIRECTION('center_axis',(0.,0.418358158739791,-0.908282142847613));
#24210=DIRECTION('ref_axis',(-0.707106781186555,0.642252462438189,0.295823891009622));
#24211=DIRECTION('',(0.,0.418358158739791,-0.908282142847613));
#24212=DIRECTION('center_axis',(0.,-0.418358158739791,0.908282142847613));
#24213=DIRECTION('ref_axis',(0.,0.908282142847613,0.418358158739791));
#24214=DIRECTION('',(0.,-0.418358158739791,0.908282142847613));
#24215=DIRECTION('center_axis',(1.,0.,0.));
#24216=DIRECTION('ref_axis',(0.,0.,-1.));
#24217=DIRECTION('center_axis',(0.,0.418358158739791,-0.908282142847613));
#24218=DIRECTION('ref_axis',(0.,-0.908282142847613,-0.418358158739791));
#24219=DIRECTION('center_axis',(-1.,0.,0.));
#24220=DIRECTION('ref_axis',(0.,0.418358158739791,-0.908282142847613));
#24221=DIRECTION('center_axis',(1.,0.,0.));
#24222=DIRECTION('ref_axis',(0.,0.418358158739791,-0.908282142847613));
#24223=DIRECTION('center_axis',(0.,-0.418358158739791,0.908282142847613));
#24224=DIRECTION('ref_axis',(-0.707106781186553,-0.642252462438188,-0.295823891009627));
#24225=DIRECTION('center_axis',(1.17829328657438E-14,0.418358158739788,
-0.908282142847614));
#24226=DIRECTION('ref_axis',(0.,-0.908282142847615,-0.418358158739788));
#24227=DIRECTION('',(0.,0.418358158739791,-0.908282142847613));
#24228=DIRECTION('',(0.,-0.418358158739791,0.908282142847613));
#24229=DIRECTION('center_axis',(0.,0.,1.));
#24230=DIRECTION('ref_axis',(-0.882931989457712,-0.469500907339108,0.));
#24231=DIRECTION('center_axis',(-0.362122741649372,0.389964366236962,-0.846637415335365));
#24232=DIRECTION('ref_axis',(0.,-0.908282142847613,-0.418358158739791));
#24233=DIRECTION('center_axis',(0.,-0.738355409626738,0.674411809708973));
#24234=DIRECTION('ref_axis',(0.,0.674411809708973,0.738355409626738));
#24235=DIRECTION('center_axis',(-0.115099770040445,-0.983149096918184,0.142020759628991));
#24236=DIRECTION('ref_axis',(-0.619019837529353,0.182805506560833,0.763804024286447));
#24237=DIRECTION('center_axis',(0.381760244687915,-0.386672292982237,0.839490115138756));
#24238=DIRECTION('ref_axis',(-0.70710678118655,0.462718383602925,0.534688411578082));
#24239=DIRECTION('center_axis',(-1.,0.,0.));
#24240=DIRECTION('ref_axis',(0.,-0.600825752699094,0.799380019073261));
#24241=DIRECTION('center_axis',(0.776895413605824,-9.19403442267706E-16,
0.629629666008707));
#24242=DIRECTION('ref_axis',(0.619019837529357,-0.182805506560832,-0.763804024286444));
#24243=DIRECTION('center_axis',(-1.,0.,0.));
#24244=DIRECTION('ref_axis',(0.,-0.600825752699094,0.799380019073261));
#24245=DIRECTION('center_axis',(0.,-0.756163603297457,0.654382613650612));
#24246=DIRECTION('ref_axis',(0.,0.654382613650612,0.756163603297457));
#24247=DIRECTION('center_axis',(-1.,0.,0.));
#24248=DIRECTION('ref_axis',(0.,0.,1.));
#24249=DIRECTION('center_axis',(1.,0.,0.));
#24250=DIRECTION('ref_axis',(0.,0.975243650528983,0.221133041635355));
#24251=DIRECTION('',(0.,0.908282142847613,0.41835815873979));
#24252=DIRECTION('center_axis',(-1.,0.,0.));
#24253=DIRECTION('ref_axis',(0.,-0.908282142847614,-0.418358158739789));
#24254=DIRECTION('',(0.,-0.908282142847613,-0.41835815873979));
#24255=DIRECTION('center_axis',(1.,0.,0.));
#24256=DIRECTION('ref_axis',(0.,0.19866967435672,-0.980066508197783));
#24257=DIRECTION('',(0.,0.41835815873979,-0.908282142847613));
#24258=DIRECTION('center_axis',(-1.,0.,0.));
#24259=DIRECTION('ref_axis',(0.,-0.41835815873979,0.908282142847613));
#24260=DIRECTION('',(0.,-0.41835815873979,0.908282142847613));
#24261=DIRECTION('center_axis',(1.,0.,0.));
#24262=DIRECTION('ref_axis',(0.,-0.980066508197783,-0.198669674356721));
#24263=DIRECTION('',(0.,-0.908282142847613,-0.418358158739791));
#24264=DIRECTION('center_axis',(-1.,0.,0.));
#24265=DIRECTION('ref_axis',(0.,0.908282142847613,0.418358158739791));
#24266=DIRECTION('',(0.,0.908282142847613,0.418358158739791));
#24267=DIRECTION('center_axis',(1.,0.,0.));
#24268=DIRECTION('ref_axis',(0.,-0.210810429782021,0.977526962643548));
#24269=DIRECTION('center_axis',(-1.,0.,0.));
#24270=DIRECTION('ref_axis',(0.,-1.,0.));
#24271=DIRECTION('center_axis',(1.,0.,0.));
#24272=DIRECTION('ref_axis',(0.,0.,-1.));
#24273=DIRECTION('center_axis',(-1.,0.,0.));
#24274=DIRECTION('ref_axis',(0.,0.975243650528983,0.221133041635355));
#24275=DIRECTION('center_axis',(-4.03739704015074E-15,0.416488486990263,
0.909140990278494));
#24276=DIRECTION('ref_axis',(-0.707106781186543,0.64285975928058,-0.294501833436945));
#24277=DIRECTION('center_axis',(1.,0.,0.));
#24278=DIRECTION('ref_axis',(0.,1.,0.));
#24279=DIRECTION('center_axis',(1.,0.,0.));
#24280=DIRECTION('ref_axis',(0.,0.969995350913823,0.24312346494234));
#24281=DIRECTION('center_axis',(1.,0.,0.));
#24282=DIRECTION('ref_axis',(0.,0.,-1.));
#24283=DIRECTION('center_axis',(-1.77862036335276E-15,0.404205740461642,
0.914668092467347));
#24284=DIRECTION('ref_axis',(0.,0.914668092467347,-0.404205740461642));
#24285=DIRECTION('center_axis',(1.,0.,0.));
#24286=DIRECTION('ref_axis',(0.,-0.600825752699096,0.79938001907326));
#24287=DIRECTION('',(1.,0.,0.));
#24288=DIRECTION('center_axis',(1.,0.,0.));
#24289=DIRECTION('ref_axis',(0.,-0.600825752699096,0.79938001907326));
#24290=DIRECTION('center_axis',(0.,0.908282142847613,0.418358158739791));
#24291=DIRECTION('ref_axis',(-0.707106781186555,-0.295823891009622,0.642252462438189));
#24292=DIRECTION('',(0.,0.908282142847613,0.418358158739791));
#24293=DIRECTION('center_axis',(0.,-0.908282142847613,-0.418358158739791));
#24294=DIRECTION('ref_axis',(0.,-0.418358158739791,0.908282142847613));
#24295=DIRECTION('center_axis',(1.,0.,0.));
#24296=DIRECTION('ref_axis',(0.,0.908282142847613,0.418358158739792));
#24297=DIRECTION('center_axis',(0.,0.908282142847616,0.418358158739784));
#24298=DIRECTION('ref_axis',(0.,0.418358158739784,-0.908282142847616));
#24299=DIRECTION('center_axis',(1.,0.,0.));
#24300=DIRECTION('ref_axis',(0.,0.908282142847613,0.418358158739791));
#24301=DIRECTION('center_axis',(0.,-0.908282142847613,-0.418358158739791));
#24302=DIRECTION('ref_axis',(-0.707106781186548,0.295823891009625,-0.642252462438195));
#24303=DIRECTION('',(0.,-0.908282142847613,-0.418358158739791));
#24304=DIRECTION('center_axis',(-0.707106781186546,0.642252462438197,0.295823891009625));
#24305=DIRECTION('ref_axis',(-0.707106781186549,-0.642252462438194,-0.295823891009623));
#24306=DIRECTION('center_axis',(1.,0.,0.));
#24307=DIRECTION('ref_axis',(0.,0.,-1.));
#24308=DIRECTION('center_axis',(-5.98998015374409E-15,-0.738355409626737,
0.674411809708974));
#24309=DIRECTION('ref_axis',(-1.,0.,-8.88178419700113E-15));
#24310=DIRECTION('center_axis',(-1.,0.,0.));
#24311=DIRECTION('ref_axis',(0.,-0.980066508197783,-0.198669674356721));
#24312=DIRECTION('center_axis',(1.,0.,0.));
#24313=DIRECTION('ref_axis',(0.,-0.216171072508796,0.976355502575981));
#24314=DIRECTION('center_axis',(-1.,0.,0.));
#24315=DIRECTION('ref_axis',(0.,-0.210810429782021,0.977526962643547));
#24316=DIRECTION('center_axis',(0.,-0.908282142847613,-0.418358158739791));
#24317=DIRECTION('ref_axis',(0.,0.418358158739791,-0.908282142847613));
#24318=DIRECTION('',(-1.,0.,0.));
#24319=DIRECTION('',(0.,0.418358158739791,-0.908282142847613));
#24320=DIRECTION('',(1.,0.,0.));
#24321=DIRECTION('center_axis',(1.,0.,0.));
#24322=DIRECTION('ref_axis',(0.,1.,0.));
#24323=DIRECTION('center_axis',(1.,0.,0.));
#24324=DIRECTION('ref_axis',(0.,-0.241033715966295,0.97051674265181));
#24325=DIRECTION('center_axis',(1.,0.,0.));
#24326=DIRECTION('ref_axis',(0.,-0.799380019073275,-0.600825752699076));
#24327=DIRECTION('',(1.,0.,0.));
#24328=DIRECTION('center_axis',(1.,0.,0.));
#24329=DIRECTION('ref_axis',(0.,-0.799380019073275,-0.600825752699076));
#24330=DIRECTION('center_axis',(-0.381760244555379,-0.386672293005136,0.83949011518848));
#24331=DIRECTION('ref_axis',(0.,0.908282142847615,0.418358158739788));
#24332=DIRECTION('center_axis',(0.362122741649375,0.389964366236962,-0.846637415335364));
#24333=DIRECTION('ref_axis',(-0.707106781186545,-0.476881163957516,-0.522096117072833));
#24334=DIRECTION('center_axis',(0.,0.,1.));
#24335=DIRECTION('ref_axis',(-0.882931989457715,0.469500907339103,0.));
#24336=DIRECTION('center_axis',(0.,0.41835815873979,-0.908282142847613));
#24337=DIRECTION('ref_axis',(-0.707106781186547,0.642252462438196,0.295823891009626));
#24338=DIRECTION('center_axis',(1.,0.,0.));
#24339=DIRECTION('ref_axis',(0.,0.600825752699123,-0.79938001907324));
#24340=DIRECTION('center_axis',(1.,0.,0.));
#24341=DIRECTION('ref_axis',(0.,-0.654382613650613,-0.756163603297456));
#24342=DIRECTION('center_axis',(1.,0.,0.));
#24343=DIRECTION('ref_axis',(0.,-0.654382613650613,-0.756163603297456));
#24344=DIRECTION('',(1.,0.,0.));
#24345=DIRECTION('center_axis',(1.,0.,0.));
#24346=DIRECTION('ref_axis',(0.,0.600825752699123,-0.79938001907324));
#24347=DIRECTION('center_axis',(0.115099770900997,-0.983149096632188,0.142020760911393));
#24348=DIRECTION('ref_axis',(-0.619019836769066,-0.18280550809895,-0.763804024534489));
#24349=DIRECTION('center_axis',(0.,0.756163603307808,-0.654382613638651));
#24350=DIRECTION('ref_axis',(0.,-0.654382613638651,-0.756163603307808));
#24351=DIRECTION('center_axis',(-0.776895414084112,1.7867651802561E-15,
0.62962966541855));
#24352=DIRECTION('ref_axis',(0.619019836769075,0.182805508098944,0.763804024534484));
#24353=DIRECTION('center_axis',(0.,0.418358158739791,-0.908282142847613));
#24354=DIRECTION('ref_axis',(0.,0.908282142847613,0.418358158739791));
#24355=DIRECTION('',(-1.,0.,0.));
#24356=DIRECTION('',(0.,0.908282142847613,0.418358158739791));
#24357=DIRECTION('',(1.,0.,0.));
#24358=DIRECTION('center_axis',(1.,0.,0.));
#24359=DIRECTION('ref_axis',(0.,-0.977546692794496,-0.210718920381021));
#24360=DIRECTION('center_axis',(1.,0.,0.));
#24361=DIRECTION('ref_axis',(0.,-0.97051674265181,-0.241033715966295));
#24362=DIRECTION('center_axis',(1.,0.,0.));
#24363=DIRECTION('ref_axis',(0.,0.,-1.));
#24364=DIRECTION('center_axis',(-1.,0.,0.));
#24365=DIRECTION('ref_axis',(0.,-0.712574909369129,0.701596036574878));
#24366=DIRECTION('center_axis',(0.,-0.418358158739791,0.908282142847613));
#24367=DIRECTION('ref_axis',(0.,-0.908282142847613,-0.418358158739791));
#24368=DIRECTION('',(1.,0.,0.));
#24369=DIRECTION('',(0.,-0.908282142847613,-0.418358158739791));
#24370=DIRECTION('center_axis',(1.,0.,0.));
#24371=DIRECTION('ref_axis',(0.,-0.218855045483687,0.975757382276113));
#24372=DIRECTION('center_axis',(-1.,0.,0.));
#24373=DIRECTION('ref_axis',(0.,0.701596036574878,0.712574909369129));
#24374=DIRECTION('center_axis',(0.,0.908282142847613,0.418358158739791));
#24375=DIRECTION('ref_axis',(0.,-0.418358158739791,0.908282142847613));
#24376=DIRECTION('',(1.,0.,0.));
#24377=DIRECTION('',(0.,-0.418358158739791,0.908282142847613));
#24378=DIRECTION('center_axis',(0.545880488382889,0.761016047468252,0.350526843335369));
#24379=DIRECTION('ref_axis',(0.,0.418358158739799,-0.90828214284761));
#24380=DIRECTION('center_axis',(-0.551814247024938,-0.757477375369894,-0.348896922576048));
#24381=DIRECTION('ref_axis',(-0.70710678118655,0.64676801069249,-0.285816620134091));
#24382=DIRECTION('center_axis',(0.,0.,1.));
#24383=DIRECTION('ref_axis',(1.,0.,0.));
#24384=DIRECTION('center_axis',(0.,0.908282142847613,0.41835815873979));
#24385=DIRECTION('ref_axis',(-0.707106781186551,0.295823891009619,-0.642252462438195));
#24386=DIRECTION('center_axis',(0.,0.,1.));
#24387=DIRECTION('ref_axis',(1.,0.,0.));
#24388=DIRECTION('center_axis',(-1.,0.,0.));
#24389=DIRECTION('ref_axis',(0.,0.712574909369127,-0.70159603657488));
#24390=DIRECTION('center_axis',(0.,-0.908282142847613,-0.41835815873979));
#24391=DIRECTION('ref_axis',(-0.707106781186552,0.295823891009633,-0.642252462438187));
#24392=DIRECTION('',(0.,-0.908282142847613,-0.41835815873979));
#24393=DIRECTION('center_axis',(0.,0.908282142847613,0.418358158739791));
#24394=DIRECTION('ref_axis',(0.,0.418358158739791,-0.908282142847613));
#24395=DIRECTION('center_axis',(0.,-0.41835815873979,0.908282142847613));
#24396=DIRECTION('ref_axis',(0.,-0.908282142847613,-0.41835815873979));
#24397=DIRECTION('',(-1.,0.,0.));
#24398=DIRECTION('',(0.,-0.908282142847613,-0.41835815873979));
#24399=DIRECTION('',(1.,0.,0.));
#24400=DIRECTION('center_axis',(-1.,0.,0.));
#24401=DIRECTION('ref_axis',(0.,0.712574909369129,-0.701596036574878));
#24402=DIRECTION('center_axis',(-1.,0.,0.));
#24403=DIRECTION('ref_axis',(0.,-0.701596036574868,-0.712574909369139));
#24404=DIRECTION('center_axis',(1.,0.,0.));
#24405=DIRECTION('ref_axis',(0.,-0.908282142847615,-0.418358158739787));
#24406=DIRECTION('',(-1.,0.,0.));
#24407=DIRECTION('center_axis',(0.545880488382904,0.35052684333534,-0.761016047468255));
#24408=DIRECTION('ref_axis',(-3.55271367880051E-14,-0.908282142847614,-0.41835815873979));
#24409=DIRECTION('center_axis',(-0.551814249371486,-0.348896917908686,0.757477375810264));
#24410=DIRECTION('ref_axis',(-0.70710678118654,-0.285816620074966,-0.646768010718629));
#24411=DIRECTION('center_axis',(0.,0.,1.));
#24412=DIRECTION('ref_axis',(1.,0.,0.));
#24413=DIRECTION('center_axis',(0.,0.41835815873979,-0.908282142847613));
#24414=DIRECTION('ref_axis',(-0.707106781186553,-0.642252462438192,-0.295823891009619));
#24415=DIRECTION('center_axis',(0.,-0.909140990278493,0.416488486990267));
#24416=DIRECTION('ref_axis',(0.,-0.416488486990267,-0.909140990278493));
#24417=DIRECTION('center_axis',(0.,0.,1.));
#24418=DIRECTION('ref_axis',(1.,0.,0.));
#24419=DIRECTION('center_axis',(0.,-0.914668092467346,0.404205740461645));
#24420=DIRECTION('ref_axis',(0.,-0.404205740461645,-0.914668092467346));
#24421=DIRECTION('center_axis',(1.,0.,0.));
#24422=DIRECTION('ref_axis',(0.,0.,-1.));
#24423=DIRECTION('center_axis',(1.,0.,0.));
#24424=DIRECTION('ref_axis',(0.,0.241033715966294,-0.97051674265181));
#24425=DIRECTION('center_axis',(7.50087139441506E-14,0.654382613650666,
0.75616360329741));
#24426=DIRECTION('ref_axis',(-0.707106781186547,0.534688411578089,-0.462718383602923));
#24427=DIRECTION('center_axis',(1.,0.,0.));
#24428=DIRECTION('ref_axis',(0.,1.,0.));
#24429=DIRECTION('center_axis',(-1.,0.,0.));
#24430=DIRECTION('ref_axis',(0.,0.19866967435672,-0.980066508197783));
#24431=DIRECTION('center_axis',(1.,0.,0.));
#24432=DIRECTION('ref_axis',(0.,0.,-1.));
#24433=DIRECTION('center_axis',(1.,0.,0.));
#24434=DIRECTION('ref_axis',(0.,-0.515822394929815,-0.856695545038533));
#24435=DIRECTION('center_axis',(1.,0.,0.));
#24436=DIRECTION('ref_axis',(0.,0.,-1.));
#24437=DIRECTION('',(0.,0.41835815873979,-0.908282142847613));
#24438=DIRECTION('center_axis',(1.,0.,0.));
#24439=DIRECTION('ref_axis',(0.,0.,-1.));
#24440=DIRECTION('',(0.,-0.41835815873979,0.908282142847613));
#24441=DIRECTION('center_axis',(-1.,0.,0.));
#24442=DIRECTION('ref_axis',(0.,0.,-1.));
#24443=DIRECTION('center_axis',(-0.785375350227634,-0.602017675855261,0.144084271218794));
#24444=DIRECTION('ref_axis',(-0.619019837529315,0.763804024286477,-0.182805506560837));
#24445=DIRECTION('center_axis',(0.381760244688023,0.839490115138715,0.386672292982221));
#24446=DIRECTION('ref_axis',(0.,-0.418358158739795,0.908282142847611));
#24447=DIRECTION('center_axis',(-1.,0.,0.));
#24448=DIRECTION('ref_axis',(0.,0.75616360329746,-0.654382613650609));
#24449=DIRECTION('center_axis',(0.36212274164936,0.846637415335364,0.389964366236975));
#24450=DIRECTION('ref_axis',(-0.707106781186551,0.522096117072829,-0.476881163957511));
#24451=DIRECTION('center_axis',(1.,0.,0.));
#24452=DIRECTION('ref_axis',(0.,0.79938001907329,0.600825752699055));
#24453=DIRECTION('',(1.,0.,0.));
#24454=DIRECTION('center_axis',(1.,0.,0.));
#24455=DIRECTION('ref_axis',(0.,0.79938001907329,0.600825752699055));
#24456=DIRECTION('center_axis',(1.,0.,0.));
#24457=DIRECTION('ref_axis',(0.,0.,-1.));
#24458=DIRECTION('center_axis',(0.,-0.674411809708971,-0.73835540962674));
#24459=DIRECTION('ref_axis',(-1.,0.,0.));
#24460=DIRECTION('center_axis',(0.,-0.41835815873979,0.908282142847613));
#24461=DIRECTION('ref_axis',(-0.707106781186555,-0.642252462438189,-0.295823891009622));
#24462=DIRECTION('',(0.,-0.41835815873979,0.908282142847613));
#24463=DIRECTION('center_axis',(0.,0.418358158739791,-0.908282142847613));
#24464=DIRECTION('ref_axis',(0.,-0.908282142847613,-0.418358158739791));
#24465=DIRECTION('center_axis',(1.,0.,0.));
#24466=DIRECTION('ref_axis',(0.,-0.418358158739791,0.908282142847613));
#24467=DIRECTION('center_axis',(0.,-0.418358158739791,0.908282142847613));
#24468=DIRECTION('ref_axis',(0.,0.908282142847613,0.418358158739791));
#24469=DIRECTION('center_axis',(1.,0.,0.));
#24470=DIRECTION('ref_axis',(0.,-0.418358158739791,0.908282142847613));
#24471=DIRECTION('center_axis',(0.,0.41835815873979,-0.908282142847613));
#24472=DIRECTION('ref_axis',(-0.707106781186546,0.642252462438194,0.295823891009631));
#24473=DIRECTION('',(0.,0.41835815873979,-0.908282142847613));
#24474=DIRECTION('center_axis',(0.,0.,1.));
#24475=DIRECTION('ref_axis',(-0.892745142068122,-0.450561994972688,0.));
#24476=DIRECTION('center_axis',(0.,0.908282142847613,0.41835815873979));
#24477=DIRECTION('ref_axis',(-0.707106781186553,-0.295823891009619,0.642252462438192));
#24478=DIRECTION('center_axis',(0.,0.908282142847613,0.41835815873979));
#24479=DIRECTION('ref_axis',(0.,-0.41835815873979,0.908282142847613));
#24480=DIRECTION('',(1.,0.,0.));
#24481=DIRECTION('center_axis',(0.,0.41835815873979,-0.908282142847613));
#24482=DIRECTION('ref_axis',(0.,0.908282142847613,0.41835815873979));
#24483=DIRECTION('',(0.,0.908282142847613,0.41835815873979));
#24484=DIRECTION('',(1.,0.,0.));
#24485=DIRECTION('',(0.,0.908282142847613,0.41835815873979));
#24486=DIRECTION('center_axis',(0.,0.908282142847613,0.41835815873979));
#24487=DIRECTION('ref_axis',(-0.707106781186552,-0.295823891009608,0.642252462438199));
#24488=DIRECTION('center_axis',(0.,-0.908282142847614,-0.418358158739788));
#24489=DIRECTION('ref_axis',(0.,-0.418358158739788,0.908282142847615));
#24490=DIRECTION('center_axis',(1.,0.,0.));
#24491=DIRECTION('ref_axis',(0.,0.,-1.));
#24492=DIRECTION('center_axis',(1.,0.,0.));
#24493=DIRECTION('ref_axis',(0.,-0.908282142847614,-0.418358158739789));
#24494=DIRECTION('center_axis',(1.,0.,0.));
#24495=DIRECTION('ref_axis',(0.,0.,-1.));
#24496=DIRECTION('center_axis',(1.,0.,0.));
#24497=DIRECTION('ref_axis',(0.,0.,-1.));
#24498=DIRECTION('center_axis',(1.,0.,0.));
#24499=DIRECTION('ref_axis',(0.,0.,-1.));
#24500=DIRECTION('center_axis',(0.,-1.,0.));
#24501=DIRECTION('ref_axis',(0.,0.,1.));
#24502=DIRECTION('center_axis',(1.,0.,0.));
#24503=DIRECTION('ref_axis',(0.,0.,-1.));
#24504=DIRECTION('center_axis',(1.,0.,0.));
#24505=DIRECTION('ref_axis',(0.,0.,-1.));
#24506=DIRECTION('',(1.,0.,0.));
#24507=DIRECTION('center_axis',(-1.,0.,0.));
#24508=DIRECTION('ref_axis',(0.,0.,-1.));
#24509=DIRECTION('center_axis',(-1.,0.,0.));
#24510=DIRECTION('ref_axis',(0.,0.,-1.));
#24511=DIRECTION('center_axis',(-7.105427357601E-15,-1.,1.4210854715202E-14));
#24512=DIRECTION('ref_axis',(0.577350269189629,-7.10542735760104E-15,-0.816496580927724));
#24513=DIRECTION('center_axis',(0.,-0.707106781186552,-0.707106781186543));
#24514=DIRECTION('ref_axis',(0.,0.707106781186543,-0.707106781186552));
#24515=DIRECTION('center_axis',(0.,0.707106781186548,-0.707106781186547));
#24516=DIRECTION('ref_axis',(0.707106781186548,-0.5,-0.5));
#24517=DIRECTION('center_axis',(1.,0.,0.));
#24518=DIRECTION('ref_axis',(0.,0.,-1.));
#24519=DIRECTION('center_axis',(0.,0.707106781186547,0.707106781186548));
#24520=DIRECTION('ref_axis',(0.707106781186547,0.5,-0.5));
#24521=DIRECTION('center_axis',(0.707106781186545,0.500000000000002,0.500000000000002));
#24522=DIRECTION('ref_axis',(0.70710678118655,-0.499999999999998,-0.499999999999999));
#24523=DIRECTION('',(0.,-0.707106781186547,-0.707106781186548));
#24524=DIRECTION('',(0.,0.707106781186547,0.707106781186548));
#24525=DIRECTION('center_axis',(0.,0.707106781186548,-0.707106781186547));
#24526=DIRECTION('ref_axis',(0.,0.707106781186547,0.707106781186548));
#24527=DIRECTION('',(1.,0.,0.));
#24528=DIRECTION('',(1.,0.,0.));
#24529=DIRECTION('',(0.,-0.707106781186547,-0.707106781186548));
#24530=DIRECTION('',(-1.,0.,0.));
#24531=DIRECTION('',(-1.57009245868378E-16,0.707106781186547,0.707106781186548));
#24532=DIRECTION('center_axis',(1.,0.,0.));
#24533=DIRECTION('ref_axis',(0.,0.,-1.));
#24534=DIRECTION('',(-1.,0.,0.));
#24535=DIRECTION('center_axis',(-1.,0.,0.));
#24536=DIRECTION('ref_axis',(0.,0.,-1.));
#24537=DIRECTION('center_axis',(0.,-0.707106781186547,-0.707106781186548));
#24538=DIRECTION('ref_axis',(0.923879532511287,0.270598050073103,-0.270598050073094));
#24539=DIRECTION('center_axis',(0.32505758367186,0.398112608509073,0.857813451890045));
#24540=DIRECTION('ref_axis',(0.627963030199558,-0.769094500660421,0.118979333316701));
#24541=DIRECTION('',(-3.92523114670943E-17,0.707106781186547,0.707106781186548));
#24542=DIRECTION('center_axis',(0.325057583671865,-0.857813451890045,-0.398112608509066));
#24543=DIRECTION('ref_axis',(0.627963030199555,-0.118979333316694,0.769094500660424));
#24544=DIRECTION('center_axis',(0.,0.,-1.));
#24545=DIRECTION('ref_axis',(-1.47196168001604E-16,1.,0.));
#24546=DIRECTION('',(0.,-0.707106781186547,-0.707106781186548));
#24547=DIRECTION('center_axis',(0.,1.,6.28036983473511E-15));
#24548=DIRECTION('ref_axis',(-1.47196168001605E-16,6.35971014366111E-15,
-1.));
#24549=DIRECTION('center_axis',(-0.577350269189628,0.816496580927725,-1.02558009940457E-15));
#24550=DIRECTION('ref_axis',(0.707106781186546,0.500000000000001,0.500000000000001));
#24551=DIRECTION('',(-0.577350269189628,0.816496580927725,-1.02558009940457E-15));
#24552=DIRECTION('center_axis',(-0.577350269189625,0.816496580927727,3.85594080342543E-15));
#24553=DIRECTION('ref_axis',(0.707106781186545,0.500000000000004,0.499999999999999));
#24554=DIRECTION('',(0.577350269189628,-0.816496580927725,1.02558009940457E-15));
#24555=DIRECTION('center_axis',(-0.325057583671864,0.857813451890046,-0.398112608509065));
#24556=DIRECTION('ref_axis',(0.627963030199557,-0.118979333316692,-0.769094500660423));
#24557=DIRECTION('center_axis',(0.707106781186546,0.500000000000001,-0.500000000000001));
#24558=DIRECTION('ref_axis',(-0.577350269189627,0.,-0.816496580927725));
#24559=DIRECTION('',(0.577350269189624,5.25609800944841E-15,0.816496580927727));
#24560=DIRECTION('',(1.57009245868378E-16,-0.707106781186547,-0.707106781186548));
#24561=DIRECTION('center_axis',(-0.577350269189624,-5.25609800944841E-15,
-0.816496580927727));
#24562=DIRECTION('ref_axis',(0.707106781186548,0.5,-0.5));
#24563=DIRECTION('center_axis',(-0.325057583671868,0.398112608509056,-0.857813451890049));
#24564=DIRECTION('ref_axis',(0.627963030199554,0.769094500660427,0.118979333316684));
#24565=DIRECTION('',(-0.577350269189624,-5.25609800944841E-15,-0.816496580927727));
#24566=DIRECTION('center_axis',(-0.577350269189631,9.81512204508276E-15,
-0.816496580927722));
#24567=DIRECTION('ref_axis',(0.707106781186547,0.5,-0.5));
#24568=DIRECTION('center_axis',(-1.57009245868378E-16,0.707106781186547,
0.707106781186548));
#24569=DIRECTION('ref_axis',(0.382683432365086,0.65328148243819,-0.65328148243819));
#24570=DIRECTION('center_axis',(0.,0.707106781186548,0.707106781186548));
#24571=DIRECTION('ref_axis',(0.707106781186546,0.500000000000001,-0.500000000000001));
#24572=DIRECTION('center_axis',(0.,-0.707106781186548,-0.707106781186548));
#24573=DIRECTION('ref_axis',(-2.22044604925032E-15,0.707106781186548,-0.707106781186548));
#24574=DIRECTION('center_axis',(0.707106781186545,0.500000000000001,0.500000000000002));
#24575=DIRECTION('ref_axis',(0.577350269189628,0.,-0.816496580927724));
#24576=DIRECTION('',(7.8504622934189E-17,0.707106781186548,-0.707106781186547));
#24577=DIRECTION('',(-0.577350269189628,-1.18153318744577E-15,0.816496580927725));
#24578=DIRECTION('',(-3.92523114670943E-17,-0.707106781186548,0.707106781186547));
#24579=DIRECTION('center_axis',(0.707106781186551,-0.499999999999998,-0.499999999999997));
#24580=DIRECTION('ref_axis',(-0.577350269189622,0.,-0.816496580927729));
#24581=DIRECTION('',(-3.92523114670946E-17,0.707106781186547,-0.707106781186548));
#24582=DIRECTION('center_axis',(-0.707106781186551,0.499999999999998,0.499999999999997));
#24583=DIRECTION('ref_axis',(-0.40824829046386,-0.86602540378444,0.288675134594813));
#24584=DIRECTION('',(7.85046229341884E-17,-0.707106781186547,0.707106781186548));
#24585=DIRECTION('center_axis',(0.,-0.707106781186547,0.707106781186548));
#24586=DIRECTION('ref_axis',(0.92387953251129,-0.270598050073093,-0.270598050073093));
#24587=DIRECTION('',(0.,-0.707106781186547,0.707106781186548));
#24588=DIRECTION('center_axis',(0.,-6.28036983473511E-15,-1.));
#24589=DIRECTION('ref_axis',(-4.90653893338677E-17,-1.,6.35971014366104E-15));
#24590=DIRECTION('center_axis',(1.,0.,0.));
#24591=DIRECTION('ref_axis',(0.,0.,-1.));
#24592=DIRECTION('center_axis',(1.,0.,0.));
#24593=DIRECTION('ref_axis',(0.,0.515822394929815,0.856695545038534));
#24594=DIRECTION('center_axis',(1.,0.,0.));
#24595=DIRECTION('ref_axis',(0.,0.,-1.));
#24596=DIRECTION('center_axis',(1.,0.,0.));
#24597=DIRECTION('ref_axis',(0.,0.,-1.));
#24598=DIRECTION('center_axis',(-1.,0.,0.));
#24599=DIRECTION('ref_axis',(0.,0.,-1.));
#24600=DIRECTION('center_axis',(1.,0.,0.));
#24601=DIRECTION('ref_axis',(0.,0.,-1.));
#24602=DIRECTION('center_axis',(0.,-1.,0.));
#24603=DIRECTION('ref_axis',(0.,0.,1.));
#24604=DIRECTION('center_axis',(1.,0.,0.));
#24605=DIRECTION('ref_axis',(0.,0.,-1.));
#24606=DIRECTION('center_axis',(1.,0.,0.));
#24607=DIRECTION('ref_axis',(0.,0.,-1.));
#24608=DIRECTION('',(1.,0.,0.));
#24609=DIRECTION('center_axis',(-1.,0.,0.));
#24610=DIRECTION('ref_axis',(0.,0.,-1.));
#24611=DIRECTION('center_axis',(-1.,0.,0.));
#24612=DIRECTION('ref_axis',(0.,0.,-1.));
#24613=DIRECTION('center_axis',(1.,0.,0.));
#24614=DIRECTION('ref_axis',(0.,1.,0.));
#24615=DIRECTION('center_axis',(-1.,0.,0.));
#24616=DIRECTION('ref_axis',(0.,0.707106781186545,0.70710678118655));
#24617=DIRECTION('center_axis',(-1.,0.,0.));
#24618=DIRECTION('ref_axis',(0.,1.,0.));
#24619=DIRECTION('',(1.,0.,0.));
#24620=DIRECTION('center_axis',(0.,0.,1.));
#24621=DIRECTION('ref_axis',(1.,0.,0.));
#24622=DIRECTION('center_axis',(7.8504622934189E-17,0.707106781186548,-0.707106781186547));
#24623=DIRECTION('ref_axis',(0.382683432365092,0.653281482438186,0.65328148243819));
#24624=DIRECTION('center_axis',(1.,0.,0.));
#24625=DIRECTION('ref_axis',(0.,0.,-1.));
#24626=DIRECTION('center_axis',(-1.,0.,0.));
#24627=DIRECTION('ref_axis',(0.,0.707106781186552,-0.707106781186543));
#24628=DIRECTION('',(-1.,0.,0.));
#24629=DIRECTION('center_axis',(-0.082463514308756,-0.971269669085137,0.223237538785703));
#24630=DIRECTION('ref_axis',(0.336556770590781,-0.237981574738988,-0.911095115920536));
#24631=DIRECTION('center_axis',(-7.85046229341884E-17,0.707106781186547,
-0.707106781186548));
#24632=DIRECTION('ref_axis',(0.382683432365094,-0.653281482438187,-0.653281482438187));
#24633=DIRECTION('center_axis',(-7.8504622934189E-17,-0.707106781186548,
0.707106781186547));
#24634=DIRECTION('ref_axis',(0.382683432365091,0.65328148243819,0.653281482438185));
#24635=DIRECTION('',(-7.8504622934189E-17,-0.707106781186548,0.707106781186547));
#24636=DIRECTION('center_axis',(-1.77862036335272E-14,0.707106781186548,
-0.707106781186548));
#24637=DIRECTION('ref_axis',(2.22044604925032E-15,0.707106781186548,0.707106781186548));
#24638=DIRECTION('center_axis',(-3.5527136788005E-15,-1.,-7.105427357601E-15));
#24639=DIRECTION('ref_axis',(0.50544946512442,-7.10542735760098E-15,0.862856209461019));
#24640=DIRECTION('center_axis',(0.,-0.707106781186548,-0.707106781186547));
#24641=DIRECTION('ref_axis',(0.382683432365087,-0.653281482438187,0.653281482438191));
#24642=DIRECTION('center_axis',(-0.577350269189628,-1.15377761183014E-15,
0.816496580927725));
#24643=DIRECTION('ref_axis',(0.816496580927725,0.,0.577350269189628));
#24644=DIRECTION('center_axis',(1.,0.,0.));
#24645=DIRECTION('ref_axis',(0.,0.,1.));
#24646=DIRECTION('center_axis',(1.,0.,0.));
#24647=DIRECTION('ref_axis',(0.,0.,1.));
#24648=DIRECTION('',(-1.,0.,0.));
#24649=DIRECTION('center_axis',(-1.,0.,0.));
#24650=DIRECTION('ref_axis',(0.,0.,1.));
#24651=DIRECTION('',(1.,0.,0.));
#24652=DIRECTION('center_axis',(0.,0.707106781186547,0.707106781186548));
#24653=DIRECTION('ref_axis',(0.,-0.707106781186548,0.707106781186547));
#24654=DIRECTION('',(0.,0.707106781186548,-0.707106781186547));
#24655=DIRECTION('center_axis',(0.,0.707106781186548,-0.707106781186547));
#24656=DIRECTION('ref_axis',(0.923879532511287,0.270598050073103,0.270598050073094));
#24657=DIRECTION('center_axis',(0.,0.707106781186548,-0.707106781186548));
#24658=DIRECTION('ref_axis',(0.707106781186546,0.500000000000001,0.500000000000001));
#24659=DIRECTION('',(0.,0.707106781186548,-0.707106781186547));
#24660=DIRECTION('center_axis',(-0.577350269189628,-1.15377761183014E-15,
0.816496580927725));
#24661=DIRECTION('ref_axis',(0.816496580927726,0.,0.577350269189625));
#24662=DIRECTION('',(0.577350269189628,1.12602203621451E-15,-0.816496580927725));
#24663=DIRECTION('center_axis',(-0.577350269189629,4.70725240937645E-15,
0.816496580927724));
#24664=DIRECTION('ref_axis',(0.707106781186546,-0.499999999999997,0.500000000000005));
#24665=DIRECTION('center_axis',(0.,0.,1.));
#24666=DIRECTION('ref_axis',(1.,0.,0.));
#24667=DIRECTION('center_axis',(0.,0.707106781186548,0.707106781186547));
#24668=DIRECTION('ref_axis',(0.923879532511286,-0.270598050073101,0.270598050073101));
#24669=DIRECTION('center_axis',(1.,0.,0.));
#24670=DIRECTION('ref_axis',(0.,0.,-1.));
#24671=DIRECTION('',(0.,0.707106781186548,0.707106781186547));
#24672=DIRECTION('center_axis',(0.,0.707106781186548,0.707106781186547));
#24673=DIRECTION('ref_axis',(0.923879532511286,-0.270598050073102,0.270598050073097));
#24674=DIRECTION('',(0.,-0.707106781186548,-0.707106781186547));
#24675=DIRECTION('center_axis',(0.499999999999999,0.853553390593275,0.146446609406727));
#24676=DIRECTION('ref_axis',(0.5,-0.146446609406725,-0.853553390593274));
#24677=DIRECTION('center_axis',(0.707106781186547,-0.500000000000001,0.500000000000001));
#24678=DIRECTION('ref_axis',(0.577350269189627,0.,-0.816496580927725));
#24679=DIRECTION('',(0.,0.707106781186548,0.707106781186547));
#24680=DIRECTION('',(-0.707106781186549,-0.499999999999999,0.5));
#24681=DIRECTION('center_axis',(1.,0.,0.));
#24682=DIRECTION('ref_axis',(0.,0.,-1.));
#24683=DIRECTION('center_axis',(-1.,0.,0.));
#24684=DIRECTION('ref_axis',(0.,1.,0.));
#24685=DIRECTION('center_axis',(0.,-1.,-1.22464679914735E-16));
#24686=DIRECTION('ref_axis',(0.,-1.22464679914735E-16,1.));
#24687=DIRECTION('center_axis',(1.,0.,0.));
#24688=DIRECTION('ref_axis',(0.,1.,0.));
#24689=DIRECTION('center_axis',(-1.,0.,0.));
#24690=DIRECTION('ref_axis',(0.,1.,0.));
#24691=DIRECTION('center_axis',(1.,0.,0.));
#24692=DIRECTION('ref_axis',(0.,1.,0.));
#24693=DIRECTION('center_axis',(1.,0.,0.));
#24694=DIRECTION('ref_axis',(0.,-1.,1.83697019872103E-16));
#24695=DIRECTION('',(-1.,0.,0.));
#24696=DIRECTION('center_axis',(1.,0.,0.));
#24697=DIRECTION('ref_axis',(0.,-1.,1.83697019872103E-16));
#24698=DIRECTION('center_axis',(1.,0.,0.));
#24699=DIRECTION('ref_axis',(0.,0.,-1.));
#24700=DIRECTION('center_axis',(1.,0.,0.));
#24701=DIRECTION('ref_axis',(0.,0.,-1.));
#24702=DIRECTION('center_axis',(1.,0.,0.));
#24703=DIRECTION('ref_axis',(0.,0.,-1.));
#24704=DIRECTION('center_axis',(-1.,0.,0.));
#24705=DIRECTION('ref_axis',(0.,-1.,3.06161699786838E-17));
#24706=DIRECTION('center_axis',(-1.,0.,0.));
#24707=DIRECTION('ref_axis',(0.,-1.,3.06161699786838E-17));
#24708=DIRECTION('center_axis',(0.,-1.,-1.22464679914735E-16));
#24709=DIRECTION('ref_axis',(0.,-1.22464679914735E-16,1.));
#24710=DIRECTION('center_axis',(-1.,0.,0.));
#24711=DIRECTION('ref_axis',(0.,1.,0.));
#24712=DIRECTION('center_axis',(1.,0.,0.));
#24713=DIRECTION('ref_axis',(0.,-1.,3.06161699786838E-17));
#24714=DIRECTION('',(-0.707106781186544,-0.707106781186551,-8.65956056235498E-17));
#24715=DIRECTION('center_axis',(1.,0.,0.));
#24716=DIRECTION('ref_axis',(0.,-1.,3.06161699786838E-17));
#24717=DIRECTION('center_axis',(1.,0.,0.));
#24718=DIRECTION('ref_axis',(0.,0.,-1.));
#24719=DIRECTION('center_axis',(1.,0.,0.));
#24720=DIRECTION('ref_axis',(0.,-0.856695545038534,0.515822394929815));
#24721=DIRECTION('center_axis',(1.,0.,0.));
#24722=DIRECTION('ref_axis',(0.,0.,-1.));
#24723=DIRECTION('center_axis',(1.,0.,0.));
#24724=DIRECTION('ref_axis',(0.,0.,-1.));
#24725=DIRECTION('center_axis',(-1.,0.,0.));
#24726=DIRECTION('ref_axis',(0.,0.,-1.));
#24727=DIRECTION('center_axis',(1.,0.,0.));
#24728=DIRECTION('ref_axis',(0.,0.,-1.));
#24729=DIRECTION('center_axis',(1.,0.,0.));
#24730=DIRECTION('ref_axis',(0.,0.856695545038533,-0.515822394929815));
#24731=DIRECTION('center_axis',(1.,0.,0.));
#24732=DIRECTION('ref_axis',(0.,0.,-1.));
#24733=DIRECTION('center_axis',(-1.,0.,0.));
#24734=DIRECTION('ref_axis',(0.,0.,-1.));
#24735=DIRECTION('center_axis',(-0.707106781186549,-0.499999999999999,0.5));
#24736=DIRECTION('ref_axis',(0.,-0.70710678118655,-0.707106781186545));
#24737=DIRECTION('center_axis',(-0.707106781186548,-0.5,0.5));
#24738=DIRECTION('ref_axis',(0.,-0.707106781186548,-0.707106781186548));
#24739=DIRECTION('center_axis',(0.382683432365078,0.653281482438192,-0.653281482438192));
#24740=DIRECTION('ref_axis',(0.923879532511292,-0.270598050073089,0.270598050073091));
#24741=DIRECTION('center_axis',(-7.85046229341884E-17,0.707106781186547,
-0.707106781186548));
#24742=DIRECTION('ref_axis',(0.382683432365097,-0.653281482438186,-0.653281482438186));
#24743=DIRECTION('',(-7.85046229341884E-17,0.707106781186547,-0.707106781186548));
#24744=DIRECTION('center_axis',(0.,-0.707106781186548,-0.707106781186547));
#24745=DIRECTION('ref_axis',(0.,0.707106781186547,-0.707106781186548));
#24746=DIRECTION('',(1.,0.,0.));
#24747=DIRECTION('',(0.,0.707106781186547,-0.707106781186548));
#24748=DIRECTION('center_axis',(0.,-0.707106781186548,-0.707106781186547));
#24749=DIRECTION('ref_axis',(0.382683432365089,-0.653281482438186,0.653281482438191));
#24750=DIRECTION('',(0.,-0.707106781186548,-0.707106781186547));
#24751=DIRECTION('center_axis',(0.,0.707106781186548,0.707106781186548));
#24752=DIRECTION('ref_axis',(0.,-0.707106781186548,0.707106781186548));
#24753=DIRECTION('center_axis',(0.,0.,1.));
#24754=DIRECTION('ref_axis',(1.,0.,0.));
#24755=DIRECTION('center_axis',(1.,0.,0.));
#24756=DIRECTION('ref_axis',(0.,-1.,0.));
#24757=DIRECTION('center_axis',(0.,-0.707106781186547,0.707106781186548));
#24758=DIRECTION('ref_axis',(0.,-0.707106781186548,-0.707106781186547));
#24759=DIRECTION('',(0.,0.707106781186548,0.707106781186547));
#24760=DIRECTION('',(-1.,0.,0.));
#24761=DIRECTION('',(0.,-0.707106781186548,-0.707106781186547));
#24762=DIRECTION('',(-1.,0.,0.));
#24763=DIRECTION('center_axis',(1.,0.,0.));
#24764=DIRECTION('ref_axis',(0.,-1.,0.));
#24765=DIRECTION('center_axis',(-0.707106781186547,-0.500000000000001,-0.500000000000001));
#24766=DIRECTION('ref_axis',(0.707106781186549,-0.499999999999999,-0.499999999999999));
#24767=DIRECTION('center_axis',(1.,0.,0.));
#24768=DIRECTION('ref_axis',(0.,0.,-1.));
#24769=DIRECTION('center_axis',(0.,-1.,0.));
#24770=DIRECTION('ref_axis',(0.,0.,1.));
#24771=DIRECTION('center_axis',(1.,0.,0.));
#24772=DIRECTION('ref_axis',(0.,0.,-1.));
#24773=DIRECTION('center_axis',(1.,0.,0.));
#24774=DIRECTION('ref_axis',(0.,0.,-1.));
#24775=DIRECTION('',(1.,0.,0.));
#24776=DIRECTION('center_axis',(-1.,0.,0.));
#24777=DIRECTION('ref_axis',(0.,0.,-1.));
#24778=DIRECTION('center_axis',(-1.,0.,0.));
#24779=DIRECTION('ref_axis',(0.,0.,-1.));
#24780=DIRECTION('center_axis',(1.,0.,0.));
#24781=DIRECTION('ref_axis',(0.,0.,-1.));
#24782=DIRECTION('center_axis',(0.,-1.,0.));
#24783=DIRECTION('ref_axis',(0.,0.,1.));
#24784=DIRECTION('center_axis',(1.,0.,0.));
#24785=DIRECTION('ref_axis',(0.,0.,-1.));
#24786=DIRECTION('center_axis',(1.,0.,0.));
#24787=DIRECTION('ref_axis',(0.,0.,-1.));
#24788=DIRECTION('',(1.,0.,0.));
#24789=DIRECTION('center_axis',(-1.,0.,0.));
#24790=DIRECTION('ref_axis',(0.,0.,-1.));
#24791=DIRECTION('center_axis',(-1.,0.,0.));
#24792=DIRECTION('ref_axis',(0.,0.,-1.));
#24793=DIRECTION('center_axis',(-1.,0.,0.));
#24794=DIRECTION('ref_axis',(0.,0.,1.));
#24795=DIRECTION('center_axis',(1.,0.,0.));
#24796=DIRECTION('ref_axis',(0.,0.,-1.));
#24797=DIRECTION('center_axis',(0.,-1.,0.));
#24798=DIRECTION('ref_axis',(0.,0.,-1.));
#24799=DIRECTION('center_axis',(-1.,0.,0.));
#24800=DIRECTION('ref_axis',(0.,0.,-1.));
#24801=DIRECTION('center_axis',(-1.,0.,0.));
#24802=DIRECTION('ref_axis',(0.,0.,-1.));
#24803=DIRECTION('center_axis',(1.,0.,0.));
#24804=DIRECTION('ref_axis',(0.,0.,-1.));
#24805=DIRECTION('center_axis',(-1.,0.,0.));
#24806=DIRECTION('ref_axis',(0.,-1.,1.83697019872103E-16));
#24807=DIRECTION('center_axis',(1.,0.,0.));
#24808=DIRECTION('ref_axis',(0.,0.,-1.));
#24809=DIRECTION('center_axis',(1.,0.,0.));
#24810=DIRECTION('ref_axis',(0.,0.,-1.));
#24811=DIRECTION('center_axis',(1.,0.,0.));
#24812=DIRECTION('ref_axis',(0.,0.,-1.));
#24813=DIRECTION('center_axis',(1.,0.,0.));
#24814=DIRECTION('ref_axis',(0.,0.,-1.));
#24815=DIRECTION('center_axis',(-1.,0.,0.));
#24816=DIRECTION('ref_axis',(0.,0.,-1.));
#24817=DIRECTION('center_axis',(-1.,0.,0.));
#24818=DIRECTION('ref_axis',(0.,0.,-1.));
#24819=DIRECTION('center_axis',(-1.,0.,0.));
#24820=DIRECTION('ref_axis',(0.,0.,-1.));
#24821=DIRECTION('center_axis',(1.,0.,0.));
#24822=DIRECTION('ref_axis',(0.,-1.,1.83697019872103E-16));
#24823=DIRECTION('center_axis',(1.,0.,0.));
#24824=DIRECTION('ref_axis',(0.,0.,-1.));
#24825=DIRECTION('center_axis',(1.,0.,0.));
#24826=DIRECTION('ref_axis',(0.,0.,-1.));
#24827=DIRECTION('center_axis',(1.,0.,0.));
#24828=DIRECTION('ref_axis',(0.,0.,-1.));
#24829=DIRECTION('center_axis',(1.,0.,0.));
#24830=DIRECTION('ref_axis',(0.,0.,-1.));
#24831=DIRECTION('',(1.,0.,0.));
#24832=DIRECTION('center_axis',(-1.,0.,0.));
#24833=DIRECTION('ref_axis',(0.,0.,1.));
#24834=DIRECTION('center_axis',(0.,-1.,0.));
#24835=DIRECTION('ref_axis',(0.,0.,-1.));
#24836=DIRECTION('center_axis',(-1.,0.,0.));
#24837=DIRECTION('ref_axis',(0.,0.,-1.));
#24838=DIRECTION('center_axis',(-1.,0.,0.));
#24839=DIRECTION('ref_axis',(0.,0.,-1.));
#24840=DIRECTION('center_axis',(1.,0.,0.));
#24841=DIRECTION('ref_axis',(0.,0.,-1.));
#24842=DIRECTION('center_axis',(1.,0.,0.));
#24843=DIRECTION('ref_axis',(0.,0.,-1.));
#24844=DIRECTION('',(1.,0.,0.));
#24845=DIRECTION('center_axis',(1.,0.,0.));
#24846=DIRECTION('ref_axis',(0.,0.,-1.));
#24847=DIRECTION('center_axis',(0.,-1.,-1.22464679914735E-16));
#24848=DIRECTION('ref_axis',(0.,-1.22464679914735E-16,1.));
#24849=DIRECTION('center_axis',(-1.,0.,0.));
#24850=DIRECTION('ref_axis',(0.,0.,1.));
#24851=DIRECTION('center_axis',(0.,-1.,0.));
#24852=DIRECTION('ref_axis',(0.,0.,-1.));
#24853=DIRECTION('center_axis',(-1.,0.,0.));
#24854=DIRECTION('ref_axis',(0.,0.,1.));
#24855=DIRECTION('center_axis',(0.,-1.,0.));
#24856=DIRECTION('ref_axis',(0.,0.,-1.));
#24857=DIRECTION('center_axis',(-1.,0.,0.));
#24858=DIRECTION('ref_axis',(0.,0.,1.));
#24859=DIRECTION('center_axis',(0.,-1.,0.));
#24860=DIRECTION('ref_axis',(0.,0.,-1.));
#24861=DIRECTION('center_axis',(-1.,0.,0.));
#24862=DIRECTION('ref_axis',(0.,0.,-1.));
#24863=DIRECTION('center_axis',(-1.,0.,0.));
#24864=DIRECTION('ref_axis',(0.,0.,-1.));
#24865=DIRECTION('center_axis',(1.,0.,0.));
#24866=DIRECTION('ref_axis',(0.,0.,-1.));
#24867=DIRECTION('center_axis',(1.,0.,0.));
#24868=DIRECTION('ref_axis',(0.,0.,-1.));
#24869=DIRECTION('',(1.,0.,0.));
#24870=DIRECTION('center_axis',(-1.,0.,0.));
#24871=DIRECTION('ref_axis',(0.,0.,1.));
#24872=DIRECTION('center_axis',(0.,-1.,0.));
#24873=DIRECTION('ref_axis',(0.,0.,-1.));
#24874=DIRECTION('center_axis',(-1.,0.,0.));
#24875=DIRECTION('ref_axis',(0.,0.,1.));
#24876=DIRECTION('center_axis',(0.,-1.,0.));
#24877=DIRECTION('ref_axis',(0.,0.,-1.));
#24878=DIRECTION('center_axis',(1.,0.,0.));
#24879=DIRECTION('ref_axis',(0.,0.,-1.));
#24880=DIRECTION('center_axis',(-1.,0.,0.));
#24881=DIRECTION('ref_axis',(0.,0.,-1.));
#24882=DIRECTION('center_axis',(0.,-1.,0.));
#24883=DIRECTION('ref_axis',(0.,0.,1.));
#24884=DIRECTION('center_axis',(1.,0.,0.));
#24885=DIRECTION('ref_axis',(0.,0.,-1.));
#24886=DIRECTION('center_axis',(1.,0.,0.));
#24887=DIRECTION('ref_axis',(0.,0.,-1.));
#24888=DIRECTION('center_axis',(1.,0.,0.));
#24889=DIRECTION('ref_axis',(0.,0.,-1.));
#24890=DIRECTION('',(1.,0.,0.));
#24891=DIRECTION('center_axis',(1.,0.,0.));
#24892=DIRECTION('ref_axis',(0.,0.,-1.));
#24893=DIRECTION('center_axis',(1.,0.,0.));
#24894=DIRECTION('ref_axis',(0.,0.,-1.));
#24895=DIRECTION('center_axis',(1.,0.,0.));
#24896=DIRECTION('ref_axis',(0.,0.,-1.));
#24897=DIRECTION('center_axis',(-1.,0.,0.));
#24898=DIRECTION('ref_axis',(0.,0.,-1.));
#24899=DIRECTION('center_axis',(0.,-1.,0.));
#24900=DIRECTION('ref_axis',(0.,0.,1.));
#24901=DIRECTION('center_axis',(1.,0.,0.));
#24902=DIRECTION('ref_axis',(0.,0.,-1.));
#24903=DIRECTION('center_axis',(1.,0.,0.));
#24904=DIRECTION('ref_axis',(0.,0.,-1.));
#24905=DIRECTION('center_axis',(1.,0.,0.));
#24906=DIRECTION('ref_axis',(0.,0.,-1.));
#24907=DIRECTION('',(1.,0.,0.));
#24908=DIRECTION('center_axis',(1.,0.,0.));
#24909=DIRECTION('ref_axis',(0.,0.,-1.));
#24910=DIRECTION('center_axis',(1.,0.,0.));
#24911=DIRECTION('ref_axis',(0.,0.,-1.));
#24912=DIRECTION('center_axis',(1.,0.,0.));
#24913=DIRECTION('ref_axis',(0.,0.,-1.));
#24914=DIRECTION('center_axis',(-1.,0.,0.));
#24915=DIRECTION('ref_axis',(0.,0.,-1.));
#24916=DIRECTION('center_axis',(0.,-1.,0.));
#24917=DIRECTION('ref_axis',(0.,0.,1.));
#24918=DIRECTION('center_axis',(1.,0.,0.));
#24919=DIRECTION('ref_axis',(0.,0.,-1.));
#24920=DIRECTION('center_axis',(1.,0.,0.));
#24921=DIRECTION('ref_axis',(0.,0.,-1.));
#24922=DIRECTION('center_axis',(1.,0.,0.));
#24923=DIRECTION('ref_axis',(0.,0.,-1.));
#24924=DIRECTION('',(1.,0.,0.));
#24925=DIRECTION('center_axis',(1.,0.,0.));
#24926=DIRECTION('ref_axis',(0.,0.,-1.));
#24927=DIRECTION('center_axis',(1.,0.,0.));
#24928=DIRECTION('ref_axis',(0.,0.,-1.));
#24929=DIRECTION('center_axis',(0.,0.707106781186548,-0.707106781186547));
#24930=DIRECTION('ref_axis',(0.707106781186547,-0.5,-0.5));
#24931=DIRECTION('',(0.,-0.707106781186548,0.707106781186547));
#24932=DIRECTION('center_axis',(0.,0.707106781186548,-0.707106781186548));
#24933=DIRECTION('ref_axis',(1.,0.,0.));
#24934=DIRECTION('',(0.,0.707106781186548,-0.707106781186547));
#24935=DIRECTION('center_axis',(0.,-0.707106781186548,-0.707106781186547));
#24936=DIRECTION('ref_axis',(0.707106781186547,-0.5,0.5));
#24937=DIRECTION('center_axis',(0.,0.707106781186548,0.707106781186548));
#24938=DIRECTION('ref_axis',(0.,-0.707106781186548,0.707106781186548));
#24939=DIRECTION('',(0.,0.707106781186548,0.707106781186547));
#24940=DIRECTION('center_axis',(0.,0.,1.));
#24941=DIRECTION('ref_axis',(1.,0.,0.));
#24942=DIRECTION('center_axis',(1.,0.,0.));
#24943=DIRECTION('ref_axis',(0.,-1.,0.));
#24944=DIRECTION('center_axis',(0.,-0.707106781186547,-0.707106781186548));
#24945=DIRECTION('ref_axis',(0.,0.707106781186548,-0.707106781186547));
#24946=DIRECTION('',(0.,0.707106781186548,-0.707106781186547));
#24947=DIRECTION('',(1.,0.,0.));
#24948=DIRECTION('',(0.,-0.707106781186548,0.707106781186547));
#24949=DIRECTION('center_axis',(1.,0.,0.));
#24950=DIRECTION('ref_axis',(0.,-1.,0.));
#24951=DIRECTION('center_axis',(-1.,0.,0.));
#24952=DIRECTION('ref_axis',(0.,-1.,0.));
#24953=DIRECTION('center_axis',(1.,0.,0.));
#24954=DIRECTION('ref_axis',(0.,0.,-1.));
#24955=DIRECTION('center_axis',(-1.,0.,0.));
#24956=DIRECTION('ref_axis',(0.,-1.,1.83697019872103E-16));
#24957=DIRECTION('center_axis',(-1.,0.,0.));
#24958=DIRECTION('ref_axis',(0.,-1.,1.83697019872103E-16));
#24959=DIRECTION('center_axis',(0.,-1.,-1.22464679914735E-16));
#24960=DIRECTION('ref_axis',(0.,-1.22464679914735E-16,1.));
#24961=DIRECTION('center_axis',(1.,0.,0.));
#24962=DIRECTION('ref_axis',(0.,-1.,3.06161699786838E-17));
#24963=DIRECTION('center_axis',(1.,0.,0.));
#24964=DIRECTION('ref_axis',(0.,-1.,3.06161699786838E-17));
#24965=DIRECTION('center_axis',(1.,0.,0.));
#24966=DIRECTION('ref_axis',(0.,1.,0.));
#24967=DIRECTION('',(-0.707106781186545,0.70710678118655,8.65956056235496E-17));
#24968=DIRECTION('center_axis',(-1.,0.,0.));
#24969=DIRECTION('ref_axis',(0.,-1.,3.06161699786838E-17));
#24970=DIRECTION('center_axis',(-1.,0.,0.));
#24971=DIRECTION('ref_axis',(0.,-1.,3.06161699786838E-17));
#24972=DIRECTION('center_axis',(1.,0.,0.));
#24973=DIRECTION('ref_axis',(0.,1.,0.));
#24974=DIRECTION('center_axis',(1.,0.,0.));
#24975=DIRECTION('ref_axis',(0.,-1.,1.83697019872103E-16));
#24976=DIRECTION('',(-1.,0.,0.));
#24977=DIRECTION('center_axis',(1.,0.,0.));
#24978=DIRECTION('ref_axis',(0.,-1.,1.83697019872103E-16));
#24979=DIRECTION('center_axis',(1.,0.,0.));
#24980=DIRECTION('ref_axis',(0.,0.,-1.));
#24981=DIRECTION('center_axis',(0.,-1.,-1.22464679914735E-16));
#24982=DIRECTION('ref_axis',(0.,-1.22464679914735E-16,1.));
#24983=DIRECTION('center_axis',(1.,0.,0.));
#24984=DIRECTION('ref_axis',(0.,-1.,1.83697019872103E-16));
#24985=DIRECTION('center_axis',(-1.,0.,0.));
#24986=DIRECTION('ref_axis',(0.,0.,1.));
#24987=DIRECTION('center_axis',(-1.,0.,0.));
#24988=DIRECTION('ref_axis',(0.,0.,-1.));
#24989=DIRECTION('center_axis',(-1.,0.,0.));
#24990=DIRECTION('ref_axis',(0.,0.,-1.));
#24991=DIRECTION('center_axis',(1.,0.,0.));
#24992=DIRECTION('ref_axis',(0.,0.,-1.));
#24993=DIRECTION('center_axis',(1.,0.,0.));
#24994=DIRECTION('ref_axis',(0.,0.,-1.));
#24995=DIRECTION('center_axis',(1.,0.,0.));
#24996=DIRECTION('ref_axis',(0.,0.,-1.));
#24997=DIRECTION('center_axis',(-1.,0.,0.));
#24998=DIRECTION('ref_axis',(0.,-1.,1.83697019872103E-16));
#24999=DIRECTION('center_axis',(-1.,0.,0.));
#25000=DIRECTION('ref_axis',(0.,0.,-1.));
#25001=DIRECTION('center_axis',(1.,0.,0.));
#25002=DIRECTION('ref_axis',(0.,0.,-1.));
#25003=DIRECTION('center_axis',(0.,-1.,0.));
#25004=DIRECTION('ref_axis',(0.,0.,1.));
#25005=DIRECTION('center_axis',(1.,0.,0.));
#25006=DIRECTION('ref_axis',(0.,0.,-1.));
#25007=DIRECTION('center_axis',(0.,-1.,0.));
#25008=DIRECTION('ref_axis',(0.,0.,1.));
#25009=DIRECTION('center_axis',(1.,0.,0.));
#25010=DIRECTION('ref_axis',(0.,0.,-1.));
#25011=DIRECTION('center_axis',(0.,-1.,0.));
#25012=DIRECTION('ref_axis',(0.,0.,1.));
#25013=DIRECTION('center_axis',(1.,0.,0.));
#25014=DIRECTION('ref_axis',(0.,0.,-1.));
#25015=DIRECTION('center_axis',(-1.,0.,0.));
#25016=DIRECTION('ref_axis',(0.,-1.,1.83697019872103E-16));
#25017=DIRECTION('center_axis',(-1.,0.,0.));
#25018=DIRECTION('ref_axis',(0.,-1.,1.83697019872103E-16));
#25019=DIRECTION('center_axis',(0.,-1.,-1.22464679914735E-16));
#25020=DIRECTION('ref_axis',(0.,-1.22464679914735E-16,1.));
#25021=DIRECTION('center_axis',(1.,0.,0.));
#25022=DIRECTION('ref_axis',(0.,1.,0.));
#25023=DIRECTION('',(-1.,0.,0.));
#25024=DIRECTION('center_axis',(1.,0.,0.));
#25025=DIRECTION('ref_axis',(0.,-1.,0.));
#25026=DIRECTION('center_axis',(1.,0.,0.));
#25027=DIRECTION('ref_axis',(0.,-1.,0.));
#25028=DIRECTION('center_axis',(-1.,0.,0.));
#25029=DIRECTION('ref_axis',(0.,0.,1.));
#25030=DIRECTION('center_axis',(1.,0.,0.));
#25031=DIRECTION('ref_axis',(0.,-1.,6.12323399573677E-17));
#25032=DIRECTION('center_axis',(0.,-1.,1.22464679914735E-16));
#25033=DIRECTION('ref_axis',(0.,-1.22464679914735E-16,-1.));
#25034=DIRECTION('center_axis',(1.,0.,0.));
#25035=DIRECTION('ref_axis',(0.,-1.,6.12323399573677E-17));
#25036=DIRECTION('center_axis',(-1.,0.,0.));
#25037=DIRECTION('ref_axis',(0.,-1.,0.));
#25038=DIRECTION('',(0.707106781186552,-0.707106781186543,8.65956056235488E-17));
#25039=DIRECTION('center_axis',(-1.,0.,0.));
#25040=DIRECTION('ref_axis',(0.,-1.,6.12323399573677E-17));
#25041=DIRECTION('center_axis',(-1.,0.,0.));
#25042=DIRECTION('ref_axis',(0.,-1.,6.12323399573677E-17));
#25043=DIRECTION('center_axis',(1.,0.,0.));
#25044=DIRECTION('ref_axis',(0.,0.,-1.));
#25045=DIRECTION('center_axis',(0.,-1.,-1.22464679914735E-16));
#25046=DIRECTION('ref_axis',(0.,-1.22464679914735E-16,1.));
#25047=DIRECTION('center_axis',(1.,0.,0.));
#25048=DIRECTION('ref_axis',(0.,0.,-1.));
#25049=DIRECTION('center_axis',(0.,-1.,-1.22464679914735E-16));
#25050=DIRECTION('ref_axis',(0.,-1.22464679914735E-16,1.));
#25051=DIRECTION('center_axis',(1.,0.,0.));
#25052=DIRECTION('ref_axis',(0.,-1.,1.83697019872103E-16));
#25053=DIRECTION('center_axis',(1.,0.,0.));
#25054=DIRECTION('ref_axis',(0.,-1.,1.83697019872103E-16));
#25055=DIRECTION('center_axis',(1.,0.,0.));
#25056=DIRECTION('ref_axis',(0.,1.,0.));
#25057=DIRECTION('center_axis',(-1.,0.,0.));
#25058=DIRECTION('ref_axis',(0.,-1.,0.));
#25059=DIRECTION('',(-1.,0.,0.));
#25060=DIRECTION('center_axis',(-1.,0.,0.));
#25061=DIRECTION('ref_axis',(0.,-1.,0.));
#25062=DIRECTION('center_axis',(1.,0.,0.));
#25063=DIRECTION('ref_axis',(0.,0.,-1.));
#25064=DIRECTION('center_axis',(-1.,0.,0.));
#25065=DIRECTION('ref_axis',(0.,-1.,3.06161699786838E-17));
#25066=DIRECTION('center_axis',(-1.,0.,0.));
#25067=DIRECTION('ref_axis',(0.,-1.,3.06161699786838E-17));
#25068=DIRECTION('center_axis',(0.,-1.,-1.22464679914735E-16));
#25069=DIRECTION('ref_axis',(0.,-1.22464679914735E-16,1.));
#25070=DIRECTION('center_axis',(-1.,0.,0.));
#25071=DIRECTION('ref_axis',(0.,1.,0.));
#25072=DIRECTION('center_axis',(1.,-3.60555815900857E-17,-3.60555815900857E-17));
#25073=DIRECTION('ref_axis',(-5.09902924839489E-17,-0.707106781186547,-0.707106781186548));
#25074=DIRECTION('',(-0.707106781186545,-0.70710678118655,-8.65956056235496E-17));
#25075=DIRECTION('center_axis',(1.,-3.60555815900857E-17,-3.60555815900857E-17));
#25076=DIRECTION('ref_axis',(-5.09902924839489E-17,-0.707106781186547,-0.707106781186548));
#25077=DIRECTION('center_axis',(1.,0.,0.));
#25078=DIRECTION('ref_axis',(0.,0.,-1.));
#25079=DIRECTION('center_axis',(1.,0.,0.));
#25080=DIRECTION('ref_axis',(0.,3.89573857868908E-14,1.));
#25081=DIRECTION('center_axis',(1.,0.,0.));
#25082=DIRECTION('ref_axis',(0.,0.,-1.));
#25083=DIRECTION('center_axis',(-1.,0.,0.));
#25084=DIRECTION('ref_axis',(0.,-0.707106781186547,0.707106781186548));
#25085=DIRECTION('center_axis',(1.,0.,0.));
#25086=DIRECTION('ref_axis',(0.,0.,-1.));
#25087=DIRECTION('center_axis',(-1.,0.,0.));
#25088=DIRECTION('ref_axis',(0.,0.707106781186547,0.707106781186547));
#25089=DIRECTION('center_axis',(1.,0.,0.));
#25090=DIRECTION('ref_axis',(0.,0.,-1.));
#25091=DIRECTION('center_axis',(-1.,0.,0.));
#25092=DIRECTION('ref_axis',(0.,0.707106781186547,-0.707106781186547));
#25093=DIRECTION('center_axis',(-1.,0.,0.));
#25094=DIRECTION('ref_axis',(0.,-0.707106781186547,-0.707106781186548));
#25095=DIRECTION('center_axis',(-1.,0.,0.));
#25096=DIRECTION('ref_axis',(0.,0.,1.));
#25097=DIRECTION('center_axis',(1.,0.,0.));
#25098=DIRECTION('ref_axis',(0.,0.,-1.));
#25099=DIRECTION('center_axis',(0.,-1.,0.));
#25100=DIRECTION('ref_axis',(0.,0.,-1.));
#25101=DIRECTION('center_axis',(-1.,0.,0.));
#25102=DIRECTION('ref_axis',(0.,0.,-1.));
#25103=DIRECTION('center_axis',(-1.,0.,0.));
#25104=DIRECTION('ref_axis',(0.,0.,-1.));
#25105=DIRECTION('center_axis',(1.,0.,0.));
#25106=DIRECTION('ref_axis',(0.,0.,-1.));
#25107=DIRECTION('',(0.,0.707106781186548,0.707106781186548));
#25108=DIRECTION('',(0.,-0.707106781186548,-0.707106781186548));
#25109=DIRECTION('center_axis',(1.,0.,0.));
#25110=DIRECTION('ref_axis',(0.,0.,-1.));
#25111=DIRECTION('center_axis',(1.,0.,0.));
#25112=DIRECTION('ref_axis',(0.,-1.,0.));
#25113=DIRECTION('center_axis',(1.,0.,0.));
#25114=DIRECTION('ref_axis',(0.,0.,-1.));
#25115=DIRECTION('center_axis',(1.,0.,0.));
#25116=DIRECTION('ref_axis',(0.,0.,-1.));
#25117=DIRECTION('',(1.,0.,0.));
#25118=DIRECTION('center_axis',(-1.,0.,0.));
#25119=DIRECTION('ref_axis',(0.,0.,1.));
#25120=DIRECTION('center_axis',(0.,-1.,0.));
#25121=DIRECTION('ref_axis',(0.,0.,-1.));
#25122=DIRECTION('center_axis',(-1.,0.,0.));
#25123=DIRECTION('ref_axis',(0.,0.,-1.));
#25124=DIRECTION('center_axis',(-1.,0.,0.));
#25125=DIRECTION('ref_axis',(0.,0.,-1.));
#25126=DIRECTION('center_axis',(1.,0.,0.));
#25127=DIRECTION('ref_axis',(0.,0.,-1.));
#25128=DIRECTION('',(1.,0.,0.));
#25129=DIRECTION('center_axis',(-1.,0.,0.));
#25130=DIRECTION('ref_axis',(0.,0.,1.));
#25131=DIRECTION('center_axis',(0.,-1.,0.));
#25132=DIRECTION('ref_axis',(0.,0.,-1.));
#25133=DIRECTION('center_axis',(-1.,0.,0.));
#25134=DIRECTION('ref_axis',(0.,0.,-1.));
#25135=DIRECTION('center_axis',(-1.,0.,0.));
#25136=DIRECTION('ref_axis',(0.,0.,-1.));
#25137=DIRECTION('center_axis',(1.,0.,0.));
#25138=DIRECTION('ref_axis',(0.,0.,-1.));
#25139=DIRECTION('',(1.,0.,0.));
#25140=DIRECTION('center_axis',(-1.,0.,0.));
#25141=DIRECTION('ref_axis',(0.,0.,1.));
#25142=DIRECTION('center_axis',(1.,0.,0.));
#25143=DIRECTION('ref_axis',(0.,-1.,6.12323399573676E-17));
#25144=DIRECTION('center_axis',(0.,-1.,1.22464679914735E-16));
#25145=DIRECTION('ref_axis',(0.,-1.22464679914735E-16,-1.));
#25146=DIRECTION('center_axis',(1.,0.,0.));
#25147=DIRECTION('ref_axis',(0.,-1.,6.12323399573676E-17));
#25148=DIRECTION('center_axis',(1.,0.,0.));
#25149=DIRECTION('ref_axis',(0.,-1.,0.));
#25150=DIRECTION('',(0.707106781186548,0.707106781186548,-8.65956056235493E-17));
#25151=DIRECTION('center_axis',(-1.,0.,0.));
#25152=DIRECTION('ref_axis',(0.,-1.,6.12323399573676E-17));
#25153=DIRECTION('center_axis',(-1.,0.,0.));
#25154=DIRECTION('ref_axis',(0.,-1.,6.12323399573676E-17));
#25155=DIRECTION('center_axis',(1.,0.,0.));
#25156=DIRECTION('ref_axis',(0.,0.,-1.));
#25157=DIRECTION('center_axis',(0.,-1.,-1.22464679914735E-16));
#25158=DIRECTION('ref_axis',(0.,-1.22464679914735E-16,1.));
#25159=DIRECTION('center_axis',(0.,-0.908282142847613,-0.41835815873979));
#25160=DIRECTION('ref_axis',(0.,0.41835815873979,-0.908282142847613));
#25161=DIRECTION('',(1.,0.,0.));
#25162=DIRECTION('center_axis',(1.,0.,0.));
#25163=DIRECTION('ref_axis',(0.,-0.41835815873979,0.908282142847614));
#25164=DIRECTION('center_axis',(1.,0.,0.));
#25165=DIRECTION('ref_axis',(0.,0.908282142847613,0.418358158739791));
#25166=DIRECTION('center_axis',(1.,0.,0.));
#25167=DIRECTION('ref_axis',(0.,0.,-1.));
#25168=DIRECTION('center_axis',(1.,0.,0.));
#25169=DIRECTION('ref_axis',(0.,0.,-1.));
#25170=DIRECTION('center_axis',(1.,0.,0.));
#25171=DIRECTION('ref_axis',(0.,0.,-1.));
#25172=DIRECTION('center_axis',(1.,0.,0.));
#25173=DIRECTION('ref_axis',(0.,0.,-1.));
#25174=DIRECTION('center_axis',(0.,0.707106781186548,-0.707106781186548));
#25175=DIRECTION('ref_axis',(0.,0.707106781186548,0.707106781186548));
#25176=DIRECTION('',(0.,-0.707106781186548,-0.707106781186548));
#25177=DIRECTION('center_axis',(1.,0.,0.));
#25178=DIRECTION('ref_axis',(0.,0.,-1.));
#25179=DIRECTION('center_axis',(1.,0.,0.));
#25180=DIRECTION('ref_axis',(0.,0.,-1.));
#25181=DIRECTION('center_axis',(1.,0.,0.));
#25182=DIRECTION('ref_axis',(0.,0.,-1.));
#25183=DIRECTION('center_axis',(1.,0.,0.));
#25184=DIRECTION('ref_axis',(0.,0.,-1.));
#25185=DIRECTION('center_axis',(1.,0.,0.));
#25186=DIRECTION('ref_axis',(0.,0.,-1.));
#25187=DIRECTION('center_axis',(0.,0.707106781186548,-0.707106781186548));
#25188=DIRECTION('ref_axis',(0.,0.707106781186548,0.707106781186548));
#25189=DIRECTION('center_axis',(1.,0.,0.));
#25190=DIRECTION('ref_axis',(0.,1.,0.));
#25191=DIRECTION('',(1.,0.,0.));
#25192=DIRECTION('center_axis',(1.,0.,0.));
#25193=DIRECTION('ref_axis',(0.,0.,-1.));
#25194=DIRECTION('',(-1.,0.,0.));
#25195=DIRECTION('center_axis',(1.,0.,0.));
#25196=DIRECTION('ref_axis',(0.,0.,-1.));
#25197=DIRECTION('',(-1.,0.,0.));
#25198=DIRECTION('center_axis',(1.,0.,0.));
#25199=DIRECTION('ref_axis',(0.,0.,-1.));
#25200=DIRECTION('',(-1.,0.,0.));
#25201=DIRECTION('axis',(0.,0.,1.));
#25202=DIRECTION('refdir',(1.,0.,0.));
#25203=DIRECTION('center_axis',(1.,0.,0.));
#25204=DIRECTION('ref_axis',(0.,-1.,0.));
#25205=DIRECTION('center_axis',(-1.,0.,0.));
#25206=DIRECTION('ref_axis',(0.,-1.,0.));
#25207=DIRECTION('center_axis',(-1.,0.,0.));
#25208=DIRECTION('ref_axis',(0.,-1.,0.));
#25209=DIRECTION('',(0.707106781186546,0.70710678118655,-8.65956056235496E-17));
#25210=DIRECTION('center_axis',(1.,0.,0.));
#25211=DIRECTION('ref_axis',(0.,-1.,0.));
#25212=DIRECTION('center_axis',(1.,0.,0.));
#25213=DIRECTION('ref_axis',(0.,1.,0.));
#25214=DIRECTION('',(-1.,0.,0.));
#25215=DIRECTION('center_axis',(1.,0.,0.));
#25216=DIRECTION('ref_axis',(0.,-1.,0.));
#25217=DIRECTION('center_axis',(1.,0.,0.));
#25218=DIRECTION('ref_axis',(0.,-1.,0.));
#25219=DIRECTION('center_axis',(1.,0.,0.));
#25220=DIRECTION('ref_axis',(0.,0.,-1.));
#25221=DIRECTION('center_axis',(1.,0.,0.));
#25222=DIRECTION('ref_axis',(0.,0.947793690616251,-0.318884179645254));
#25223=DIRECTION('center_axis',(1.,0.,0.));
#25224=DIRECTION('ref_axis',(0.,0.,-1.));
#25225=DIRECTION('center_axis',(1.,0.,0.));
#25226=DIRECTION('ref_axis',(0.,0.992291268649497,0.123927552069634));
#25227=DIRECTION('center_axis',(1.,0.,0.));
#25228=DIRECTION('ref_axis',(0.,0.,-1.));
#25229=DIRECTION('center_axis',(1.,0.,0.));
#25230=DIRECTION('ref_axis',(0.,0.840253391272934,0.542193912225445));
#25231=DIRECTION('center_axis',(1.,0.,0.));
#25232=DIRECTION('ref_axis',(0.,0.,-1.));
#25233=DIRECTION('center_axis',(1.,0.,0.));
#25234=DIRECTION('ref_axis',(0.,0.521793024723191,0.853072118493052));
#25235=DIRECTION('center_axis',(1.,0.,0.));
#25236=DIRECTION('ref_axis',(0.,0.,-1.));
#25237=DIRECTION('center_axis',(1.,0.,0.));
#25238=DIRECTION('ref_axis',(0.,0.0999851502555302,0.994988929450162));
#25239=DIRECTION('center_axis',(1.,0.,0.));
#25240=DIRECTION('ref_axis',(0.,0.,-1.));
#25241=DIRECTION('center_axis',(1.,0.,0.));
#25242=DIRECTION('ref_axis',(0.,-0.341626009457634,0.939835980191253));
#25243=DIRECTION('center_axis',(1.,0.,0.));
#25244=DIRECTION('ref_axis',(0.,0.,-1.));
#25245=DIRECTION('center_axis',(1.,0.,0.));
#25246=DIRECTION('ref_axis',(0.,-0.715573948229662,0.698536988723585));
#25247=DIRECTION('center_axis',(1.,0.,0.));
#25248=DIRECTION('ref_axis',(0.,0.,-1.));
#25249=DIRECTION('center_axis',(1.,0.,0.));
#25250=DIRECTION('ref_axis',(0.,-0.947793690616251,0.318884179645253));
#25251=DIRECTION('center_axis',(1.,0.,0.));
#25252=DIRECTION('ref_axis',(0.,0.,-1.));
#25253=DIRECTION('center_axis',(1.,0.,0.));
#25254=DIRECTION('ref_axis',(0.,-0.992291268649497,-0.123927552069633));
#25255=DIRECTION('center_axis',(1.,0.,0.));
#25256=DIRECTION('ref_axis',(0.,0.,-1.));
#25257=DIRECTION('center_axis',(1.,0.,0.));
#25258=DIRECTION('ref_axis',(0.,-0.840253391272934,-0.542193912225445));
#25259=DIRECTION('center_axis',(1.,0.,0.));
#25260=DIRECTION('ref_axis',(0.,0.,-1.));
#25261=DIRECTION('center_axis',(1.,0.,0.));
#25262=DIRECTION('ref_axis',(0.,-0.521793024723191,-0.853072118493052));
#25263=DIRECTION('center_axis',(1.,0.,0.));
#25264=DIRECTION('ref_axis',(0.,0.,-1.));
#25265=DIRECTION('center_axis',(1.,0.,0.));
#25266=DIRECTION('ref_axis',(0.,-0.0999851502555303,-0.994988929450162));
#25267=DIRECTION('center_axis',(1.,0.,0.));
#25268=DIRECTION('ref_axis',(0.,0.,-1.));
#25269=DIRECTION('center_axis',(1.,0.,0.));
#25270=DIRECTION('ref_axis',(0.,0.341626009457634,-0.939835980191253));
#25271=DIRECTION('center_axis',(1.,0.,0.));
#25272=DIRECTION('ref_axis',(0.,0.,-1.));
#25273=DIRECTION('center_axis',(1.,0.,0.));
#25274=DIRECTION('ref_axis',(0.,0.715573948229662,-0.698536988723585));
#25275=DIRECTION('center_axis',(1.,0.,0.));
#25276=DIRECTION('ref_axis',(0.,0.,-1.));
#25277=DIRECTION('center_axis',(-1.,0.,0.));
#25278=DIRECTION('ref_axis',(0.,-1.,0.));
#25279=DIRECTION('center_axis',(-1.,0.,0.));
#25280=DIRECTION('ref_axis',(0.,-1.,0.));
#25281=DIRECTION('',(0.707106781186551,-0.707106781186544,8.65956056235489E-17));
#25282=DIRECTION('center_axis',(-1.,0.,0.));
#25283=DIRECTION('ref_axis',(0.,0.,1.));
#25284=DIRECTION('center_axis',(-1.,0.,0.));
#25285=DIRECTION('ref_axis',(0.,0.984693235726434,-0.174296389849606));
#25286=DIRECTION('center_axis',(1.,0.,0.));
#25287=DIRECTION('ref_axis',(0.,0.,-1.));
#25288=DIRECTION('center_axis',(-1.,0.,0.));
#25289=DIRECTION('ref_axis',(0.,0.910411537476949,-0.413703797938643));
#25290=DIRECTION('center_axis',(1.,0.,0.));
#25291=DIRECTION('ref_axis',(0.,0.,-1.));
#25292=DIRECTION('center_axis',(-1.,0.,0.));
#25293=DIRECTION('ref_axis',(0.,0.778925334068368,-0.627116674907055));
#25294=DIRECTION('center_axis',(1.,0.,0.));
#25295=DIRECTION('ref_axis',(0.,0.,-1.));
#25296=DIRECTION('center_axis',(-1.,0.,0.));
#25297=DIRECTION('ref_axis',(0.,0.598496387233281,-0.801125504817261));
#25298=DIRECTION('center_axis',(1.,0.,0.));
#25299=DIRECTION('ref_axis',(0.,0.,-1.));
#25300=DIRECTION('center_axis',(-1.,0.,0.));
#25301=DIRECTION('ref_axis',(0.,0.380461711272584,-0.924796672926291));
#25302=DIRECTION('center_axis',(1.,0.,0.));
#25303=DIRECTION('ref_axis',(0.,0.,-1.));
#25304=DIRECTION('center_axis',(-1.,0.,0.));
#25305=DIRECTION('ref_axis',(0.,0.138521226752336,-0.990359464911114));
#25306=DIRECTION('center_axis',(1.,0.,0.));
#25307=DIRECTION('ref_axis',(0.,0.,-1.));
#25308=DIRECTION('center_axis',(-1.,0.,0.));
#25309=DIRECTION('ref_axis',(0.,-0.112123055890198,-0.993694329428242));
#25310=DIRECTION('center_axis',(1.,0.,0.));
#25311=DIRECTION('ref_axis',(0.,0.,-1.));
#25312=DIRECTION('center_axis',(-1.,0.,0.));
#25313=DIRECTION('ref_axis',(0.,-0.355722234571395,-0.93459172467529));
#25314=DIRECTION('center_axis',(1.,0.,0.));
#25315=DIRECTION('ref_axis',(0.,0.,-1.));
#25316=DIRECTION('center_axis',(-1.,0.,0.));
#25317=DIRECTION('ref_axis',(0.,-0.576970076999607,-0.816765284673061));
#25318=DIRECTION('center_axis',(1.,0.,0.));
#25319=DIRECTION('ref_axis',(0.,0.,-1.));
#25320=DIRECTION('center_axis',(-1.,0.,0.));
#25321=DIRECTION('ref_axis',(0.,-0.761964767542423,-0.64761847798223));
#25322=DIRECTION('center_axis',(1.,0.,0.));
#25323=DIRECTION('ref_axis',(0.,0.,-1.));
#25324=DIRECTION('center_axis',(-1.,0.,0.));
#25325=DIRECTION('ref_axis',(0.,-0.899082409430159,-0.437779420545621));
#25326=DIRECTION('center_axis',(1.,0.,0.));
#25327=DIRECTION('ref_axis',(0.,0.,-1.));
#25328=DIRECTION('center_axis',(-1.,0.,0.));
#25329=DIRECTION('ref_axis',(0.,-0.979707396939596,-0.200433072076046));
#25330=DIRECTION('center_axis',(1.,0.,0.));
#25331=DIRECTION('ref_axis',(0.,0.,-1.));
#25332=DIRECTION('center_axis',(-1.,0.,0.));
#25333=DIRECTION('ref_axis',(0.,-0.998773765587553,0.0495072234533422));
#25334=DIRECTION('center_axis',(1.,0.,0.));
#25335=DIRECTION('ref_axis',(0.,0.,-1.));
#25336=DIRECTION('center_axis',(-1.,0.,0.));
#25337=DIRECTION('ref_axis',(0.,-0.955083505310682,0.296336798058325));
#25338=DIRECTION('center_axis',(1.,0.,0.));
#25339=DIRECTION('ref_axis',(0.,0.,-1.));
#25340=DIRECTION('center_axis',(-1.,0.,0.));
#25341=DIRECTION('ref_axis',(0.,-0.851381835843715,0.524546441790797));
#25342=DIRECTION('center_axis',(1.,0.,0.));
#25343=DIRECTION('ref_axis',(0.,0.,-1.));
#25344=DIRECTION('center_axis',(-1.,0.,0.));
#25345=DIRECTION('ref_axis',(0.,-0.694184714467323,0.719796903438686));
#25346=DIRECTION('center_axis',(1.,0.,0.));
#25347=DIRECTION('ref_axis',(0.,0.,-1.));
#25348=DIRECTION('center_axis',(-1.,0.,0.));
#25349=DIRECTION('ref_axis',(0.,-0.493369414448157,0.869819878415688));
#25350=DIRECTION('center_axis',(1.,0.,0.));
#25351=DIRECTION('ref_axis',(0.,0.,-1.));
#25352=DIRECTION('center_axis',(-1.,0.,0.));
#25353=DIRECTION('ref_axis',(0.,-0.261553899633433,0.965188871458091));
#25354=DIRECTION('center_axis',(1.,0.,0.));
#25355=DIRECTION('ref_axis',(0.,0.,-1.));
#25356=DIRECTION('center_axis',(-1.,0.,0.));
#25357=DIRECTION('ref_axis',(0.,-0.0133039913767846,0.99991149799042));
#25358=DIRECTION('center_axis',(1.,0.,0.));
#25359=DIRECTION('ref_axis',(0.,0.,-1.));
#25360=DIRECTION('center_axis',(-1.,0.,0.));
#25361=DIRECTION('ref_axis',(0.,0.235781855586725,0.971806007686761));
#25362=DIRECTION('center_axis',(1.,0.,0.));
#25363=DIRECTION('ref_axis',(0.,0.,-1.));
#25364=DIRECTION('center_axis',(-1.,0.,0.));
#25365=DIRECTION('ref_axis',(0.,0.470052661418713,0.882638371867655));
#25366=DIRECTION('center_axis',(1.,0.,0.));
#25367=DIRECTION('ref_axis',(0.,0.,-1.));
#25368=DIRECTION('center_axis',(-1.,0.,0.));
#25369=DIRECTION('ref_axis',(0.,0.674788329801001,0.738011321027242));
#25370=DIRECTION('center_axis',(1.,0.,0.));
#25371=DIRECTION('ref_axis',(0.,0.,-1.));
#25372=DIRECTION('center_axis',(-1.,0.,0.));
#25373=DIRECTION('ref_axis',(0.,0.837124565724013,0.547012304670911));
#25374=DIRECTION('center_axis',(1.,0.,0.));
#25375=DIRECTION('ref_axis',(0.,0.,-1.));
#25376=DIRECTION('center_axis',(-1.,0.,0.));
#25377=DIRECTION('ref_axis',(0.,0.946861186453793,0.321642493441576));
#25378=DIRECTION('center_axis',(1.,0.,0.));
#25379=DIRECTION('ref_axis',(0.,0.,-1.));
#25380=DIRECTION('center_axis',(-1.,0.,0.));
#25381=DIRECTION('ref_axis',(0.,0.99710303652683,0.0760627014309627));
#25382=DIRECTION('center_axis',(1.,0.,0.));
#25383=DIRECTION('ref_axis',(0.,0.,-1.));
#25384=DIRECTION('',(1.,0.,0.));
#25385=DIRECTION('center_axis',(1.,0.,0.));
#25386=DIRECTION('ref_axis',(0.,0.947793690616251,-0.318884179645254));
#25387=DIRECTION('center_axis',(1.,0.,0.));
#25388=DIRECTION('ref_axis',(0.,0.947793690616251,-0.318884179645254));
#25389=DIRECTION('',(1.,0.,0.));
#25390=DIRECTION('center_axis',(-1.,0.,0.));
#25391=DIRECTION('ref_axis',(0.,1.,0.));
#25392=DIRECTION('center_axis',(1.,0.,0.));
#25393=DIRECTION('ref_axis',(0.,0.,-1.));
#25394=DIRECTION('center_axis',(1.,0.,0.));
#25395=DIRECTION('ref_axis',(0.,1.,0.));
#25396=DIRECTION('center_axis',(1.,0.,0.));
#25397=DIRECTION('ref_axis',(0.,0.,-1.));
#25398=DIRECTION('',(1.,0.,0.));
#25399=DIRECTION('center_axis',(1.,0.,0.));
#25400=DIRECTION('ref_axis',(0.,0.715573948229662,-0.698536988723585));
#25401=DIRECTION('center_axis',(1.,0.,0.));
#25402=DIRECTION('ref_axis',(0.,0.715573948229662,-0.698536988723585));
#25403=DIRECTION('',(1.,0.,0.));
#25404=DIRECTION('center_axis',(1.,0.,0.));
#25405=DIRECTION('ref_axis',(0.,0.,-1.));
#25406=DIRECTION('center_axis',(1.,0.,0.));
#25407=DIRECTION('ref_axis',(0.,0.,-1.));
#25408=DIRECTION('center_axis',(1.,0.,0.));
#25409=DIRECTION('ref_axis',(0.,0.99710303652683,0.0760627014309627));
#25410=DIRECTION('center_axis',(1.,0.,0.));
#25411=DIRECTION('ref_axis',(0.,0.,-1.));
#25412=DIRECTION('center_axis',(1.,0.,0.));
#25413=DIRECTION('ref_axis',(0.,0.946861186453793,0.321642493441576));
#25414=DIRECTION('center_axis',(1.,0.,0.));
#25415=DIRECTION('ref_axis',(0.,0.,-1.));
#25416=DIRECTION('center_axis',(1.,0.,0.));
#25417=DIRECTION('ref_axis',(0.,0.837124565724013,0.547012304670911));
#25418=DIRECTION('center_axis',(1.,0.,0.));
#25419=DIRECTION('ref_axis',(0.,0.,-1.));
#25420=DIRECTION('center_axis',(1.,0.,0.));
#25421=DIRECTION('ref_axis',(0.,0.674788329801001,0.738011321027242));
#25422=DIRECTION('center_axis',(1.,0.,0.));
#25423=DIRECTION('ref_axis',(0.,0.,-1.));
#25424=DIRECTION('center_axis',(1.,0.,0.));
#25425=DIRECTION('ref_axis',(0.,0.470052661418713,0.882638371867655));
#25426=DIRECTION('center_axis',(1.,0.,0.));
#25427=DIRECTION('ref_axis',(0.,0.,-1.));
#25428=DIRECTION('center_axis',(1.,0.,0.));
#25429=DIRECTION('ref_axis',(0.,0.235781855586725,0.971806007686761));
#25430=DIRECTION('center_axis',(1.,0.,0.));
#25431=DIRECTION('ref_axis',(0.,0.,-1.));
#25432=DIRECTION('center_axis',(1.,0.,0.));
#25433=DIRECTION('ref_axis',(0.,-0.0133039913767846,0.99991149799042));
#25434=DIRECTION('center_axis',(1.,0.,0.));
#25435=DIRECTION('ref_axis',(0.,0.,-1.));
#25436=DIRECTION('center_axis',(1.,0.,0.));
#25437=DIRECTION('ref_axis',(0.,-0.261553899633433,0.965188871458091));
#25438=DIRECTION('center_axis',(1.,0.,0.));
#25439=DIRECTION('ref_axis',(0.,0.,-1.));
#25440=DIRECTION('center_axis',(1.,0.,0.));
#25441=DIRECTION('ref_axis',(0.,-0.493369414448157,0.869819878415688));
#25442=DIRECTION('center_axis',(1.,0.,0.));
#25443=DIRECTION('ref_axis',(0.,0.,-1.));
#25444=DIRECTION('center_axis',(1.,0.,0.));
#25445=DIRECTION('ref_axis',(0.,-0.694184714467323,0.719796903438686));
#25446=DIRECTION('center_axis',(1.,0.,0.));
#25447=DIRECTION('ref_axis',(0.,0.,-1.));
#25448=DIRECTION('center_axis',(1.,0.,0.));
#25449=DIRECTION('ref_axis',(0.,-0.851381835843715,0.524546441790797));
#25450=DIRECTION('center_axis',(1.,0.,0.));
#25451=DIRECTION('ref_axis',(0.,0.,-1.));
#25452=DIRECTION('center_axis',(1.,0.,0.));
#25453=DIRECTION('ref_axis',(0.,-0.955083505310682,0.296336798058325));
#25454=DIRECTION('center_axis',(1.,0.,0.));
#25455=DIRECTION('ref_axis',(0.,0.,-1.));
#25456=DIRECTION('center_axis',(1.,0.,0.));
#25457=DIRECTION('ref_axis',(0.,-0.998773765587553,0.0495072234533422));
#25458=DIRECTION('center_axis',(1.,0.,0.));
#25459=DIRECTION('ref_axis',(0.,0.,-1.));
#25460=DIRECTION('center_axis',(1.,0.,0.));
#25461=DIRECTION('ref_axis',(0.,-0.979707396939596,-0.200433072076046));
#25462=DIRECTION('center_axis',(1.,0.,0.));
#25463=DIRECTION('ref_axis',(0.,0.,-1.));
#25464=DIRECTION('center_axis',(1.,0.,0.));
#25465=DIRECTION('ref_axis',(0.,-0.899082409430159,-0.437779420545621));
#25466=DIRECTION('center_axis',(1.,0.,0.));
#25467=DIRECTION('ref_axis',(0.,0.,-1.));
#25468=DIRECTION('center_axis',(1.,0.,0.));
#25469=DIRECTION('ref_axis',(0.,-0.761964767542423,-0.64761847798223));
#25470=DIRECTION('center_axis',(1.,0.,0.));
#25471=DIRECTION('ref_axis',(0.,0.,-1.));
#25472=DIRECTION('center_axis',(1.,0.,0.));
#25473=DIRECTION('ref_axis',(0.,-0.576970076999607,-0.816765284673061));
#25474=DIRECTION('center_axis',(1.,0.,0.));
#25475=DIRECTION('ref_axis',(0.,0.,-1.));
#25476=DIRECTION('center_axis',(1.,0.,0.));
#25477=DIRECTION('ref_axis',(0.,-0.355722234571395,-0.93459172467529));
#25478=DIRECTION('center_axis',(1.,0.,0.));
#25479=DIRECTION('ref_axis',(0.,0.,-1.));
#25480=DIRECTION('center_axis',(1.,0.,0.));
#25481=DIRECTION('ref_axis',(0.,-0.112123055890198,-0.993694329428242));
#25482=DIRECTION('center_axis',(1.,0.,0.));
#25483=DIRECTION('ref_axis',(0.,0.,-1.));
#25484=DIRECTION('center_axis',(1.,0.,0.));
#25485=DIRECTION('ref_axis',(0.,0.138521226752336,-0.990359464911114));
#25486=DIRECTION('center_axis',(1.,0.,0.));
#25487=DIRECTION('ref_axis',(0.,0.,-1.));
#25488=DIRECTION('center_axis',(1.,0.,0.));
#25489=DIRECTION('ref_axis',(0.,0.380461711272584,-0.924796672926291));
#25490=DIRECTION('center_axis',(1.,0.,0.));
#25491=DIRECTION('ref_axis',(0.,0.,-1.));
#25492=DIRECTION('center_axis',(1.,0.,0.));
#25493=DIRECTION('ref_axis',(0.,0.598496387233281,-0.801125504817261));
#25494=DIRECTION('center_axis',(1.,0.,0.));
#25495=DIRECTION('ref_axis',(0.,0.,-1.));
#25496=DIRECTION('center_axis',(1.,0.,0.));
#25497=DIRECTION('ref_axis',(0.,0.778925334068368,-0.627116674907055));
#25498=DIRECTION('center_axis',(1.,0.,0.));
#25499=DIRECTION('ref_axis',(0.,0.,-1.));
#25500=DIRECTION('center_axis',(1.,0.,0.));
#25501=DIRECTION('ref_axis',(0.,0.910411537476949,-0.413703797938643));
#25502=DIRECTION('center_axis',(1.,0.,0.));
#25503=DIRECTION('ref_axis',(0.,0.,-1.));
#25504=DIRECTION('center_axis',(1.,0.,0.));
#25505=DIRECTION('ref_axis',(0.,0.984693235726434,-0.174296389849606));
#25506=DIRECTION('center_axis',(1.,0.,0.));
#25507=DIRECTION('ref_axis',(0.,0.,-1.));
#25508=DIRECTION('center_axis',(1.,0.,0.));
#25509=DIRECTION('ref_axis',(0.,0.,-1.));
#25510=DIRECTION('center_axis',(1.,0.,0.));
#25511=DIRECTION('ref_axis',(0.,0.341626009457634,-0.939835980191253));
#25512=DIRECTION('center_axis',(1.,0.,0.));
#25513=DIRECTION('ref_axis',(0.,0.,-1.));
#25514=DIRECTION('center_axis',(1.,0.,0.));
#25515=DIRECTION('ref_axis',(0.,-0.0999851502555303,-0.994988929450162));
#25516=DIRECTION('center_axis',(1.,0.,0.));
#25517=DIRECTION('ref_axis',(0.,0.,-1.));
#25518=DIRECTION('center_axis',(1.,0.,0.));
#25519=DIRECTION('ref_axis',(0.,-0.521793024723191,-0.853072118493052));
#25520=DIRECTION('center_axis',(1.,0.,0.));
#25521=DIRECTION('ref_axis',(0.,0.,-1.));
#25522=DIRECTION('center_axis',(1.,0.,0.));
#25523=DIRECTION('ref_axis',(0.,-0.840253391272934,-0.542193912225445));
#25524=DIRECTION('center_axis',(1.,0.,0.));
#25525=DIRECTION('ref_axis',(0.,0.,-1.));
#25526=DIRECTION('center_axis',(1.,0.,0.));
#25527=DIRECTION('ref_axis',(0.,-0.992291268649497,-0.123927552069633));
#25528=DIRECTION('center_axis',(1.,0.,0.));
#25529=DIRECTION('ref_axis',(0.,0.,-1.));
#25530=DIRECTION('center_axis',(1.,0.,0.));
#25531=DIRECTION('ref_axis',(0.,-0.947793690616251,0.318884179645253));
#25532=DIRECTION('center_axis',(1.,0.,0.));
#25533=DIRECTION('ref_axis',(0.,0.,-1.));
#25534=DIRECTION('center_axis',(1.,0.,0.));
#25535=DIRECTION('ref_axis',(0.,-0.715573948229662,0.698536988723585));
#25536=DIRECTION('center_axis',(1.,0.,0.));
#25537=DIRECTION('ref_axis',(0.,0.,-1.));
#25538=DIRECTION('center_axis',(1.,0.,0.));
#25539=DIRECTION('ref_axis',(0.,-0.341626009457634,0.939835980191253));
#25540=DIRECTION('center_axis',(1.,0.,0.));
#25541=DIRECTION('ref_axis',(0.,0.,-1.));
#25542=DIRECTION('center_axis',(1.,0.,0.));
#25543=DIRECTION('ref_axis',(0.,0.0999851502555302,0.994988929450162));
#25544=DIRECTION('center_axis',(1.,0.,0.));
#25545=DIRECTION('ref_axis',(0.,0.,-1.));
#25546=DIRECTION('center_axis',(1.,0.,0.));
#25547=DIRECTION('ref_axis',(0.,0.521793024723191,0.853072118493052));
#25548=DIRECTION('center_axis',(1.,0.,0.));
#25549=DIRECTION('ref_axis',(0.,0.,-1.));
#25550=DIRECTION('center_axis',(1.,0.,0.));
#25551=DIRECTION('ref_axis',(0.,0.840253391272934,0.542193912225445));
#25552=DIRECTION('center_axis',(1.,0.,0.));
#25553=DIRECTION('ref_axis',(0.,0.,-1.));
#25554=DIRECTION('center_axis',(1.,0.,0.));
#25555=DIRECTION('ref_axis',(0.,0.992291268649497,0.123927552069634));
#25556=DIRECTION('center_axis',(1.,0.,0.));
#25557=DIRECTION('ref_axis',(0.,1.,0.));
#25558=DIRECTION('center_axis',(1.,0.,0.));
#25559=DIRECTION('ref_axis',(0.,0.,-1.));
#25560=DIRECTION('center_axis',(-1.,0.,0.));
#25561=DIRECTION('ref_axis',(0.,1.,0.));
#25562=DIRECTION('',(1.,0.,0.));
#25563=DIRECTION('center_axis',(1.,0.,0.));
#25564=DIRECTION('ref_axis',(0.,0.341626009457634,-0.939835980191253));
#25565=DIRECTION('',(1.,0.,0.));
#25566=DIRECTION('center_axis',(-1.,0.,0.));
#25567=DIRECTION('ref_axis',(0.,1.,0.));
#25568=DIRECTION('center_axis',(1.,0.,0.));
#25569=DIRECTION('ref_axis',(0.,0.,-1.));
#25570=DIRECTION('center_axis',(1.,0.,0.));
#25571=DIRECTION('ref_axis',(0.,1.,0.));
#25572=DIRECTION('',(1.,0.,0.));
#25573=DIRECTION('center_axis',(1.,0.,0.));
#25574=DIRECTION('ref_axis',(0.,-0.0999851502555303,-0.994988929450162));
#25575=DIRECTION('',(1.,0.,0.));
#25576=DIRECTION('center_axis',(1.,0.,0.));
#25577=DIRECTION('ref_axis',(0.,1.,0.));
#25578=DIRECTION('center_axis',(1.,0.,0.));
#25579=DIRECTION('ref_axis',(0.,0.,-1.));
#25580=DIRECTION('center_axis',(-1.,0.,0.));
#25581=DIRECTION('ref_axis',(0.,1.,0.));
#25582=DIRECTION('',(1.,0.,0.));
#25583=DIRECTION('center_axis',(1.,0.,0.));
#25584=DIRECTION('ref_axis',(0.,-0.521793024723191,-0.853072118493052));
#25585=DIRECTION('',(1.,0.,0.));
#25586=DIRECTION('center_axis',(-1.,0.,0.));
#25587=DIRECTION('ref_axis',(0.,1.,0.));
#25588=DIRECTION('center_axis',(1.,0.,0.));
#25589=DIRECTION('ref_axis',(0.,0.,-1.));
#25590=DIRECTION('center_axis',(1.,0.,0.));
#25591=DIRECTION('ref_axis',(0.,1.,0.));
#25592=DIRECTION('',(1.,0.,0.));
#25593=DIRECTION('center_axis',(1.,0.,0.));
#25594=DIRECTION('ref_axis',(0.,-0.840253391272934,-0.542193912225445));
#25595=DIRECTION('',(1.,0.,0.));
#25596=DIRECTION('center_axis',(1.,0.,0.));
#25597=DIRECTION('ref_axis',(0.,1.,0.));
#25598=DIRECTION('center_axis',(1.,0.,0.));
#25599=DIRECTION('ref_axis',(0.,0.,-1.));
#25600=DIRECTION('center_axis',(-1.,0.,0.));
#25601=DIRECTION('ref_axis',(0.,1.,0.));
#25602=DIRECTION('',(1.,0.,0.));
#25603=DIRECTION('center_axis',(1.,0.,0.));
#25604=DIRECTION('ref_axis',(0.,-0.992291268649497,-0.123927552069633));
#25605=DIRECTION('',(1.,0.,0.));
#25606=DIRECTION('center_axis',(-1.,0.,0.));
#25607=DIRECTION('ref_axis',(0.,1.,0.));
#25608=DIRECTION('center_axis',(1.,0.,0.));
#25609=DIRECTION('ref_axis',(0.,0.,-1.));
#25610=DIRECTION('center_axis',(1.,0.,0.));
#25611=DIRECTION('ref_axis',(0.,1.,0.));
#25612=DIRECTION('',(1.,0.,0.));
#25613=DIRECTION('center_axis',(1.,0.,0.));
#25614=DIRECTION('ref_axis',(0.,-0.947793690616251,0.318884179645253));
#25615=DIRECTION('',(1.,0.,0.));
#25616=DIRECTION('center_axis',(1.,0.,0.));
#25617=DIRECTION('ref_axis',(0.,1.,0.));
#25618=DIRECTION('center_axis',(1.,0.,0.));
#25619=DIRECTION('ref_axis',(0.,0.,-1.));
#25620=DIRECTION('center_axis',(-1.,0.,0.));
#25621=DIRECTION('ref_axis',(0.,1.,0.));
#25622=DIRECTION('',(1.,0.,0.));
#25623=DIRECTION('center_axis',(1.,0.,0.));
#25624=DIRECTION('ref_axis',(0.,-0.715573948229662,0.698536988723585));
#25625=DIRECTION('',(1.,0.,0.));
#25626=DIRECTION('center_axis',(-1.,0.,0.));
#25627=DIRECTION('ref_axis',(0.,-0.99999975051671,-0.000706375620521827));
#25628=DIRECTION('center_axis',(1.,0.,0.));
#25629=DIRECTION('ref_axis',(0.,0.,-1.));
#25630=DIRECTION('center_axis',(1.,0.,0.));
#25631=DIRECTION('ref_axis',(0.,-0.99999795302892,0.00202334820765901));
#25632=DIRECTION('',(1.,0.,0.));
#25633=DIRECTION('center_axis',(1.,0.,0.));
#25634=DIRECTION('ref_axis',(0.,-0.341626009457634,0.939835980191253));
#25635=DIRECTION('',(1.,0.,0.));
#25636=DIRECTION('center_axis',(1.,0.,0.));
#25637=DIRECTION('ref_axis',(0.,1.,0.));
#25638=DIRECTION('center_axis',(1.,0.,0.));
#25639=DIRECTION('ref_axis',(0.,0.,-1.));
#25640=DIRECTION('center_axis',(-1.,0.,0.));
#25641=DIRECTION('ref_axis',(0.,1.,0.));
#25642=DIRECTION('',(1.,0.,0.));
#25643=DIRECTION('center_axis',(1.,0.,0.));
#25644=DIRECTION('ref_axis',(0.,0.0999851502555302,0.994988929450162));
#25645=DIRECTION('',(1.,0.,0.));
#25646=DIRECTION('center_axis',(-1.,0.,0.));
#25647=DIRECTION('ref_axis',(0.,1.,0.));
#25648=DIRECTION('center_axis',(1.,0.,0.));
#25649=DIRECTION('ref_axis',(0.,0.,-1.));
#25650=DIRECTION('center_axis',(1.,0.,0.));
#25651=DIRECTION('ref_axis',(0.,1.,0.));
#25652=DIRECTION('',(1.,0.,0.));
#25653=DIRECTION('center_axis',(1.,0.,0.));
#25654=DIRECTION('ref_axis',(0.,0.521793024723191,0.853072118493052));
#25655=DIRECTION('',(1.,0.,0.));
#25656=DIRECTION('center_axis',(1.,0.,0.));
#25657=DIRECTION('ref_axis',(0.,1.,0.));
#25658=DIRECTION('center_axis',(1.,0.,0.));
#25659=DIRECTION('ref_axis',(0.,0.,-1.));
#25660=DIRECTION('center_axis',(-1.,0.,0.));
#25661=DIRECTION('ref_axis',(0.,1.,0.));
#25662=DIRECTION('',(1.,0.,0.));
#25663=DIRECTION('center_axis',(1.,0.,0.));
#25664=DIRECTION('ref_axis',(0.,0.840253391272934,0.542193912225445));
#25665=DIRECTION('',(1.,0.,0.));
#25666=DIRECTION('center_axis',(-1.,0.,0.));
#25667=DIRECTION('ref_axis',(0.,1.,0.));
#25668=DIRECTION('center_axis',(1.,0.,0.));
#25669=DIRECTION('ref_axis',(0.,0.,-1.));
#25670=DIRECTION('center_axis',(1.,0.,0.));
#25671=DIRECTION('ref_axis',(0.,1.,0.));
#25672=DIRECTION('',(1.,0.,0.));
#25673=DIRECTION('center_axis',(1.,0.,0.));
#25674=DIRECTION('ref_axis',(0.,0.992291268649497,0.123927552069634));
#25675=DIRECTION('',(1.,0.,0.));
#25676=DIRECTION('',(1.,0.,0.));
#25677=DIRECTION('center_axis',(1.,0.,0.));
#25678=DIRECTION('ref_axis',(0.,0.984693235726434,-0.174296389849606));
#25679=DIRECTION('',(1.,0.,0.));
#25680=DIRECTION('center_axis',(1.,0.,0.));
#25681=DIRECTION('ref_axis',(0.,1.,0.));
#25682=DIRECTION('center_axis',(1.,0.,0.));
#25683=DIRECTION('ref_axis',(0.,0.,-1.));
#25684=DIRECTION('center_axis',(1.,0.,0.));
#25685=DIRECTION('ref_axis',(0.,1.,0.));
#25686=DIRECTION('center_axis',(1.,0.,0.));
#25687=DIRECTION('ref_axis',(0.,0.,-1.));
#25688=DIRECTION('center_axis',(-1.,0.,0.));
#25689=DIRECTION('ref_axis',(0.,1.,0.));
#25690=DIRECTION('',(1.,0.,0.));
#25691=DIRECTION('center_axis',(1.,0.,0.));
#25692=DIRECTION('ref_axis',(0.,0.910411537476949,-0.413703797938643));
#25693=DIRECTION('',(1.,0.,0.));
#25694=DIRECTION('center_axis',(1.,0.,0.));
#25695=DIRECTION('ref_axis',(0.,1.,0.));
#25696=DIRECTION('center_axis',(1.,0.,0.));
#25697=DIRECTION('ref_axis',(0.,0.,-1.));
#25698=DIRECTION('center_axis',(1.,0.,0.));
#25699=DIRECTION('ref_axis',(0.,1.,0.));
#25700=DIRECTION('center_axis',(1.,0.,0.));
#25701=DIRECTION('ref_axis',(0.,0.,-1.));
#25702=DIRECTION('center_axis',(-1.,0.,0.));
#25703=DIRECTION('ref_axis',(0.,1.,0.));
#25704=DIRECTION('',(1.,0.,0.));
#25705=DIRECTION('center_axis',(1.,0.,0.));
#25706=DIRECTION('ref_axis',(0.,0.778925334068368,-0.627116674907055));
#25707=DIRECTION('',(1.,0.,0.));
#25708=DIRECTION('center_axis',(1.,0.,0.));
#25709=DIRECTION('ref_axis',(0.,1.,0.));
#25710=DIRECTION('center_axis',(1.,0.,0.));
#25711=DIRECTION('ref_axis',(0.,0.,-1.));
#25712=DIRECTION('center_axis',(1.,0.,0.));
#25713=DIRECTION('ref_axis',(0.,1.,0.));
#25714=DIRECTION('center_axis',(1.,0.,0.));
#25715=DIRECTION('ref_axis',(0.,0.,-1.));
#25716=DIRECTION('center_axis',(-1.,0.,0.));
#25717=DIRECTION('ref_axis',(0.,1.,0.));
#25718=DIRECTION('',(1.,0.,0.));
#25719=DIRECTION('center_axis',(1.,0.,0.));
#25720=DIRECTION('ref_axis',(0.,0.598496387233281,-0.801125504817261));
#25721=DIRECTION('',(1.,0.,0.));
#25722=DIRECTION('center_axis',(1.,0.,0.));
#25723=DIRECTION('ref_axis',(0.,1.,0.));
#25724=DIRECTION('center_axis',(1.,0.,0.));
#25725=DIRECTION('ref_axis',(0.,0.,-1.));
#25726=DIRECTION('center_axis',(1.,0.,0.));
#25727=DIRECTION('ref_axis',(0.,1.,0.));
#25728=DIRECTION('center_axis',(1.,0.,0.));
#25729=DIRECTION('ref_axis',(0.,0.,-1.));
#25730=DIRECTION('center_axis',(-1.,0.,0.));
#25731=DIRECTION('ref_axis',(0.,1.,0.));
#25732=DIRECTION('',(1.,0.,0.));
#25733=DIRECTION('center_axis',(1.,0.,0.));
#25734=DIRECTION('ref_axis',(0.,0.380461711272584,-0.924796672926291));
#25735=DIRECTION('',(1.,0.,0.));
#25736=DIRECTION('center_axis',(1.,0.,0.));
#25737=DIRECTION('ref_axis',(0.,1.,0.));
#25738=DIRECTION('center_axis',(1.,0.,0.));
#25739=DIRECTION('ref_axis',(0.,0.,-1.));
#25740=DIRECTION('center_axis',(1.,0.,0.));
#25741=DIRECTION('ref_axis',(0.,1.,0.));
#25742=DIRECTION('center_axis',(1.,0.,0.));
#25743=DIRECTION('ref_axis',(0.,0.,-1.));
#25744=DIRECTION('center_axis',(-1.,0.,0.));
#25745=DIRECTION('ref_axis',(0.,1.,0.));
#25746=DIRECTION('',(1.,0.,0.));
#25747=DIRECTION('center_axis',(1.,0.,0.));
#25748=DIRECTION('ref_axis',(0.,0.138521226752336,-0.990359464911114));
#25749=DIRECTION('',(1.,0.,0.));
#25750=DIRECTION('center_axis',(1.,0.,0.));
#25751=DIRECTION('ref_axis',(0.,1.,0.));
#25752=DIRECTION('center_axis',(1.,0.,0.));
#25753=DIRECTION('ref_axis',(0.,0.,-1.));
#25754=DIRECTION('center_axis',(1.,0.,0.));
#25755=DIRECTION('ref_axis',(0.,1.,0.));
#25756=DIRECTION('center_axis',(1.,0.,0.));
#25757=DIRECTION('ref_axis',(0.,0.,-1.));
#25758=DIRECTION('center_axis',(-1.,0.,0.));
#25759=DIRECTION('ref_axis',(0.,1.,0.));
#25760=DIRECTION('',(1.,0.,0.));
#25761=DIRECTION('center_axis',(1.,0.,0.));
#25762=DIRECTION('ref_axis',(0.,-0.112123055890198,-0.993694329428242));
#25763=DIRECTION('',(1.,0.,0.));
#25764=DIRECTION('center_axis',(1.,0.,0.));
#25765=DIRECTION('ref_axis',(0.,1.,0.));
#25766=DIRECTION('center_axis',(1.,0.,0.));
#25767=DIRECTION('ref_axis',(0.,0.,-1.));
#25768=DIRECTION('center_axis',(1.,0.,0.));
#25769=DIRECTION('ref_axis',(0.,1.,0.));
#25770=DIRECTION('center_axis',(1.,0.,0.));
#25771=DIRECTION('ref_axis',(0.,0.,-1.));
#25772=DIRECTION('center_axis',(-1.,0.,0.));
#25773=DIRECTION('ref_axis',(0.,1.,0.));
#25774=DIRECTION('',(1.,0.,0.));
#25775=DIRECTION('center_axis',(1.,0.,0.));
#25776=DIRECTION('ref_axis',(0.,-0.355722234571395,-0.93459172467529));
#25777=DIRECTION('',(1.,0.,0.));
#25778=DIRECTION('center_axis',(1.,0.,0.));
#25779=DIRECTION('ref_axis',(0.,1.,0.));
#25780=DIRECTION('center_axis',(1.,0.,0.));
#25781=DIRECTION('ref_axis',(0.,0.,-1.));
#25782=DIRECTION('center_axis',(1.,0.,0.));
#25783=DIRECTION('ref_axis',(0.,1.,0.));
#25784=DIRECTION('center_axis',(1.,0.,0.));
#25785=DIRECTION('ref_axis',(0.,0.,-1.));
#25786=DIRECTION('center_axis',(-1.,0.,0.));
#25787=DIRECTION('ref_axis',(0.,1.,0.));
#25788=DIRECTION('',(1.,0.,0.));
#25789=DIRECTION('center_axis',(1.,0.,0.));
#25790=DIRECTION('ref_axis',(0.,-0.576970076999607,-0.816765284673061));
#25791=DIRECTION('',(1.,0.,0.));
#25792=DIRECTION('center_axis',(1.,0.,0.));
#25793=DIRECTION('ref_axis',(0.,1.,0.));
#25794=DIRECTION('center_axis',(1.,0.,0.));
#25795=DIRECTION('ref_axis',(0.,0.,-1.));
#25796=DIRECTION('center_axis',(1.,0.,0.));
#25797=DIRECTION('ref_axis',(0.,1.,0.));
#25798=DIRECTION('center_axis',(1.,0.,0.));
#25799=DIRECTION('ref_axis',(0.,0.,-1.));
#25800=DIRECTION('center_axis',(-1.,0.,0.));
#25801=DIRECTION('ref_axis',(0.,1.,0.));
#25802=DIRECTION('',(1.,0.,0.));
#25803=DIRECTION('center_axis',(1.,0.,0.));
#25804=DIRECTION('ref_axis',(0.,-0.761964767542423,-0.64761847798223));
#25805=DIRECTION('',(1.,0.,0.));
#25806=DIRECTION('center_axis',(1.,0.,0.));
#25807=DIRECTION('ref_axis',(0.,1.,0.));
#25808=DIRECTION('center_axis',(1.,0.,0.));
#25809=DIRECTION('ref_axis',(0.,0.,-1.));
#25810=DIRECTION('center_axis',(1.,0.,0.));
#25811=DIRECTION('ref_axis',(0.,1.,0.));
#25812=DIRECTION('center_axis',(1.,0.,0.));
#25813=DIRECTION('ref_axis',(0.,0.,-1.));
#25814=DIRECTION('center_axis',(-1.,0.,0.));
#25815=DIRECTION('ref_axis',(0.,1.,0.));
#25816=DIRECTION('',(1.,0.,0.));
#25817=DIRECTION('center_axis',(1.,0.,0.));
#25818=DIRECTION('ref_axis',(0.,-0.899082409430159,-0.437779420545621));
#25819=DIRECTION('',(1.,0.,0.));
#25820=DIRECTION('center_axis',(1.,0.,0.));
#25821=DIRECTION('ref_axis',(0.,1.,0.));
#25822=DIRECTION('center_axis',(1.,0.,0.));
#25823=DIRECTION('ref_axis',(0.,0.,-1.));
#25824=DIRECTION('center_axis',(1.,0.,0.));
#25825=DIRECTION('ref_axis',(0.,1.,0.));
#25826=DIRECTION('center_axis',(1.,0.,0.));
#25827=DIRECTION('ref_axis',(0.,0.,-1.));
#25828=DIRECTION('center_axis',(-1.,0.,0.));
#25829=DIRECTION('ref_axis',(0.,1.,0.));
#25830=DIRECTION('',(1.,0.,0.));
#25831=DIRECTION('center_axis',(1.,0.,0.));
#25832=DIRECTION('ref_axis',(0.,-0.979707396939596,-0.200433072076046));
#25833=DIRECTION('',(1.,0.,0.));
#25834=DIRECTION('center_axis',(1.,0.,0.));
#25835=DIRECTION('ref_axis',(0.,1.,0.));
#25836=DIRECTION('center_axis',(1.,0.,0.));
#25837=DIRECTION('ref_axis',(0.,0.,-1.));
#25838=DIRECTION('center_axis',(1.,0.,0.));
#25839=DIRECTION('ref_axis',(0.,1.,0.));
#25840=DIRECTION('center_axis',(1.,0.,0.));
#25841=DIRECTION('ref_axis',(0.,0.,-1.));
#25842=DIRECTION('center_axis',(-1.,0.,0.));
#25843=DIRECTION('ref_axis',(0.,1.,0.));
#25844=DIRECTION('',(1.,0.,0.));
#25845=DIRECTION('center_axis',(1.,0.,0.));
#25846=DIRECTION('ref_axis',(0.,-0.998773765587553,0.0495072234533422));
#25847=DIRECTION('',(1.,0.,0.));
#25848=DIRECTION('center_axis',(1.,0.,0.));
#25849=DIRECTION('ref_axis',(0.,1.,0.));
#25850=DIRECTION('center_axis',(1.,0.,0.));
#25851=DIRECTION('ref_axis',(0.,0.,-1.));
#25852=DIRECTION('center_axis',(1.,0.,0.));
#25853=DIRECTION('ref_axis',(0.,1.,0.));
#25854=DIRECTION('center_axis',(1.,0.,0.));
#25855=DIRECTION('ref_axis',(0.,0.,-1.));
#25856=DIRECTION('center_axis',(-1.,0.,0.));
#25857=DIRECTION('ref_axis',(0.,1.,0.));
#25858=DIRECTION('',(1.,0.,0.));
#25859=DIRECTION('center_axis',(1.,0.,0.));
#25860=DIRECTION('ref_axis',(0.,-0.955083505310682,0.296336798058325));
#25861=DIRECTION('',(1.,0.,0.));
#25862=DIRECTION('center_axis',(1.,0.,0.));
#25863=DIRECTION('ref_axis',(0.,1.,0.));
#25864=DIRECTION('center_axis',(1.,0.,0.));
#25865=DIRECTION('ref_axis',(0.,0.,-1.));
#25866=DIRECTION('center_axis',(1.,0.,0.));
#25867=DIRECTION('ref_axis',(0.,1.,0.));
#25868=DIRECTION('center_axis',(1.,0.,0.));
#25869=DIRECTION('ref_axis',(0.,0.,-1.));
#25870=DIRECTION('center_axis',(-1.,0.,0.));
#25871=DIRECTION('ref_axis',(0.,1.,0.));
#25872=DIRECTION('',(1.,0.,0.));
#25873=DIRECTION('center_axis',(1.,0.,0.));
#25874=DIRECTION('ref_axis',(0.,-0.851381835843715,0.524546441790797));
#25875=DIRECTION('',(1.,0.,0.));
#25876=DIRECTION('center_axis',(1.,0.,0.));
#25877=DIRECTION('ref_axis',(0.,1.,0.));
#25878=DIRECTION('center_axis',(1.,0.,0.));
#25879=DIRECTION('ref_axis',(0.,0.,-1.));
#25880=DIRECTION('center_axis',(1.,0.,0.));
#25881=DIRECTION('ref_axis',(0.,1.,0.));
#25882=DIRECTION('center_axis',(1.,0.,0.));
#25883=DIRECTION('ref_axis',(0.,0.,-1.));
#25884=DIRECTION('center_axis',(-1.,0.,0.));
#25885=DIRECTION('ref_axis',(0.,1.,0.));
#25886=DIRECTION('',(1.,0.,0.));
#25887=DIRECTION('center_axis',(1.,0.,0.));
#25888=DIRECTION('ref_axis',(0.,-0.694184714467323,0.719796903438686));
#25889=DIRECTION('',(1.,0.,0.));
#25890=DIRECTION('center_axis',(1.,0.,0.));
#25891=DIRECTION('ref_axis',(0.,1.,0.));
#25892=DIRECTION('center_axis',(1.,0.,0.));
#25893=DIRECTION('ref_axis',(0.,0.,-1.));
#25894=DIRECTION('center_axis',(1.,0.,0.));
#25895=DIRECTION('ref_axis',(0.,1.,0.));
#25896=DIRECTION('center_axis',(1.,0.,0.));
#25897=DIRECTION('ref_axis',(0.,0.,-1.));
#25898=DIRECTION('center_axis',(-1.,0.,0.));
#25899=DIRECTION('ref_axis',(0.,1.,0.));
#25900=DIRECTION('',(1.,0.,0.));
#25901=DIRECTION('center_axis',(1.,0.,0.));
#25902=DIRECTION('ref_axis',(0.,-0.493369414448157,0.869819878415688));
#25903=DIRECTION('',(1.,0.,0.));
#25904=DIRECTION('center_axis',(1.,0.,0.));
#25905=DIRECTION('ref_axis',(0.,1.,0.));
#25906=DIRECTION('center_axis',(1.,0.,0.));
#25907=DIRECTION('ref_axis',(0.,0.,-1.));
#25908=DIRECTION('center_axis',(1.,0.,0.));
#25909=DIRECTION('ref_axis',(0.,1.,0.));
#25910=DIRECTION('center_axis',(1.,0.,0.));
#25911=DIRECTION('ref_axis',(0.,0.,-1.));
#25912=DIRECTION('center_axis',(-1.,0.,0.));
#25913=DIRECTION('ref_axis',(0.,1.,0.));
#25914=DIRECTION('',(1.,0.,0.));
#25915=DIRECTION('center_axis',(1.,0.,0.));
#25916=DIRECTION('ref_axis',(0.,-0.261553899633433,0.965188871458091));
#25917=DIRECTION('',(1.,0.,0.));
#25918=DIRECTION('center_axis',(1.,0.,0.));
#25919=DIRECTION('ref_axis',(0.,1.,0.));
#25920=DIRECTION('center_axis',(1.,0.,0.));
#25921=DIRECTION('ref_axis',(0.,0.,-1.));
#25922=DIRECTION('center_axis',(1.,0.,0.));
#25923=DIRECTION('ref_axis',(0.,1.,0.));
#25924=DIRECTION('center_axis',(1.,0.,0.));
#25925=DIRECTION('ref_axis',(0.,0.,-1.));
#25926=DIRECTION('center_axis',(-1.,0.,0.));
#25927=DIRECTION('ref_axis',(0.,1.,0.));
#25928=DIRECTION('',(1.,0.,0.));
#25929=DIRECTION('center_axis',(1.,0.,0.));
#25930=DIRECTION('ref_axis',(0.,-0.0133039913767846,0.99991149799042));
#25931=DIRECTION('',(1.,0.,0.));
#25932=DIRECTION('center_axis',(1.,0.,0.));
#25933=DIRECTION('ref_axis',(0.,1.,0.));
#25934=DIRECTION('center_axis',(1.,0.,0.));
#25935=DIRECTION('ref_axis',(0.,0.,-1.));
#25936=DIRECTION('center_axis',(1.,0.,0.));
#25937=DIRECTION('ref_axis',(0.,1.,0.));
#25938=DIRECTION('center_axis',(1.,0.,0.));
#25939=DIRECTION('ref_axis',(0.,0.,-1.));
#25940=DIRECTION('center_axis',(-1.,0.,0.));
#25941=DIRECTION('ref_axis',(0.,1.,0.));
#25942=DIRECTION('',(1.,0.,0.));
#25943=DIRECTION('center_axis',(1.,0.,0.));
#25944=DIRECTION('ref_axis',(0.,0.235781855586725,0.971806007686761));
#25945=DIRECTION('',(1.,0.,0.));
#25946=DIRECTION('center_axis',(1.,0.,0.));
#25947=DIRECTION('ref_axis',(0.,1.,0.));
#25948=DIRECTION('center_axis',(1.,0.,0.));
#25949=DIRECTION('ref_axis',(0.,0.,-1.));
#25950=DIRECTION('center_axis',(1.,0.,0.));
#25951=DIRECTION('ref_axis',(0.,1.,0.));
#25952=DIRECTION('center_axis',(1.,0.,0.));
#25953=DIRECTION('ref_axis',(0.,0.,-1.));
#25954=DIRECTION('center_axis',(-1.,0.,0.));
#25955=DIRECTION('ref_axis',(0.,1.,0.));
#25956=DIRECTION('',(1.,0.,0.));
#25957=DIRECTION('center_axis',(1.,0.,0.));
#25958=DIRECTION('ref_axis',(0.,0.470052661418713,0.882638371867655));
#25959=DIRECTION('',(1.,0.,0.));
#25960=DIRECTION('center_axis',(1.,0.,0.));
#25961=DIRECTION('ref_axis',(0.,1.,0.));
#25962=DIRECTION('center_axis',(1.,0.,0.));
#25963=DIRECTION('ref_axis',(0.,0.,-1.));
#25964=DIRECTION('center_axis',(1.,0.,0.));
#25965=DIRECTION('ref_axis',(0.,1.,0.));
#25966=DIRECTION('center_axis',(1.,0.,0.));
#25967=DIRECTION('ref_axis',(0.,0.,-1.));
#25968=DIRECTION('center_axis',(-1.,0.,0.));
#25969=DIRECTION('ref_axis',(0.,1.,0.));
#25970=DIRECTION('',(1.,0.,0.));
#25971=DIRECTION('center_axis',(1.,0.,0.));
#25972=DIRECTION('ref_axis',(0.,0.674788329801001,0.738011321027242));
#25973=DIRECTION('',(1.,0.,0.));
#25974=DIRECTION('center_axis',(1.,0.,0.));
#25975=DIRECTION('ref_axis',(0.,1.,0.));
#25976=DIRECTION('center_axis',(1.,0.,0.));
#25977=DIRECTION('ref_axis',(0.,0.,-1.));
#25978=DIRECTION('center_axis',(1.,0.,0.));
#25979=DIRECTION('ref_axis',(0.,1.,0.));
#25980=DIRECTION('center_axis',(1.,0.,0.));
#25981=DIRECTION('ref_axis',(0.,0.,-1.));
#25982=DIRECTION('center_axis',(-1.,0.,0.));
#25983=DIRECTION('ref_axis',(0.,1.,0.));
#25984=DIRECTION('',(1.,0.,0.));
#25985=DIRECTION('center_axis',(1.,0.,0.));
#25986=DIRECTION('ref_axis',(0.,0.837124565724013,0.547012304670911));
#25987=DIRECTION('',(1.,0.,0.));
#25988=DIRECTION('center_axis',(1.,0.,0.));
#25989=DIRECTION('ref_axis',(0.,1.,0.));
#25990=DIRECTION('center_axis',(1.,0.,0.));
#25991=DIRECTION('ref_axis',(0.,0.,-1.));
#25992=DIRECTION('center_axis',(1.,0.,0.));
#25993=DIRECTION('ref_axis',(0.,1.,0.));
#25994=DIRECTION('center_axis',(1.,0.,0.));
#25995=DIRECTION('ref_axis',(0.,0.,-1.));
#25996=DIRECTION('center_axis',(-1.,0.,0.));
#25997=DIRECTION('ref_axis',(0.,1.,0.));
#25998=DIRECTION('',(1.,0.,0.));
#25999=DIRECTION('center_axis',(1.,0.,0.));
#26000=DIRECTION('ref_axis',(0.,0.946861186453793,0.321642493441576));
#26001=DIRECTION('',(1.,0.,0.));
#26002=DIRECTION('center_axis',(1.,0.,0.));
#26003=DIRECTION('ref_axis',(0.,1.,0.));
#26004=DIRECTION('center_axis',(1.,0.,0.));
#26005=DIRECTION('ref_axis',(0.,0.,-1.));
#26006=DIRECTION('center_axis',(1.,0.,0.));
#26007=DIRECTION('ref_axis',(0.,1.,0.));
#26008=DIRECTION('center_axis',(1.,0.,0.));
#26009=DIRECTION('ref_axis',(0.,0.,-1.));
#26010=DIRECTION('center_axis',(-1.,0.,0.));
#26011=DIRECTION('ref_axis',(0.,1.,0.));
#26012=DIRECTION('',(1.,0.,0.));
#26013=DIRECTION('center_axis',(1.,0.,0.));
#26014=DIRECTION('ref_axis',(0.,0.99710303652683,0.0760627014309627));
#26015=DIRECTION('',(1.,0.,0.));
#26016=DIRECTION('center_axis',(1.,0.,0.));
#26017=DIRECTION('ref_axis',(0.,1.,0.));
#26018=DIRECTION('center_axis',(1.,0.,0.));
#26019=DIRECTION('ref_axis',(0.,0.,-1.));
#26020=DIRECTION('center_axis',(1.,0.,0.));
#26021=DIRECTION('ref_axis',(0.,1.,0.));
#26022=DIRECTION('center_axis',(1.,0.,0.));
#26023=DIRECTION('ref_axis',(0.,0.,-1.));
#26024=DIRECTION('center_axis',(-1.,0.,0.));
#26025=DIRECTION('ref_axis',(0.,1.,0.));
#26026=DIRECTION('center_axis',(1.,0.,0.));
#26027=DIRECTION('ref_axis',(0.,1.,0.));
#26028=DIRECTION('center_axis',(1.,0.,0.));
#26029=DIRECTION('ref_axis',(0.,0.,-1.));
#26030=DIRECTION('center_axis',(-1.,0.,0.));
#26031=DIRECTION('ref_axis',(0.,1.,0.));
#26032=DIRECTION('axis',(0.,0.,1.));
#26033=DIRECTION('refdir',(1.,0.,0.));
#26034=DIRECTION('center_axis',(1.,0.,0.));
#26035=DIRECTION('ref_axis',(0.,0.,-1.));
#26036=DIRECTION('center_axis',(-1.,0.,0.));
#26037=DIRECTION('ref_axis',(0.,-1.,1.83697019872103E-16));
#26038=DIRECTION('center_axis',(0.,-1.,-1.22464679914735E-16));
#26039=DIRECTION('ref_axis',(0.,-1.22464679914735E-16,1.));
#26040=DIRECTION('center_axis',(1.,0.,0.));
#26041=DIRECTION('ref_axis',(0.,-1.,3.06161699786838E-17));
#26042=DIRECTION('center_axis',(1.,0.,0.));
#26043=DIRECTION('ref_axis',(0.,-1.,3.06161699786838E-17));
#26044=DIRECTION('center_axis',(-1.,0.,0.));
#26045=DIRECTION('ref_axis',(0.,1.,0.));
#26046=DIRECTION('',(-0.707106781186548,-0.707106781186547,-8.65956056235493E-17));
#26047=DIRECTION('center_axis',(-1.,0.,0.));
#26048=DIRECTION('ref_axis',(0.,-1.,3.06161699786838E-17));
#26049=DIRECTION('center_axis',(-1.,0.,0.));
#26050=DIRECTION('ref_axis',(0.,-1.,3.06161699786838E-17));
#26051=DIRECTION('center_axis',(1.,0.,0.));
#26052=DIRECTION('ref_axis',(0.,0.,-1.));
#26053=DIRECTION('center_axis',(1.,0.,0.));
#26054=DIRECTION('ref_axis',(0.,0.,-1.));
#26055=DIRECTION('center_axis',(0.,-1.,-1.22464679914735E-16));
#26056=DIRECTION('ref_axis',(0.,-1.22464679914735E-16,1.));
#26057=DIRECTION('center_axis',(1.,0.,0.));
#26058=DIRECTION('ref_axis',(0.,-1.,1.83697019872103E-16));
#26059=DIRECTION('center_axis',(1.,0.,0.));
#26060=DIRECTION('ref_axis',(0.,-1.,1.83697019872103E-16));
#26061=DIRECTION('center_axis',(1.,0.,0.));
#26062=DIRECTION('ref_axis',(0.,1.,0.));
#26063=DIRECTION('',(-1.,0.,0.));
#26064=DIRECTION('center_axis',(-1.,0.,0.));
#26065=DIRECTION('ref_axis',(0.,-1.,1.83697019872103E-16));
#26066=DIRECTION('center_axis',(-1.,0.,0.));
#26067=DIRECTION('ref_axis',(0.,-1.,1.83697019872103E-16));
#26068=DIRECTION('center_axis',(1.,0.,0.));
#26069=DIRECTION('ref_axis',(0.,0.,-1.));
#26070=DIRECTION('center_axis',(0.,-1.,-1.22464679914735E-16));
#26071=DIRECTION('ref_axis',(0.,-1.22464679914735E-16,1.));
#26072=DIRECTION('center_axis',(1.,0.,0.));
#26073=DIRECTION('ref_axis',(0.,-1.,3.06161699786838E-17));
#26074=DIRECTION('center_axis',(1.,0.,0.));
#26075=DIRECTION('ref_axis',(0.,-1.,3.06161699786838E-17));
#26076=DIRECTION('center_axis',(1.,0.,0.));
#26077=DIRECTION('ref_axis',(0.,1.,0.));
#26078=DIRECTION('',(-0.707106781186556,0.707106781186539,8.65956056235483E-17));
#26079=DIRECTION('center_axis',(-1.,0.,0.));
#26080=DIRECTION('ref_axis',(0.,-1.,3.06161699786838E-17));
#26081=DIRECTION('center_axis',(-1.,0.,0.));
#26082=DIRECTION('ref_axis',(0.,-1.,3.06161699786838E-17));
#26083=DIRECTION('center_axis',(1.,0.,0.));
#26084=DIRECTION('ref_axis',(0.,0.,-1.));
#26085=DIRECTION('center_axis',(0.,-1.,-1.22464679914735E-16));
#26086=DIRECTION('ref_axis',(0.,-1.22464679914735E-16,1.));
#26087=DIRECTION('center_axis',(1.,0.,0.));
#26088=DIRECTION('ref_axis',(0.,-1.,1.83697019872103E-16));
#26089=DIRECTION('center_axis',(-1.,0.,0.));
#26090=DIRECTION('ref_axis',(0.,0.,1.));
#26091=DIRECTION('axis',(0.,0.,1.));
#26092=DIRECTION('refdir',(1.,0.,0.));
#26093=DIRECTION('center_axis',(0.,-1.,0.));
#26094=DIRECTION('ref_axis',(0.707106781186548,0.,0.707106781186547));
#26095=DIRECTION('center_axis',(0.,-1.,0.));
#26096=DIRECTION('ref_axis',(1.,0.,0.));
#26097=DIRECTION('',(0.,-1.,0.));
#26098=DIRECTION('center_axis',(0.,1.,0.));
#26099=DIRECTION('ref_axis',(0.,0.,1.));
#26100=DIRECTION('',(0.,1.,0.));
#26101=DIRECTION('center_axis',(1.,0.,0.));
#26102=DIRECTION('ref_axis',(0.,0.,-1.));
#26103=DIRECTION('center_axis',(0.,-1.,0.));
#26104=DIRECTION('ref_axis',(0.,0.,-1.));
#26105=DIRECTION('center_axis',(-1.,0.,0.));
#26106=DIRECTION('ref_axis',(0.,-1.,-6.12323399573677E-17));
#26107=DIRECTION('center_axis',(1.,0.,0.));
#26108=DIRECTION('ref_axis',(0.,-1.,-6.12323399573677E-17));
#26109=DIRECTION('center_axis',(0.,1.,0.));
#26110=DIRECTION('ref_axis',(0.707106781186548,0.,-0.707106781186547));
#26111=DIRECTION('center_axis',(0.,-1.,0.));
#26112=DIRECTION('ref_axis',(0.,0.,-1.));
#26113=DIRECTION('',(0.,-1.,0.));
#26114=DIRECTION('',(0.,1.,0.));
#26115=DIRECTION('center_axis',(1.,0.,0.));
#26116=DIRECTION('ref_axis',(0.,0.,-1.));
#26117=DIRECTION('center_axis',(-1.,0.,0.));
#26118=DIRECTION('ref_axis',(0.,1.,-6.12323399573677E-17));
#26119=DIRECTION('center_axis',(1.,0.,0.));
#26120=DIRECTION('ref_axis',(0.,1.,-6.12323399573677E-17));
#26121=DIRECTION('center_axis',(1.,0.,0.));
#26122=DIRECTION('ref_axis',(0.,0.,-1.));
#26123=DIRECTION('',(1.,0.,0.));
#26124=DIRECTION('center_axis',(-1.,0.,0.));
#26125=DIRECTION('ref_axis',(0.,-1.,-6.12323399573677E-17));
#26126=DIRECTION('',(1.,0.,0.));
#26127=DIRECTION('center_axis',(0.,0.,1.));
#26128=DIRECTION('ref_axis',(0.,-1.,0.));
#26129=DIRECTION('',(1.,0.,0.));
#26130=DIRECTION('',(0.,1.,0.));
#26131=DIRECTION('center_axis',(1.,0.,0.));
#26132=DIRECTION('ref_axis',(0.,0.,-1.));
#26133=DIRECTION('center_axis',(1.,0.,0.));
#26134=DIRECTION('ref_axis',(0.,0.,-1.));
#26135=DIRECTION('center_axis',(0.,1.,0.));
#26136=DIRECTION('ref_axis',(-0.707106781186548,0.,0.707106781186547));
#26137=DIRECTION('center_axis',(0.,1.,0.));
#26138=DIRECTION('ref_axis',(-1.,0.,0.));
#26139=DIRECTION('center_axis',(0.,-1.,0.));
#26140=DIRECTION('ref_axis',(0.,0.,1.));
#26141=DIRECTION('',(0.,-1.,0.));
#26142=DIRECTION('center_axis',(1.,0.,0.));
#26143=DIRECTION('ref_axis',(0.,0.,-1.));
#26144=DIRECTION('center_axis',(0.,1.,0.));
#26145=DIRECTION('ref_axis',(0.,0.,-1.));
#26146=DIRECTION('center_axis',(1.,0.,0.));
#26147=DIRECTION('ref_axis',(0.,1.,-6.12323399573677E-17));
#26148=DIRECTION('center_axis',(-1.,0.,0.));
#26149=DIRECTION('ref_axis',(0.,1.,-6.12323399573677E-17));
#26150=DIRECTION('center_axis',(0.,-1.,0.));
#26151=DIRECTION('ref_axis',(-0.707106781186548,0.,-0.707106781186547));
#26152=DIRECTION('center_axis',(0.,1.,0.));
#26153=DIRECTION('ref_axis',(0.,0.,-1.));
#26154=DIRECTION('',(0.,1.,0.));
#26155=DIRECTION('',(0.,-1.,0.));
#26156=DIRECTION('center_axis',(1.,0.,0.));
#26157=DIRECTION('ref_axis',(0.,0.,-1.));
#26158=DIRECTION('center_axis',(1.,0.,0.));
#26159=DIRECTION('ref_axis',(0.,-1.,-6.12323399573677E-17));
#26160=DIRECTION('center_axis',(1.,0.,0.));
#26161=DIRECTION('ref_axis',(0.,0.,-1.));
#26162=DIRECTION('',(1.,0.,0.));
#26163=DIRECTION('center_axis',(1.,0.,0.));
#26164=DIRECTION('ref_axis',(0.,0.,-1.));
#26165=DIRECTION('center_axis',(-1.,0.,0.));
#26166=DIRECTION('ref_axis',(0.,0.,-1.));
#26167=DIRECTION('center_axis',(1.,0.,0.));
#26168=DIRECTION('ref_axis',(0.,0.,-1.));
#26169=DIRECTION('center_axis',(0.,-1.,-1.22464679914735E-16));
#26170=DIRECTION('ref_axis',(0.,-1.22464679914735E-16,1.));
#26171=DIRECTION('center_axis',(1.,0.,0.));
#26172=DIRECTION('ref_axis',(0.,0.,-1.));
#26173=DIRECTION('center_axis',(1.,0.,0.));
#26174=DIRECTION('ref_axis',(0.,0.,-1.));
#26175=DIRECTION('',(1.,0.,0.));
#26176=DIRECTION('center_axis',(-1.,0.,0.));
#26177=DIRECTION('ref_axis',(0.,0.,-1.));
#26178=DIRECTION('center_axis',(-1.,0.,0.));
#26179=DIRECTION('ref_axis',(0.,0.,-1.));
#26180=DIRECTION('center_axis',(-1.,0.,0.));
#26181=DIRECTION('ref_axis',(0.,0.,1.));
#26182=DIRECTION('center_axis',(0.,-1.,1.22464679914735E-16));
#26183=DIRECTION('ref_axis',(0.,-1.22464679914735E-16,-1.));
#26184=DIRECTION('center_axis',(0.,0.,-1.));
#26185=DIRECTION('ref_axis',(0.,1.,0.));
#26186=DIRECTION('axis',(0.,0.,1.));
#26187=DIRECTION('refdir',(1.,0.,0.));
#26188=DIRECTION('center_axis',(1.,0.,0.));
#26189=DIRECTION('ref_axis',(0.,0.,-1.));
#26190=DIRECTION('center_axis',(-1.,0.,0.));
#26191=DIRECTION('ref_axis',(0.,-1.,1.83697019872103E-16));
#26192=DIRECTION('center_axis',(0.,-1.,-1.22464679914735E-16));
#26193=DIRECTION('ref_axis',(0.,-1.22464679914735E-16,1.));
#26194=DIRECTION('center_axis',(1.,0.,0.));
#26195=DIRECTION('ref_axis',(0.,-1.,3.06161699786838E-17));
#26196=DIRECTION('center_axis',(1.,0.,0.));
#26197=DIRECTION('ref_axis',(0.,-1.,3.06161699786838E-17));
#26198=DIRECTION('center_axis',(-1.,0.,0.));
#26199=DIRECTION('ref_axis',(0.,1.,0.));
#26200=DIRECTION('',(-0.707106781186548,-0.707106781186547,-8.65956056235493E-17));
#26201=DIRECTION('center_axis',(-1.,0.,0.));
#26202=DIRECTION('ref_axis',(0.,-1.,3.06161699786838E-17));
#26203=DIRECTION('center_axis',(-1.,0.,0.));
#26204=DIRECTION('ref_axis',(0.,-1.,3.06161699786838E-17));
#26205=DIRECTION('center_axis',(1.,0.,0.));
#26206=DIRECTION('ref_axis',(0.,0.,-1.));
#26207=DIRECTION('center_axis',(1.,0.,0.));
#26208=DIRECTION('ref_axis',(0.,0.,-1.));
#26209=DIRECTION('center_axis',(0.,-1.,-1.22464679914735E-16));
#26210=DIRECTION('ref_axis',(0.,-1.22464679914735E-16,1.));
#26211=DIRECTION('center_axis',(1.,0.,0.));
#26212=DIRECTION('ref_axis',(0.,-1.,1.83697019872103E-16));
#26213=DIRECTION('center_axis',(1.,0.,0.));
#26214=DIRECTION('ref_axis',(0.,-1.,1.83697019872103E-16));
#26215=DIRECTION('center_axis',(1.,0.,0.));
#26216=DIRECTION('ref_axis',(0.,1.,0.));
#26217=DIRECTION('',(-1.,0.,0.));
#26218=DIRECTION('center_axis',(-1.,0.,0.));
#26219=DIRECTION('ref_axis',(0.,-1.,1.83697019872103E-16));
#26220=DIRECTION('center_axis',(-1.,0.,0.));
#26221=DIRECTION('ref_axis',(0.,-1.,1.83697019872103E-16));
#26222=DIRECTION('center_axis',(1.,0.,0.));
#26223=DIRECTION('ref_axis',(0.,0.,-1.));
#26224=DIRECTION('center_axis',(0.,-1.,-1.22464679914735E-16));
#26225=DIRECTION('ref_axis',(0.,-1.22464679914735E-16,1.));
#26226=DIRECTION('center_axis',(1.,0.,0.));
#26227=DIRECTION('ref_axis',(0.,-1.,3.06161699786838E-17));
#26228=DIRECTION('center_axis',(1.,0.,0.));
#26229=DIRECTION('ref_axis',(0.,-1.,3.06161699786838E-17));
#26230=DIRECTION('center_axis',(1.,0.,0.));
#26231=DIRECTION('ref_axis',(0.,1.,0.));
#26232=DIRECTION('',(-0.707106781186547,0.707106781186547,8.65956056235493E-17));
#26233=DIRECTION('center_axis',(-1.,0.,0.));
#26234=DIRECTION('ref_axis',(0.,-1.,3.06161699786838E-17));
#26235=DIRECTION('center_axis',(-1.,0.,0.));
#26236=DIRECTION('ref_axis',(0.,-1.,3.06161699786838E-17));
#26237=DIRECTION('center_axis',(1.,0.,0.));
#26238=DIRECTION('ref_axis',(0.,0.,-1.));
#26239=DIRECTION('center_axis',(0.,-1.,-1.22464679914735E-16));
#26240=DIRECTION('ref_axis',(0.,-1.22464679914735E-16,1.));
#26241=DIRECTION('center_axis',(1.,0.,0.));
#26242=DIRECTION('ref_axis',(0.,-1.,1.83697019872103E-16));
#26243=DIRECTION('center_axis',(-1.,0.,0.));
#26244=DIRECTION('ref_axis',(0.,0.,1.));
#26245=DIRECTION('axis',(0.,0.,1.));
#26246=DIRECTION('refdir',(1.,0.,0.));
#26247=DIRECTION('center_axis',(1.,0.,0.));
#26248=DIRECTION('ref_axis',(0.,-0.984807753012208,0.17364817766693));
#26249=DIRECTION('center_axis',(0.,0.342020143325669,0.939692620785908));
#26250=DIRECTION('ref_axis',(1.,0.,0.));
#26251=DIRECTION('center_axis',(-1.,0.,0.));
#26252=DIRECTION('ref_axis',(0.,-0.984807753012208,0.17364817766693));
#26253=DIRECTION('center_axis',(0.,0.,1.));
#26254=DIRECTION('ref_axis',(1.,0.,0.));
#26255=DIRECTION('center_axis',(0.,0.342020143325669,0.939692620785908));
#26256=DIRECTION('ref_axis',(1.,0.,0.));
#26257=DIRECTION('center_axis',(0.,0.,1.));
#26258=DIRECTION('ref_axis',(1.,0.,0.));
#26259=DIRECTION('axis',(0.,0.,1.));
#26260=DIRECTION('refdir',(1.,0.,0.));
#26261=DIRECTION('center_axis',(0.,-1.,1.63268091856641E-16));
#26262=DIRECTION('ref_axis',(-0.707106781186548,0.,0.707106781186548));
#26263=DIRECTION('',(0.,-1.,1.63268091856641E-16));
#26264=DIRECTION('center_axis',(0.,1.,0.));
#26265=DIRECTION('ref_axis',(-1.,0.,0.));
#26266=DIRECTION('',(0.,1.,-1.63268091856641E-16));
#26267=DIRECTION('center_axis',(-0.707106781186548,-0.707106781186548,0.));
#26268=DIRECTION('ref_axis',(-0.707106781186548,0.707106781186548,-1.2266347333467E-16));
#26269=DIRECTION('',(0.,1.,-1.63268091856641E-16));
#26270=DIRECTION('center_axis',(0.,0.,-1.));
#26271=DIRECTION('ref_axis',(-0.707106781186548,-0.707106781186548,0.));
#26272=DIRECTION('',(0.,0.,1.));
#26273=DIRECTION('center_axis',(0.,0.,-1.));
#26274=DIRECTION('ref_axis',(0.,-1.,0.));
#26275=DIRECTION('',(0.,0.,-1.));
#26276=DIRECTION('center_axis',(-0.707106781186548,0.,0.707106781186548));
#26277=DIRECTION('ref_axis',(0.707106781186547,0.,0.707106781186547));
#26278=DIRECTION('center_axis',(-0.408248290463863,-0.816496580927726,0.408248290463863));
#26279=DIRECTION('ref_axis',(0.577350269189627,-0.577350269189623,-0.577350269189628));
#26280=DIRECTION('center_axis',(0.,0.,-1.));
#26281=DIRECTION('ref_axis',(0.,-1.,0.));
#26282=DIRECTION('center_axis',(1.,0.,0.));
#26283=DIRECTION('ref_axis',(0.,0.,-1.));
#26284=DIRECTION('center_axis',(0.,-1.,0.));
#26285=DIRECTION('ref_axis',(1.,0.,0.));
#26286=DIRECTION('center_axis',(1.,0.,0.));
#26287=DIRECTION('ref_axis',(0.,-0.707106781186548,-0.707106781186548));
#26288=DIRECTION('',(1.,0.,0.));
#26289=DIRECTION('',(-1.,0.,0.));
#26290=DIRECTION('center_axis',(0.,1.,-1.63268091856641E-16));
#26291=DIRECTION('ref_axis',(0.707106781186548,0.,-0.707106781186548));
#26292=DIRECTION('center_axis',(0.,-1.,0.));
#26293=DIRECTION('ref_axis',(0.,0.,-1.));
#26294=DIRECTION('',(0.,-1.,1.63268091856641E-16));
#26295=DIRECTION('',(0.,1.,-1.63268091856641E-16));
#26296=DIRECTION('center_axis',(0.408248290463861,-0.816496580927727,-0.408248290463863));
#26297=DIRECTION('ref_axis',(0.577350269189626,0.577350269189624,-0.577350269189628));
#26298=DIRECTION('center_axis',(1.,0.,0.));
#26299=DIRECTION('ref_axis',(0.,0.707106781186546,-0.707106781186549));
#26300=DIRECTION('center_axis',(0.,0.,-1.));
#26301=DIRECTION('ref_axis',(0.707106781186549,0.707106781186546,0.));
#26302=DIRECTION('center_axis',(-0.408248290463861,-0.816496580927727,-0.408248290463863));
#26303=DIRECTION('ref_axis',(0.577350269189626,-0.577350269189624,0.577350269189628));
#26304=DIRECTION('center_axis',(-1.38777878078145E-15,0.,1.));
#26305=DIRECTION('ref_axis',(0.,-1.,0.));
#26306=DIRECTION('center_axis',(0.,-1.,1.63268091856641E-16));
#26307=DIRECTION('ref_axis',(0.707106781186548,0.,0.707106781186548));
#26308=DIRECTION('center_axis',(1.,0.,0.));
#26309=DIRECTION('ref_axis',(0.,-0.707106781186549,0.707106781186546));
#26310=DIRECTION('center_axis',(0.,0.,-1.));
#26311=DIRECTION('ref_axis',(0.707106781186548,-0.707106781186548,0.));
#26312=DIRECTION('',(0.,0.,-1.));
#26313=DIRECTION('',(0.,0.,1.));
#26314=DIRECTION('center_axis',(0.408248290463861,-0.816496580927727,-0.408248290463862));
#26315=DIRECTION('ref_axis',(-0.577350269189626,-0.577350269189624,0.577350269189627));
#26316=DIRECTION('center_axis',(-1.,0.,0.));
#26317=DIRECTION('ref_axis',(0.,-0.707106781186549,0.707106781186546));
#26318=DIRECTION('center_axis',(1.,0.,0.));
#26319=DIRECTION('ref_axis',(0.,0.707106781186548,0.707106781186548));
#26320=DIRECTION('',(1.,0.,0.));
#26321=DIRECTION('center_axis',(1.,0.,0.));
#26322=DIRECTION('ref_axis',(0.,0.,1.));
#26323=DIRECTION('',(-1.,0.,0.));
#26324=DIRECTION('center_axis',(-1.,0.,0.));
#26325=DIRECTION('ref_axis',(0.,0.707106781186548,0.707106781186548));
#26326=DIRECTION('center_axis',(0.,1.63268091856641E-16,1.));
#26327=DIRECTION('ref_axis',(0.,-1.,1.63268091856641E-16));
#26328=DIRECTION('',(-1.,0.,0.));
#26329=DIRECTION('',(0.,-1.,1.63268091856641E-16));
#26330=DIRECTION('center_axis',(0.,-1.,0.));
#26331=DIRECTION('ref_axis',(0.,0.,-1.));
#26332=DIRECTION('',(1.,0.,0.));
#26333=DIRECTION('center_axis',(1.,0.,0.));
#26334=DIRECTION('ref_axis',(0.,-0.707106781186548,0.707106781186548));
#26335=DIRECTION('center_axis',(1.,0.,0.));
#26336=DIRECTION('ref_axis',(0.,0.707106781186548,-0.707106781186548));
#26337=DIRECTION('',(-1.,0.,0.));
#26338=DIRECTION('center_axis',(-1.,0.,0.));
#26339=DIRECTION('ref_axis',(0.,0.707106781186548,-0.707106781186548));
#26340=DIRECTION('',(1.,0.,0.));
#26341=DIRECTION('center_axis',(-0.816496580927727,0.40824829046386,0.408248290463864));
#26342=DIRECTION('ref_axis',(0.577350269189627,0.577350269189624,0.577350269189627));
#26343=DIRECTION('center_axis',(0.,0.,1.));
#26344=DIRECTION('ref_axis',(0.,1.,0.));
#26345=DIRECTION('center_axis',(0.,1.,0.));
#26346=DIRECTION('ref_axis',(1.,0.,0.));
#26347=DIRECTION('center_axis',(0.,-1.,1.63268091856641E-16));
#26348=DIRECTION('ref_axis',(0.707106781186548,0.,0.707106781186548));
#26349=DIRECTION('',(0.,1.,-1.63268091856641E-16));
#26350=DIRECTION('center_axis',(0.,0.,1.));
#26351=DIRECTION('ref_axis',(0.707106781186548,0.707106781186548,0.));
#26352=DIRECTION('',(0.,0.,1.));
#26353=DIRECTION('',(0.,0.,-1.));
#26354=DIRECTION('center_axis',(1.,0.,0.));
#26355=DIRECTION('ref_axis',(0.,0.,-1.));
#26356=DIRECTION('center_axis',(1.,0.,0.));
#26357=DIRECTION('ref_axis',(0.,0.,-1.));
#26358=DIRECTION('center_axis',(1.,0.,0.));
#26359=DIRECTION('ref_axis',(0.,0.,-1.));
#26360=DIRECTION('',(0.,1.,-1.63268091856641E-16));
#26361=DIRECTION('center_axis',(0.,0.,1.));
#26362=DIRECTION('ref_axis',(-0.707106781186548,0.707106781186548,0.));
#26363=DIRECTION('',(0.,0.,1.));
#26364=DIRECTION('center_axis',(0.,0.,-1.));
#26365=DIRECTION('ref_axis',(-1.,0.,0.));
#26366=DIRECTION('',(0.,0.,-1.));
#26367=DIRECTION('center_axis',(-0.707106781186548,0.,0.707106781186548));
#26368=DIRECTION('ref_axis',(-0.707106781186547,0.,-0.707106781186547));
#26369=DIRECTION('',(0.,0.,-1.));
#26370=DIRECTION('center_axis',(0.,-1.,0.));
#26371=DIRECTION('ref_axis',(0.707106781186548,0.,0.707106781186548));
#26372=DIRECTION('center_axis',(0.,1.,0.));
#26373=DIRECTION('ref_axis',(0.,0.,1.));
#26374=DIRECTION('',(0.,1.,0.));
#26375=DIRECTION('center_axis',(0.,-1.,0.));
#26376=DIRECTION('ref_axis',(1.,0.,0.));
#26377=DIRECTION('',(0.,-1.,0.));
#26378=DIRECTION('center_axis',(0.408248290463864,-0.816496580927727,0.40824829046386));
#26379=DIRECTION('ref_axis',(0.577350269189626,0.577350269189627,0.577350269189624));
#26380=DIRECTION('center_axis',(0.,0.,1.));
#26381=DIRECTION('ref_axis',(0.707106781186548,0.707106781186548,0.));
#26382=DIRECTION('center_axis',(1.,0.,0.));
#26383=DIRECTION('ref_axis',(0.,0.707106781186546,0.707106781186549));
#26384=DIRECTION('center_axis',(0.,-1.,0.));
#26385=DIRECTION('ref_axis',(-0.707106781186548,0.,0.707106781186548));
#26386=DIRECTION('',(0.,1.,0.));
#26387=DIRECTION('center_axis',(0.,-1.,0.));
#26388=DIRECTION('ref_axis',(0.,0.,1.));
#26389=DIRECTION('',(0.,-1.,0.));
#26390=DIRECTION('center_axis',(-0.707106781186547,0.707106781186548,0.));
#26391=DIRECTION('ref_axis',(0.707106781186548,0.707106781186547,0.));
#26392=DIRECTION('center_axis',(1.,0.,0.));
#26393=DIRECTION('ref_axis',(0.,-0.707106781186548,0.707106781186548));
#26394=DIRECTION('',(1.,0.,0.));
#26395=DIRECTION('center_axis',(-1.,0.,0.));
#26396=DIRECTION('ref_axis',(0.,-1.,0.));
#26397=DIRECTION('',(-1.,0.,0.));
#26398=DIRECTION('center_axis',(-0.408248290463863,-0.816496580927727,-0.40824829046386));
#26399=DIRECTION('ref_axis',(0.577350269189627,-0.577350269189627,0.577350269189624));
#26400=DIRECTION('center_axis',(0.,0.,1.));
#26401=DIRECTION('ref_axis',(0.707106781186548,-0.707106781186548,0.));
#26402=DIRECTION('center_axis',(-0.408248290463865,-0.816496580927727,0.40824829046386));
#26403=DIRECTION('ref_axis',(-0.577350269189626,0.577350269189627,0.577350269189624));
#26404=DIRECTION('center_axis',(-1.,0.,0.));
#26405=DIRECTION('ref_axis',(0.,0.707106781186546,0.707106781186549));
#26406=DIRECTION('center_axis',(1.,0.,0.));
#26407=DIRECTION('ref_axis',(0.,0.707106781186548,-0.707106781186548));
#26408=DIRECTION('',(1.,0.,0.));
#26409=DIRECTION('center_axis',(1.,0.,0.));
#26410=DIRECTION('ref_axis',(0.,1.,0.));
#26411=DIRECTION('',(-1.,0.,0.));
#26412=DIRECTION('center_axis',(-1.,0.,0.));
#26413=DIRECTION('ref_axis',(0.,0.707106781186548,-0.707106781186548));
#26414=DIRECTION('center_axis',(0.,1.,0.));
#26415=DIRECTION('ref_axis',(0.,0.,1.));
#26416=DIRECTION('',(-1.,0.,0.));
#26417=DIRECTION('',(0.,0.,1.));
#26418=DIRECTION('center_axis',(1.,0.,0.));
#26419=DIRECTION('ref_axis',(0.,0.707106781186548,0.707106781186548));
#26420=DIRECTION('',(1.,0.,0.));
#26421=DIRECTION('center_axis',(-0.408248290463864,-0.816496580927727,0.40824829046386));
#26422=DIRECTION('ref_axis',(0.577350269189627,-0.577350269189627,-0.577350269189624));
#26423=DIRECTION('center_axis',(0.,0.,-1.));
#26424=DIRECTION('ref_axis',(0.,-1.,0.));
#26425=DIRECTION('center_axis',(1.,0.,0.));
#26426=DIRECTION('ref_axis',(0.,0.,-1.));
#26427=DIRECTION('center_axis',(0.,-1.,0.));
#26428=DIRECTION('ref_axis',(1.,0.,0.));
#26429=DIRECTION('center_axis',(1.,0.,0.));
#26430=DIRECTION('ref_axis',(0.,-0.707106781186548,-0.707106781186548));
#26431=DIRECTION('center_axis',(-1.,0.,0.));
#26432=DIRECTION('ref_axis',(0.,-0.707106781186548,-0.707106781186548));
#26433=DIRECTION('',(1.,0.,0.));
#26434=DIRECTION('',(-1.,0.,0.));
#26435=DIRECTION('center_axis',(0.408248290463863,-0.816496580927727,-0.40824829046386));
#26436=DIRECTION('ref_axis',(0.577350269189627,0.577350269189628,-0.577350269189623));
#26437=DIRECTION('center_axis',(0.,1.,0.));
#26438=DIRECTION('ref_axis',(0.,0.,-1.));
#26439=DIRECTION('center_axis',(0.,0.,-1.));
#26440=DIRECTION('ref_axis',(1.,0.,0.));
#26441=DIRECTION('center_axis',(0.,0.,1.));
#26442=DIRECTION('ref_axis',(0.707106781186548,0.707106781186548,0.));
#26443=DIRECTION('',(0.,0.,-1.));
#26444=DIRECTION('center_axis',(0.,1.,0.));
#26445=DIRECTION('ref_axis',(0.707106781186548,0.,-0.707106781186548));
#26446=DIRECTION('',(0.,-1.,0.));
#26447=DIRECTION('',(0.,1.,0.));
#26448=DIRECTION('center_axis',(0.,0.,-1.));
#26449=DIRECTION('ref_axis',(0.707106781186548,-0.707106781186548,0.));
#26450=DIRECTION('',(0.,0.,-1.));
#26451=DIRECTION('',(0.,0.,1.));
#26452=DIRECTION('center_axis',(1.,0.,0.));
#26453=DIRECTION('ref_axis',(0.,0.,-1.));
#26454=DIRECTION('center_axis',(1.,0.,0.));
#26455=DIRECTION('ref_axis',(0.,0.,-1.));
#26456=DIRECTION('center_axis',(1.,0.,0.));
#26457=DIRECTION('ref_axis',(0.,0.,-1.));
#26458=DIRECTION('center_axis',(1.,0.,0.));
#26459=DIRECTION('ref_axis',(0.,0.,-1.));
#26460=DIRECTION('',(0.,0.,-1.));
#26461=DIRECTION('center_axis',(0.,0.,1.));
#26462=DIRECTION('ref_axis',(0.707106781186548,0.707106781186548,0.));
#26463=DIRECTION('center_axis',(0.,0.,1.));
#26464=DIRECTION('ref_axis',(1.,0.,0.));
#26465=DIRECTION('',(0.,0.,1.));
#26466=DIRECTION('center_axis',(0.,0.,-1.));
#26467=DIRECTION('ref_axis',(0.,1.,0.));
#26468=DIRECTION('',(0.,0.,-1.));
#26469=DIRECTION('center_axis',(-0.816496580927727,0.40824829046386,0.408248290463864));
#26470=DIRECTION('ref_axis',(0.577350269189627,0.577350269189624,0.577350269189627));
#26471=DIRECTION('center_axis',(1.,0.,0.));
#26472=DIRECTION('ref_axis',(0.,0.707106781186549,0.707106781186546));
#26473=DIRECTION('center_axis',(0.,1.,0.));
#26474=DIRECTION('ref_axis',(0.707106781186548,0.,0.707106781186548));
#26475=DIRECTION('center_axis',(-0.816496580927727,0.40824829046386,-0.408248290463864));
#26476=DIRECTION('ref_axis',(0.577350269189627,0.577350269189624,-0.577350269189627));
#26477=DIRECTION('center_axis',(0.,1.,0.));
#26478=DIRECTION('ref_axis',(0.707106781186548,0.,-0.707106781186548));
#26479=DIRECTION('center_axis',(1.,0.,0.));
#26480=DIRECTION('ref_axis',(0.,0.707106781186549,-0.707106781186546));
#26481=DIRECTION('center_axis',(1.,0.,0.));
#26482=DIRECTION('ref_axis',(0.,0.707106781186548,-0.707106781186548));
#26483=DIRECTION('',(-1.,0.,0.));
#26484=DIRECTION('center_axis',(-1.,0.,0.));
#26485=DIRECTION('ref_axis',(0.,0.707106781186549,-0.707106781186546));
#26486=DIRECTION('',(1.,0.,0.));
#26487=DIRECTION('center_axis',(0.,1.,0.));
#26488=DIRECTION('ref_axis',(0.707106781186548,0.,-0.707106781186548));
#26489=DIRECTION('',(0.,-1.,0.));
#26490=DIRECTION('center_axis',(0.,1.,0.));
#26491=DIRECTION('ref_axis',(1.,0.,0.));
#26492=DIRECTION('',(0.,1.,0.));
#26493=DIRECTION('center_axis',(1.,0.,0.));
#26494=DIRECTION('ref_axis',(0.,0.,-1.));
#26495=DIRECTION('',(0.,1.,0.));
#26496=DIRECTION('',(0.,0.,1.));
#26497=DIRECTION('center_axis',(0.,1.,0.));
#26498=DIRECTION('ref_axis',(-0.707106781186548,0.,-0.707106781186548));
#26499=DIRECTION('',(0.,1.,0.));
#26500=DIRECTION('center_axis',(0.,-1.,0.));
#26501=DIRECTION('ref_axis',(-1.,0.,0.));
#26502=DIRECTION('',(0.,-1.,0.));
#26503=DIRECTION('center_axis',(-0.707106781186548,0.707106781186548,0.));
#26504=DIRECTION('ref_axis',(-0.707106781186547,-0.707106781186547,0.));
#26505=DIRECTION('',(0.,-1.,0.));
#26506=DIRECTION('center_axis',(0.,0.,1.));
#26507=DIRECTION('ref_axis',(-0.707106781186548,0.707106781186548,0.));
#26508=DIRECTION('center_axis',(0.,0.,1.));
#26509=DIRECTION('ref_axis',(0.,1.,0.));
#26510=DIRECTION('',(0.,0.,1.));
#26511=DIRECTION('center_axis',(0.,0.,-1.));
#26512=DIRECTION('ref_axis',(-1.,0.,0.));
#26513=DIRECTION('',(0.,0.,-1.));
#26514=DIRECTION('center_axis',(0.,-1.,0.));
#26515=DIRECTION('ref_axis',(-0.707106781186548,0.,0.707106781186548));
#26516=DIRECTION('center_axis',(-0.707106781186548,0.707106781186548,0.));
#26517=DIRECTION('ref_axis',(-0.707106781186547,-0.707106781186547,0.));
#26518=DIRECTION('',(0.,1.,0.));
#26519=DIRECTION('center_axis',(0.,-1.,0.));
#26520=DIRECTION('ref_axis',(0.,0.,1.));
#26521=DIRECTION('',(0.,-1.,0.));
#26522=DIRECTION('',(0.,1.,0.));
#26523=DIRECTION('center_axis',(-0.816496580927727,-0.40824829046386,-0.408248290463864));
#26524=DIRECTION('ref_axis',(-0.577350269189628,0.577350269189623,0.577350269189627));
#26525=DIRECTION('center_axis',(-1.,0.,0.));
#26526=DIRECTION('ref_axis',(0.,0.707106781186549,0.707106781186546));
#26527=DIRECTION('center_axis',(-0.816496580927727,-0.40824829046386,0.408248290463864));
#26528=DIRECTION('ref_axis',(-0.577350269189628,0.577350269189623,-0.577350269189627));
#26529=DIRECTION('center_axis',(1.,0.,0.));
#26530=DIRECTION('ref_axis',(0.,-0.707106781186548,-0.707106781186548));
#26531=DIRECTION('',(1.,0.,0.));
#26532=DIRECTION('center_axis',(1.,0.,0.));
#26533=DIRECTION('ref_axis',(0.,-0.707106781186546,-0.707106781186549));
#26534=DIRECTION('',(-1.,0.,0.));
#26535=DIRECTION('center_axis',(-1.,0.,0.));
#26536=DIRECTION('ref_axis',(0.,-0.707106781186548,-0.707106781186548));
#26537=DIRECTION('center_axis',(0.,0.,-1.));
#26538=DIRECTION('ref_axis',(0.,1.,0.));
#26539=DIRECTION('center_axis',(0.,1.,0.));
#26540=DIRECTION('ref_axis',(0.,0.,1.));
#26541=DIRECTION('',(-1.,0.,0.));
#26542=DIRECTION('center_axis',(1.,0.,0.));
#26543=DIRECTION('ref_axis',(0.,0.707106781186548,0.707106781186548));
#26544=DIRECTION('',(1.,0.,0.));
#26545=DIRECTION('center_axis',(0.,0.,1.));
#26546=DIRECTION('ref_axis',(0.,-1.,0.));
#26547=DIRECTION('',(-1.,0.,0.));
#26548=DIRECTION('',(0.,-1.,0.));
#26549=DIRECTION('center_axis',(1.,0.,0.));
#26550=DIRECTION('ref_axis',(0.,-0.707106781186548,0.707106781186548));
#26551=DIRECTION('center_axis',(-1.,0.,0.));
#26552=DIRECTION('ref_axis',(0.,-0.707106781186548,0.707106781186548));
#26553=DIRECTION('',(1.,0.,0.));
#26554=DIRECTION('center_axis',(1.,0.,0.));
#26555=DIRECTION('ref_axis',(0.,-1.,0.));
#26556=DIRECTION('center_axis',(1.,0.,0.));
#26557=DIRECTION('ref_axis',(0.,0.,-1.));
#26558=DIRECTION('center_axis',(0.,-1.,-1.22464679914735E-16));
#26559=DIRECTION('ref_axis',(0.,-1.22464679914735E-16,1.));
#26560=DIRECTION('center_axis',(1.,-3.67724725538251E-17,-3.65371805748965E-17));
#26561=DIRECTION('ref_axis',(0.,0.704833646806666,-0.709372631505625));
#26562=DIRECTION('center_axis',(1.,-3.67724725538251E-17,-3.65371805748965E-17));
#26563=DIRECTION('ref_axis',(0.,0.704833646806666,-0.709372631505625));
#26564=DIRECTION('center_axis',(1.,0.,0.));
#26565=DIRECTION('ref_axis',(0.,0.,-1.));
#26566=DIRECTION('center_axis',(1.,0.,0.));
#26567=DIRECTION('ref_axis',(0.,0.,-1.));
#26568=DIRECTION('center_axis',(1.,0.,0.));
#26569=DIRECTION('ref_axis',(0.,0.,-1.));
#26570=DIRECTION('center_axis',(1.,0.,0.));
#26571=DIRECTION('ref_axis',(0.,0.,-1.));
#26572=DIRECTION('center_axis',(-1.,0.,0.));
#26573=DIRECTION('ref_axis',(0.,0.704833646806666,-0.709372631505625));
#26574=DIRECTION('center_axis',(1.,0.,0.));
#26575=DIRECTION('ref_axis',(0.,0.,-1.));
#26576=DIRECTION('center_axis',(1.,0.,0.));
#26577=DIRECTION('ref_axis',(0.,0.,-1.));
#26578=DIRECTION('',(0.,0.,1.));
#26579=DIRECTION('center_axis',(-1.,0.,0.));
#26580=DIRECTION('ref_axis',(0.,-0.707106781186548,0.707106781186548));
#26581=DIRECTION('',(0.,1.,0.));
#26582=DIRECTION('center_axis',(-1.,0.,0.));
#26583=DIRECTION('ref_axis',(0.,0.707106781186548,0.707106781186548));
#26584=DIRECTION('',(0.,-1.63268091856641E-16,-1.));
#26585=DIRECTION('',(0.,0.,1.));
#26586=DIRECTION('',(0.,-1.,0.));
#26587=DIRECTION('',(0.,0.,1.));
#26588=DIRECTION('',(0.,0.,-1.));
#26589=DIRECTION('',(0.,-1.,1.63268091856641E-16));
#26590=DIRECTION('center_axis',(1.,0.,0.));
#26591=DIRECTION('ref_axis',(0.,1.,-1.82855839818329E-16));
#26592=DIRECTION('center_axis',(-1.,0.,0.));
#26593=DIRECTION('ref_axis',(0.,1.,0.));
#26594=DIRECTION('',(-0.707106781186546,-0.707106781186549,-8.65956056235495E-17));
#26595=DIRECTION('center_axis',(-1.,0.,0.));
#26596=DIRECTION('ref_axis',(0.,-1.,3.06161699786838E-17));
#26597=DIRECTION('center_axis',(-1.,0.,0.));
#26598=DIRECTION('ref_axis',(0.,-1.,3.06161699786838E-17));
#26599=DIRECTION('center_axis',(1.,0.,0.));
#26600=DIRECTION('ref_axis',(0.,0.,-1.));
#26601=DIRECTION('center_axis',(-1.,0.,0.));
#26602=DIRECTION('ref_axis',(0.,-1.,1.83697019872103E-16));
#26603=DIRECTION('center_axis',(0.,-1.,-1.22464679914735E-16));
#26604=DIRECTION('ref_axis',(0.,-1.22464679914735E-16,1.));
#26605=DIRECTION('center_axis',(1.,0.,0.));
#26606=DIRECTION('ref_axis',(0.,-1.,1.83697019872103E-16));
#26607=DIRECTION('center_axis',(1.,0.,0.));
#26608=DIRECTION('ref_axis',(0.,-1.,1.83697019872103E-16));
#26609=DIRECTION('center_axis',(1.,0.,0.));
#26610=DIRECTION('ref_axis',(0.,1.,0.));
#26611=DIRECTION('',(-1.,0.,0.));
#26612=DIRECTION('center_axis',(-1.,0.,0.));
#26613=DIRECTION('ref_axis',(0.,-1.,1.83697019872103E-16));
#26614=DIRECTION('center_axis',(-1.,0.,0.));
#26615=DIRECTION('ref_axis',(0.,-1.,1.83697019872103E-16));
#26616=DIRECTION('center_axis',(1.,0.,0.));
#26617=DIRECTION('ref_axis',(0.,0.,-1.));
#26618=DIRECTION('center_axis',(1.,0.,0.));
#26619=DIRECTION('ref_axis',(0.,0.,-1.));
#26620=DIRECTION('center_axis',(-0.816496580927728,-0.40824829046386,0.408248290463863));
#26621=DIRECTION('ref_axis',(0.577350269189627,-0.577350269189624,0.577350269189627));
#26622=DIRECTION('center_axis',(0.,-1.,0.));
#26623=DIRECTION('ref_axis',(0.,0.,1.));
#26624=DIRECTION('center_axis',(0.,0.,1.));
#26625=DIRECTION('ref_axis',(1.,0.,0.));
#26626=DIRECTION('center_axis',(0.,0.,-1.));
#26627=DIRECTION('ref_axis',(0.707106781186548,-0.707106781186548,0.));
#26628=DIRECTION('center_axis',(0.,0.,1.));
#26629=DIRECTION('ref_axis',(0.,-1.,0.));
#26630=DIRECTION('',(0.,0.,-1.));
#26631=DIRECTION('center_axis',(0.,-1.,0.));
#26632=DIRECTION('ref_axis',(0.707106781186548,0.,0.707106781186548));
#26633=DIRECTION('center_axis',(-0.816496580927727,-0.40824829046386,-0.408248290463864));
#26634=DIRECTION('ref_axis',(0.577350269189627,-0.577350269189624,-0.577350269189627));
#26635=DIRECTION('center_axis',(1.,0.,0.));
#26636=DIRECTION('ref_axis',(0.,0.,-1.));
#26637=DIRECTION('center_axis',(0.,-1.,0.));
#26638=DIRECTION('ref_axis',(0.,0.,-1.));
#26639=DIRECTION('center_axis',(0.,1.63268091856641E-16,1.));
#26640=DIRECTION('ref_axis',(-0.707106781186548,0.707106781186548,0.));
#26641=DIRECTION('center_axis',(-0.707106781186548,0.,-0.707106781186548));
#26642=DIRECTION('ref_axis',(-0.707106781186547,6.13317366673349E-17,0.707106781186547));
#26643=DIRECTION('',(0.,-1.63268091856641E-16,-1.));
#26644=DIRECTION('center_axis',(0.,0.,1.));
#26645=DIRECTION('ref_axis',(0.,1.,0.));
#26646=DIRECTION('',(0.,1.63268091856641E-16,1.));
#26647=DIRECTION('center_axis',(1.,0.,0.));
#26648=DIRECTION('ref_axis',(0.,0.707106781186548,-0.707106781186548));
#26649=DIRECTION('center_axis',(1.,0.,0.));
#26650=DIRECTION('ref_axis',(0.,0.,-1.));
#26651=DIRECTION('',(1.,0.,0.));
#26652=DIRECTION('center_axis',(-1.,0.,0.));
#26653=DIRECTION('ref_axis',(0.,1.,0.));
#26654=DIRECTION('',(-1.,0.,0.));
#26655=DIRECTION('center_axis',(0.,1.63268091856641E-16,1.));
#26656=DIRECTION('ref_axis',(0.707106781186548,0.707106781186548,0.));
#26657=DIRECTION('center_axis',(0.,0.,1.));
#26658=DIRECTION('ref_axis',(1.,0.,0.));
#26659=DIRECTION('',(0.,1.63268091856641E-16,1.));
#26660=DIRECTION('center_axis',(0.,0.,-1.));
#26661=DIRECTION('ref_axis',(0.,1.,0.));
#26662=DIRECTION('',(0.,-1.63268091856641E-16,-1.));
#26663=DIRECTION('center_axis',(-0.816496580927728,0.408248290463863,0.40824829046386));
#26664=DIRECTION('ref_axis',(0.577350269189626,0.577350269189628,0.577350269189624));
#26665=DIRECTION('center_axis',(1.,0.,0.));
#26666=DIRECTION('ref_axis',(0.,0.707106781186549,0.707106781186546));
#26667=DIRECTION('center_axis',(0.,1.,0.));
#26668=DIRECTION('ref_axis',(0.707106781186549,0.,0.707106781186546));
#26669=DIRECTION('center_axis',(0.408248290463864,-0.816496580927727,-0.40824829046386));
#26670=DIRECTION('ref_axis',(0.577350269189626,0.577350269189627,-0.577350269189624));
#26671=DIRECTION('center_axis',(0.,1.,0.));
#26672=DIRECTION('ref_axis',(0.707106781186546,0.,-0.707106781186549));
#26673=DIRECTION('center_axis',(-0.408248290463865,-0.816496580927727,-0.40824829046386));
#26674=DIRECTION('ref_axis',(-0.577350269189626,0.577350269189627,-0.577350269189624));
#26675=DIRECTION('center_axis',(0.,1.,0.));
#26676=DIRECTION('ref_axis',(-0.707106781186546,0.,-0.707106781186549));
#26677=DIRECTION('center_axis',(1.,0.,0.));
#26678=DIRECTION('ref_axis',(0.,0.,-1.));
#26679=DIRECTION('',(0.,1.,0.));
#26680=DIRECTION('',(0.,0.,-1.));
#26681=DIRECTION('center_axis',(0.,1.,0.));
#26682=DIRECTION('ref_axis',(-0.707106781186548,0.,-0.707106781186548));
#26683=DIRECTION('',(0.,-1.,0.));
#26684=DIRECTION('center_axis',(0.,1.,0.));
#26685=DIRECTION('ref_axis',(0.,0.,-1.));
#26686=DIRECTION('center_axis',(0.,0.,-1.));
#26687=DIRECTION('ref_axis',(0.,1.,0.));
#26688=DIRECTION('',(0.,1.,0.));
#26689=DIRECTION('',(1.,0.,0.));
#26690=DIRECTION('center_axis',(0.,1.,0.));
#26691=DIRECTION('ref_axis',(0.707106781186548,0.,-0.707106781186548));
#26692=DIRECTION('',(0.,-1.,0.));
#26693=DIRECTION('center_axis',(0.,-1.,0.));
#26694=DIRECTION('ref_axis',(0.,0.,-1.));
#26695=DIRECTION('center_axis',(1.,0.,0.));
#26696=DIRECTION('ref_axis',(0.,0.,-1.));
#26697=DIRECTION('',(0.,1.,0.));
#26698=DIRECTION('',(0.,0.,1.));
#26699=DIRECTION('center_axis',(1.,0.,0.));
#26700=DIRECTION('ref_axis',(0.,0.,-1.));
#26701=DIRECTION('center_axis',(0.,-1.,-1.22464679914735E-16));
#26702=DIRECTION('ref_axis',(0.,-1.22464679914735E-16,1.));
#26703=DIRECTION('center_axis',(1.,0.,0.));
#26704=DIRECTION('ref_axis',(0.,-1.,3.06161699786838E-17));
#26705=DIRECTION('center_axis',(1.,0.,0.));
#26706=DIRECTION('ref_axis',(0.,-1.,3.06161699786838E-17));
#26707=DIRECTION('center_axis',(1.,0.,0.));
#26708=DIRECTION('ref_axis',(0.,1.,0.));
#26709=DIRECTION('',(-0.707106781186545,0.70710678118655,8.65956056235496E-17));
#26710=DIRECTION('center_axis',(-1.,0.,0.));
#26711=DIRECTION('ref_axis',(0.,-1.,3.06161699786838E-17));
#26712=DIRECTION('center_axis',(-1.,0.,0.));
#26713=DIRECTION('ref_axis',(0.,-1.,3.06161699786838E-17));
#26714=DIRECTION('center_axis',(1.,0.,0.));
#26715=DIRECTION('ref_axis',(0.,0.,-1.));
#26716=DIRECTION('center_axis',(0.,-1.,-1.22464679914735E-16));
#26717=DIRECTION('ref_axis',(0.,-1.22464679914735E-16,1.));
#26718=DIRECTION('center_axis',(1.,0.,0.));
#26719=DIRECTION('ref_axis',(0.,-1.,1.83697019872103E-16));
#26720=DIRECTION('center_axis',(1.,0.,0.));
#26721=DIRECTION('ref_axis',(0.,-1.,1.83697019872103E-16));
#26722=DIRECTION('center_axis',(1.,0.,0.));
#26723=DIRECTION('ref_axis',(0.,1.,0.));
#26724=DIRECTION('',(-1.,0.,0.));
#26725=DIRECTION('center_axis',(1.,0.,0.));
#26726=DIRECTION('ref_axis',(0.,1.,-1.82855839818329E-16));
#26727=DIRECTION('center_axis',(1.,0.,0.));
#26728=DIRECTION('ref_axis',(0.,0.,-1.));
#26729=DIRECTION('center_axis',(0.,-3.05320519733064E-16,-1.));
#26730=DIRECTION('ref_axis',(0.,-1.,3.05320519733064E-16));
#26731=DIRECTION('center_axis',(1.,0.,0.));
#26732=DIRECTION('ref_axis',(0.,0.,-1.));
#26733=DIRECTION('center_axis',(0.,-1.,-1.22464679914735E-16));
#26734=DIRECTION('ref_axis',(0.,-1.22464679914735E-16,1.));
#26735=DIRECTION('center_axis',(1.,0.,0.));
#26736=DIRECTION('ref_axis',(0.,-1.,1.83697019872103E-16));
#26737=DIRECTION('center_axis',(-1.,0.,0.));
#26738=DIRECTION('ref_axis',(0.,0.,1.));
#26739=DIRECTION('center_axis',(-1.,0.,0.));
#26740=DIRECTION('ref_axis',(0.,-1.,1.83697019872103E-16));
#26741=DIRECTION('center_axis',(0.,0.,-1.));
#26742=DIRECTION('ref_axis',(-0.707106781186548,-0.707106781186548,0.));
#26743=DIRECTION('center_axis',(0.,0.,1.));
#26744=DIRECTION('ref_axis',(-1.,0.,0.));
#26745=DIRECTION('',(0.,0.,1.));
#26746=DIRECTION('center_axis',(-0.707106781186548,0.,-0.707106781186548));
#26747=DIRECTION('ref_axis',(-0.707106781186547,0.,0.707106781186547));
#26748=DIRECTION('center_axis',(0.408248290463865,-0.816496580927727,0.40824829046386));
#26749=DIRECTION('ref_axis',(-0.577350269189626,-0.577350269189627,-0.577350269189624));
#26750=DIRECTION('center_axis',(-1.,0.,0.));
#26751=DIRECTION('ref_axis',(0.,-0.707106781186546,-0.707106781186549));
#26752=DIRECTION('center_axis',(1.,0.,0.));
#26753=DIRECTION('ref_axis',(0.,-0.707106781186548,0.707106781186548));
#26754=DIRECTION('',(1.,0.,0.));
#26755=DIRECTION('center_axis',(1.,0.,0.));
#26756=DIRECTION('ref_axis',(0.,-1.,0.));
#26757=DIRECTION('',(-1.,0.,0.));
#26758=DIRECTION('center_axis',(0.,-1.,0.));
#26759=DIRECTION('ref_axis',(0.,0.,-1.));
#26760=DIRECTION('',(-1.,0.,0.));
#26761=DIRECTION('',(0.,0.,-1.));
#26762=DIRECTION('center_axis',(1.,0.,0.));
#26763=DIRECTION('ref_axis',(0.,-0.707106781186548,-0.707106781186548));
#26764=DIRECTION('center_axis',(1.,0.,0.));
#26765=DIRECTION('ref_axis',(0.,-0.707106781186546,-0.707106781186549));
#26766=DIRECTION('center_axis',(0.,1.,-1.63268091856641E-16));
#26767=DIRECTION('ref_axis',(0.,1.63268091856641E-16,1.));
#26768=DIRECTION('',(-1.,0.,0.));
#26769=DIRECTION('center_axis',(-0.408248290463865,-0.816496580927727,0.40824829046386));
#26770=DIRECTION('ref_axis',(0.577350269189626,-0.577350269189627,-0.577350269189624));
#26771=DIRECTION('center_axis',(0.,0.,-1.));
#26772=DIRECTION('ref_axis',(0.707106781186548,-0.707106781186548,0.));
#26773=DIRECTION('center_axis',(1.,0.,0.));
#26774=DIRECTION('ref_axis',(0.,0.707106781186548,0.707106781186548));
#26775=DIRECTION('',(1.,0.,0.));
#26776=DIRECTION('center_axis',(-0.408248290463864,-0.816496580927727,-0.40824829046386));
#26777=DIRECTION('ref_axis',(0.577350269189627,-0.577350269189628,0.577350269189623));
#26778=DIRECTION('center_axis',(0.,-1.,0.));
#26779=DIRECTION('ref_axis',(0.,0.,1.));
#26780=DIRECTION('center_axis',(0.,0.,1.));
#26781=DIRECTION('ref_axis',(1.,0.,0.));
#26782=DIRECTION('center_axis',(0.,0.,-1.));
#26783=DIRECTION('ref_axis',(0.707106781186548,-0.707106781186548,0.));
#26784=DIRECTION('center_axis',(0.,-1.,0.));
#26785=DIRECTION('ref_axis',(0.707106781186548,0.,0.707106781186548));
#26786=DIRECTION('',(0.,-1.,0.));
#26787=DIRECTION('center_axis',(1.,0.,0.));
#26788=DIRECTION('ref_axis',(0.,0.,-1.));
#26789=DIRECTION('center_axis',(0.,-1.,-1.22464679914735E-16));
#26790=DIRECTION('ref_axis',(0.,-1.22464679914735E-16,1.));
#26791=DIRECTION('center_axis',(1.,0.,0.));
#26792=DIRECTION('ref_axis',(0.,-1.,1.83697019872103E-16));
#26793=DIRECTION('center_axis',(1.,0.,0.));
#26794=DIRECTION('ref_axis',(0.,-1.,1.83697019872103E-16));
#26795=DIRECTION('center_axis',(1.,0.,0.));
#26796=DIRECTION('ref_axis',(0.,1.,0.));
#26797=DIRECTION('center_axis',(-1.,0.,0.));
#26798=DIRECTION('ref_axis',(0.,1.,0.));
#26799=DIRECTION('',(-1.,0.,0.));
#26800=DIRECTION('center_axis',(-1.,0.,0.));
#26801=DIRECTION('ref_axis',(0.,1.,0.));
#26802=DIRECTION('center_axis',(1.,0.,0.));
#26803=DIRECTION('ref_axis',(0.,0.,-1.));
#26804=DIRECTION('center_axis',(0.,-1.,-1.22464679914735E-16));
#26805=DIRECTION('ref_axis',(0.,-1.22464679914735E-16,1.));
#26806=DIRECTION('center_axis',(1.,0.,0.));
#26807=DIRECTION('ref_axis',(0.,1.,0.));
#26808=DIRECTION('center_axis',(-1.,0.,0.));
#26809=DIRECTION('ref_axis',(0.,0.,1.));
#26810=DIRECTION('center_axis',(1.,0.,0.));
#26811=DIRECTION('ref_axis',(0.,0.,-1.));
#26812=DIRECTION('center_axis',(1.,0.,0.));
#26813=DIRECTION('ref_axis',(0.,1.,0.));
#26814=DIRECTION('',(1.,0.,0.));
#26815=DIRECTION('center_axis',(0.,0.,1.));
#26816=DIRECTION('ref_axis',(0.,-1.,0.));
#26817=DIRECTION('center_axis',(0.,0.,-1.));
#26818=DIRECTION('ref_axis',(0.,1.,0.));
#26819=DIRECTION('center_axis',(0.,-1.,0.));
#26820=DIRECTION('ref_axis',(0.,0.,-1.));
#26821=DIRECTION('center_axis',(0.,0.,1.));
#26822=DIRECTION('ref_axis',(0.,-1.,0.));
#26823=DIRECTION('center_axis',(0.,1.,0.));
#26824=DIRECTION('ref_axis',(0.,0.,1.));
#26825=DIRECTION('center_axis',(0.,-1.63268091856641E-16,-1.));
#26826=DIRECTION('ref_axis',(0.,1.,-1.63268091856641E-16));
#26827=DIRECTION('axis',(0.,0.,1.));
#26828=DIRECTION('refdir',(1.,0.,0.));
#26829=DIRECTION('center_axis',(0.577350269189626,0.577350269189626,0.577350269189626));
#26830=DIRECTION('ref_axis',(0.707106781186548,0.,-0.707106781186547));
#26831=DIRECTION('',(-0.707106781186548,0.,0.707106781186547));
#26832=DIRECTION('',(0.707106781186548,-0.707106781186548,0.));
#26833=DIRECTION('',(0.,0.707106781186548,-0.707106781186547));
#26834=DIRECTION('center_axis',(0.577350269189626,-0.577350269189626,0.577350269189626));
#26835=DIRECTION('ref_axis',(0.707106781186548,0.,-0.707106781186547));
#26836=DIRECTION('',(0.,0.707106781186548,0.707106781186547));
#26837=DIRECTION('',(-0.707106781186548,-0.707106781186548,0.));
#26838=DIRECTION('',(0.707106781186548,0.,-0.707106781186547));
#26839=DIRECTION('center_axis',(-0.577350269189626,0.577350269189626,0.577350269189626));
#26840=DIRECTION('ref_axis',(0.707106781186548,0.,0.707106781186547));
#26841=DIRECTION('',(0.,-0.707106781186548,0.707106781186547));
#26842=DIRECTION('',(0.707106781186548,0.707106781186548,0.));
#26843=DIRECTION('',(-0.707106781186548,0.,-0.707106781186547));
#26844=DIRECTION('center_axis',(0.577350269189626,0.577350269189626,-0.577350269189626));
#26845=DIRECTION('ref_axis',(-0.707106781186548,0.,-0.707106781186547));
#26846=DIRECTION('',(0.,-0.707106781186548,-0.707106781186547));
#26847=DIRECTION('',(-0.707106781186548,0.707106781186548,0.));
#26848=DIRECTION('',(0.707106781186548,0.,0.707106781186547));
#26849=DIRECTION('center_axis',(0.707106781186548,0.707106781186548,0.));
#26850=DIRECTION('ref_axis',(0.,0.,-1.));
#26851=DIRECTION('',(0.,0.,-1.));
#26852=DIRECTION('',(0.,0.,1.));
#26853=DIRECTION('center_axis',(-0.577350269189624,-0.577350269189629,0.577350269189625));
#26854=DIRECTION('ref_axis',(0.707106781186548,0.,0.707106781186547));
#26855=DIRECTION('',(0.707106781186548,0.,0.707106781186547));
#26856=DIRECTION('',(-0.70710678118655,0.707106781186545,0.));
#26857=DIRECTION('',(5.23364152894591E-15,-0.707106781186548,-0.707106781186547));
#26858=DIRECTION('center_axis',(0.577350269189626,-0.577350269189626,-0.577350269189626));
#26859=DIRECTION('ref_axis',(-0.707106781186548,0.,-0.707106781186547));
#26860=DIRECTION('',(-0.707106781186548,0.,-0.707106781186547));
#26861=DIRECTION('',(0.707106781186548,0.707106781186548,0.));
#26862=DIRECTION('',(0.,-0.707106781186548,0.707106781186547));
#26863=DIRECTION('center_axis',(0.707106781186548,-0.707106781186548,0.));
#26864=DIRECTION('ref_axis',(0.,0.,-1.));
#26865=DIRECTION('',(0.,0.,-1.));
#26866=DIRECTION('',(0.,0.,1.));
#26867=DIRECTION('center_axis',(-0.577350269189626,0.577350269189626,-0.577350269189626));
#26868=DIRECTION('ref_axis',(-0.707106781186548,0.,0.707106781186547));
#26869=DIRECTION('',(0.707106781186548,0.,-0.707106781186547));
#26870=DIRECTION('',(-0.707106781186548,-0.707106781186548,0.));
#26871=DIRECTION('',(0.,0.707106781186548,0.707106781186547));
#26872=DIRECTION('center_axis',(-0.707106781186548,0.707106781186548,0.));
#26873=DIRECTION('ref_axis',(0.,0.,1.));
#26874=DIRECTION('',(0.,0.,1.));
#26875=DIRECTION('',(0.,0.,-1.));
#26876=DIRECTION('center_axis',(0.,0.707106781186547,-0.707106781186548));
#26877=DIRECTION('ref_axis',(-1.,0.,0.));
#26878=DIRECTION('',(-1.,0.,0.));
#26879=DIRECTION('',(1.,0.,0.));
#26880=DIRECTION('center_axis',(-0.577350269189624,-0.577350269189628,-0.577350269189625));
#26881=DIRECTION('ref_axis',(-0.707106781186548,0.,0.707106781186547));
#26882=DIRECTION('',(-5.23364152894591E-15,0.707106781186548,-0.707106781186547));
#26883=DIRECTION('',(0.70710678118655,-0.707106781186545,0.));
#26884=DIRECTION('',(-0.707106781186548,0.,0.707106781186547));
#26885=DIRECTION('center_axis',(-0.707106781186545,-0.70710678118655,0.));
#26886=DIRECTION('ref_axis',(0.,0.,1.));
#26887=DIRECTION('',(0.,0.,-1.));
#26888=DIRECTION('',(0.,0.,1.));
#26889=DIRECTION('center_axis',(-0.707106781186547,0.,-0.707106781186548));
#26890=DIRECTION('ref_axis',(-0.707106781186548,0.,0.707106781186547));
#26891=DIRECTION('',(0.,-1.,0.));
#26892=DIRECTION('',(0.,1.,0.));
#26893=DIRECTION('center_axis',(0.,-0.707106781186547,-0.707106781186548));
#26894=DIRECTION('ref_axis',(-1.,0.,0.));
#26895=DIRECTION('',(1.,0.,0.));
#26896=DIRECTION('',(-1.,0.,0.));
#26897=DIRECTION('center_axis',(0.707106781186547,0.,-0.707106781186548));
#26898=DIRECTION('ref_axis',(-0.707106781186548,0.,-0.707106781186547));
#26899=DIRECTION('',(0.,1.,0.));
#26900=DIRECTION('',(0.,-1.,0.));
#26901=DIRECTION('center_axis',(0.,-0.707106781186547,0.707106781186548));
#26902=DIRECTION('ref_axis',(1.,0.,0.));
#26903=DIRECTION('',(-1.,0.,0.));
#26904=DIRECTION('',(1.,0.,0.));
#26905=DIRECTION('center_axis',(-0.707106781186547,0.,0.707106781186548));
#26906=DIRECTION('ref_axis',(0.707106781186548,0.,0.707106781186547));
#26907=DIRECTION('',(0.,1.,0.));
#26908=DIRECTION('',(0.,-1.,0.));
#26909=DIRECTION('center_axis',(0.,0.707106781186547,0.707106781186548));
#26910=DIRECTION('ref_axis',(1.,0.,0.));
#26911=DIRECTION('',(1.,0.,0.));
#26912=DIRECTION('',(-1.,0.,0.));
#26913=DIRECTION('center_axis',(0.707106781186547,0.,0.707106781186548));
#26914=DIRECTION('ref_axis',(0.707106781186548,0.,-0.707106781186547));
#26915=DIRECTION('',(0.,-1.,0.));
#26916=DIRECTION('',(0.,1.,0.));
#26917=DIRECTION('center_axis',(1.,0.,0.));
#26918=DIRECTION('ref_axis',(0.,1.,0.));
#26919=DIRECTION('center_axis',(0.,1.,0.));
#26920=DIRECTION('ref_axis',(-1.,0.,0.));
#26921=DIRECTION('center_axis',(0.,0.,-1.));
#26922=DIRECTION('ref_axis',(-1.,0.,0.));
#26923=DIRECTION('center_axis',(0.,-1.,0.));
#26924=DIRECTION('ref_axis',(1.,0.,0.));
#26925=DIRECTION('center_axis',(-1.,0.,0.));
#26926=DIRECTION('ref_axis',(0.,-1.,0.));
#26927=DIRECTION('center_axis',(0.,0.,1.));
#26928=DIRECTION('ref_axis',(1.,0.,0.));
#26929=DIRECTION('axis',(0.,0.,1.));
#26930=DIRECTION('refdir',(1.,0.,0.));
#26931=DIRECTION('center_axis',(0.0524864875083004,-0.00359342805144231,
0.998615169073593));
#26932=DIRECTION('ref_axis',(-0.996282959525764,0.0682093869087291,0.052609353694185));
#26933=DIRECTION('center_axis',(0.052486487479681,0.00359342804742538,0.998615169075111));
#26934=DIRECTION('ref_axis',(0.504066799442469,0.863157308043356,-0.029599379574115));
#26935=DIRECTION('center_axis',(0.052486487479681,0.00359342804742538,0.998615169075111));
#26936=DIRECTION('ref_axis',(0.504066799442469,0.863157308043356,-0.029599379574115));
#26937=DIRECTION('center_axis',(0.0524864875083004,-0.00359342805144231,
0.998615169073593));
#26938=DIRECTION('ref_axis',(-0.996282959525764,0.0682093869087291,0.052609353694185));
#26939=DIRECTION('axis',(0.,0.,1.));
#26940=DIRECTION('refdir',(1.,0.,0.));
#26941=DIRECTION('center_axis',(1.,0.,0.));
#26942=DIRECTION('ref_axis',(0.,0.,-1.));
#26943=DIRECTION('center_axis',(-1.,0.,0.));
#26944=DIRECTION('ref_axis',(0.,-1.,1.83697019872103E-16));
#26945=DIRECTION('center_axis',(0.,-1.,-1.22464679914735E-16));
#26946=DIRECTION('ref_axis',(0.,-1.22464679914735E-16,1.));
#26947=DIRECTION('center_axis',(1.,0.,0.));
#26948=DIRECTION('ref_axis',(0.,-1.,1.83697019872103E-16));
#26949=DIRECTION('center_axis',(1.,0.,0.));
#26950=DIRECTION('ref_axis',(0.,-1.,1.83697019872103E-16));
#26951=DIRECTION('center_axis',(1.,0.,0.));
#26952=DIRECTION('ref_axis',(0.,1.,0.));
#26953=DIRECTION('center_axis',(-1.,0.,0.));
#26954=DIRECTION('ref_axis',(0.,-1.,1.83697019872103E-16));
#26955=DIRECTION('center_axis',(-1.,0.,0.));
#26956=DIRECTION('ref_axis',(0.,-1.,1.83697019872103E-16));
#26957=DIRECTION('',(-1.,0.,0.));
#26958=DIRECTION('center_axis',(-1.,0.,0.));
#26959=DIRECTION('ref_axis',(0.,0.,1.));
#26960=DIRECTION('',(0.,0.707106781186548,-0.707106781186548));
#26961=DIRECTION('center_axis',(1.,0.,0.));
#26962=DIRECTION('ref_axis',(0.,0.0791961191078487,0.996859054590094));
#26963=DIRECTION('center_axis',(1.,0.,0.));
#26964=DIRECTION('ref_axis',(0.,0.,-1.));
#26965=DIRECTION('center_axis',(1.,0.,0.));
#26966=DIRECTION('ref_axis',(0.,-0.0791961191078487,0.996859054590094));
#26967=DIRECTION('',(0.,0.707106781186547,0.707106781186548));
#26968=DIRECTION('',(0.,0.707106781186548,-0.707106781186548));
#26969=DIRECTION('',(0.,-0.707106781186548,-0.707106781186548));
#26970=DIRECTION('center_axis',(1.,0.,0.));
#26971=DIRECTION('ref_axis',(0.,0.996859054590094,-0.0791961191078487));
#26972=DIRECTION('center_axis',(1.,0.,0.));
#26973=DIRECTION('ref_axis',(0.,0.,-1.));
#26974=DIRECTION('center_axis',(1.,0.,0.));
#26975=DIRECTION('ref_axis',(0.,0.,-1.));
#26976=DIRECTION('center_axis',(1.,0.,0.));
#26977=DIRECTION('ref_axis',(0.,0.996859054590094,0.0791961191078482));
#26978=DIRECTION('',(0.,0.707106781186548,-0.707106781186547));
#26979=DIRECTION('',(0.,-0.707106781186548,-0.707106781186548));
#26980=DIRECTION('',(0.,-0.707106781186548,0.707106781186548));
#26981=DIRECTION('center_axis',(1.,0.,0.));
#26982=DIRECTION('ref_axis',(0.,-0.0791961191078482,-0.996859054590094));
#26983=DIRECTION('center_axis',(1.,0.,0.));
#26984=DIRECTION('ref_axis',(0.,0.,-1.));
#26985=DIRECTION('center_axis',(1.,0.,0.));
#26986=DIRECTION('ref_axis',(0.,0.0791961191078487,-0.996859054590094));
#26987=DIRECTION('',(0.,-0.707106781186548,-0.707106781186548));
#26988=DIRECTION('',(0.,-0.707106781186548,0.707106781186548));
#26989=DIRECTION('',(0.,0.707106781186548,0.707106781186548));
#26990=DIRECTION('center_axis',(1.,0.,0.));
#26991=DIRECTION('ref_axis',(0.,-0.996859054590094,0.0791961191078482));
#26992=DIRECTION('center_axis',(1.,0.,0.));
#26993=DIRECTION('ref_axis',(0.,0.,-1.));
#26994=DIRECTION('center_axis',(1.,0.,0.));
#26995=DIRECTION('ref_axis',(0.,-0.996859054590094,-0.0791961191078487));
#26996=DIRECTION('',(0.,-0.707106781186548,0.707106781186548));
#26997=DIRECTION('',(0.,0.707106781186547,0.707106781186547));
#26998=DIRECTION('center_axis',(1.,0.,0.));
#26999=DIRECTION('ref_axis',(0.,0.,-1.));
#27000=DIRECTION('center_axis',(0.,-1.,-1.22464679914735E-16));
#27001=DIRECTION('ref_axis',(0.,-1.22464679914735E-16,1.));
#27002=DIRECTION('center_axis',(1.,0.,0.));
#27003=DIRECTION('ref_axis',(0.,-1.,1.83697019872103E-16));
#27004=DIRECTION('center_axis',(1.,0.,0.));
#27005=DIRECTION('ref_axis',(0.,0.,-1.));
#27006=DIRECTION('',(0.,0.707106781186548,-0.707106781186548));
#27007=DIRECTION('center_axis',(1.,0.,0.));
#27008=DIRECTION('ref_axis',(0.,0.,-1.));
#27009=DIRECTION('',(0.,-0.707106781186548,-0.707106781186548));
#27010=DIRECTION('',(0.,0.707106781186548,-0.707106781186548));
#27011=DIRECTION('',(0.,0.707106781186548,0.707106781186548));
#27012=DIRECTION('center_axis',(1.,0.,0.));
#27013=DIRECTION('ref_axis',(0.,0.,-1.));
#27014=DIRECTION('',(0.,0.707106781186548,-0.707106781186548));
#27015=DIRECTION('',(0.,0.707106781186548,0.707106781186548));
#27016=DIRECTION('',(0.,-0.707106781186548,0.707106781186547));
#27017=DIRECTION('center_axis',(1.,0.,0.));
#27018=DIRECTION('ref_axis',(0.,0.,-1.));
#27019=DIRECTION('center_axis',(-1.,0.,0.));
#27020=DIRECTION('ref_axis',(0.,0.996859054590094,-0.0791961191078487));
#27021=DIRECTION('',(0.,0.707106781186548,0.707106781186548));
#27022=DIRECTION('',(0.,-0.707106781186548,0.707106781186548));
#27023=DIRECTION('',(0.,-0.707106781186547,-0.707106781186548));
#27024=DIRECTION('center_axis',(-1.,0.,0.));
#27025=DIRECTION('ref_axis',(0.,-0.0791961191078487,0.996859054590094));
#27026=DIRECTION('center_axis',(1.,0.,0.));
#27027=DIRECTION('ref_axis',(0.,0.,-1.));
#27028=DIRECTION('',(0.,-0.707106781186548,0.707106781186548));
#27029=DIRECTION('',(0.,-0.707106781186548,-0.707106781186548));
#27030=DIRECTION('center_axis',(0.,-0.707106781186548,-0.707106781186548));
#27031=DIRECTION('ref_axis',(-0.707106781186547,0.5,-0.5));
#27032=DIRECTION('center_axis',(0.,0.707106781186548,0.707106781186548));
#27033=DIRECTION('ref_axis',(-0.707106781186547,0.5,-0.5));
#27034=DIRECTION('',(0.,-0.707106781186547,-0.707106781186547));
#27035=DIRECTION('center_axis',(0.,-0.707106781186548,-0.707106781186548));
#27036=DIRECTION('ref_axis',(-0.707106781186547,0.5,-0.5));
#27037=DIRECTION('center_axis',(0.,-0.707106781186548,0.707106781186548));
#27038=DIRECTION('ref_axis',(0.,-0.707106781186548,-0.707106781186548));
#27039=DIRECTION('',(1.,0.,0.));
#27040=DIRECTION('',(0.,0.707106781186548,0.707106781186548));
#27041=DIRECTION('',(1.,0.,0.));
#27042=DIRECTION('center_axis',(0.,0.707106781186548,0.707106781186548));
#27043=DIRECTION('ref_axis',(0.707106781186545,0.500000000000005,-0.499999999999999));
#27044=DIRECTION('center_axis',(0.,-0.707106781186548,-0.707106781186548));
#27045=DIRECTION('ref_axis',(0.707106781186545,0.500000000000005,-0.499999999999999));
#27046=DIRECTION('center_axis',(0.,0.707106781186548,0.707106781186548));
#27047=DIRECTION('ref_axis',(0.707106781186545,0.500000000000005,-0.499999999999999));
#27048=DIRECTION('center_axis',(0.,0.707106781186548,-0.707106781186548));
#27049=DIRECTION('ref_axis',(-0.707106781186547,0.5,0.5));
#27050=DIRECTION('center_axis',(0.,-0.707106781186548,0.707106781186548));
#27051=DIRECTION('ref_axis',(-0.707106781186547,0.5,0.5));
#27052=DIRECTION('',(0.,0.707106781186548,-0.707106781186548));
#27053=DIRECTION('center_axis',(0.,0.707106781186548,-0.707106781186548));
#27054=DIRECTION('ref_axis',(-0.707106781186547,0.5,0.5));
#27055=DIRECTION('center_axis',(0.,-0.707106781186548,-0.707106781186548));
#27056=DIRECTION('ref_axis',(0.,0.707106781186548,-0.707106781186548));
#27057=DIRECTION('',(1.,0.,0.));
#27058=DIRECTION('',(0.,-0.707106781186548,0.707106781186548));
#27059=DIRECTION('',(1.,0.,0.));
#27060=DIRECTION('center_axis',(0.,-0.707106781186548,0.707106781186548));
#27061=DIRECTION('ref_axis',(0.707106781186543,0.500000000000004,0.500000000000004));
#27062=DIRECTION('center_axis',(0.,0.707106781186548,-0.707106781186548));
#27063=DIRECTION('ref_axis',(0.707106781186543,0.500000000000004,0.500000000000004));
#27064=DIRECTION('center_axis',(0.,-0.707106781186548,0.707106781186548));
#27065=DIRECTION('ref_axis',(0.707106781186543,0.500000000000004,0.500000000000004));
#27066=DIRECTION('center_axis',(0.,0.707106781186548,0.707106781186548));
#27067=DIRECTION('ref_axis',(-0.707106781186547,-0.5,0.5));
#27068=DIRECTION('center_axis',(0.,-0.707106781186547,-0.707106781186548));
#27069=DIRECTION('ref_axis',(-0.707106781186547,-0.5,0.5));
#27070=DIRECTION('',(0.,0.707106781186548,0.707106781186548));
#27071=DIRECTION('center_axis',(0.,0.707106781186548,0.707106781186548));
#27072=DIRECTION('ref_axis',(-0.707106781186547,-0.5,0.5));
#27073=DIRECTION('center_axis',(0.,0.707106781186548,-0.707106781186548));
#27074=DIRECTION('ref_axis',(0.,0.707106781186548,0.707106781186548));
#27075=DIRECTION('',(1.,0.,0.));
#27076=DIRECTION('',(0.,-0.707106781186548,-0.707106781186548));
#27077=DIRECTION('',(1.,0.,0.));
#27078=DIRECTION('center_axis',(0.,-0.707106781186548,-0.707106781186548));
#27079=DIRECTION('ref_axis',(0.707106781186547,-0.5,0.5));
#27080=DIRECTION('center_axis',(0.,0.707106781186548,0.707106781186548));
#27081=DIRECTION('ref_axis',(0.707106781186547,-0.5,0.5));
#27082=DIRECTION('center_axis',(0.,-0.707106781186547,-0.707106781186548));
#27083=DIRECTION('ref_axis',(0.707106781186547,-0.5,0.5));
#27084=DIRECTION('center_axis',(1.,0.,0.));
#27085=DIRECTION('ref_axis',(0.,0.,-1.));
#27086=DIRECTION('center_axis',(0.,0.197113341951552,0.980380706881103));
#27087=DIRECTION('ref_axis',(-1.,0.,0.));
#27088=DIRECTION('center_axis',(-1.,0.,0.));
#27089=DIRECTION('ref_axis',(0.,-0.707106781185558,0.707106781187537));
#27090=DIRECTION('center_axis',(-4.6165181164541E-10,-0.980380706790106,
-0.197113342404141));
#27091=DIRECTION('ref_axis',(-0.707106782908637,-0.139380180416835,0.693233844291786));
#27092=DIRECTION('center_axis',(1.,0.,0.));
#27093=DIRECTION('ref_axis',(0.,-0.707106781185558,0.707106781187537));
#27094=DIRECTION('center_axis',(0.,0.,1.));
#27095=DIRECTION('ref_axis',(-0.772461049429073,0.635062144293718,0.));
#27096=DIRECTION('center_axis',(-0.700067241886871,-1.1325494929406E-16,
-0.714076926414031));
#27097=DIRECTION('ref_axis',(-0.707106781186542,-0.139380180748398,0.69323384598168));
#27098=DIRECTION('center_axis',(0.,1.58603289232165E-16,1.));
#27099=DIRECTION('ref_axis',(-0.707106781186548,0.707106781186547,0.));
#27100=DIRECTION('center_axis',(0.,-1.,1.58603289232165E-16));
#27101=DIRECTION('ref_axis',(-0.707106781186548,0.,-0.707106781186548));
#27102=DIRECTION('center_axis',(0.,1.,-4.44089209850062E-15));
#27103=DIRECTION('ref_axis',(9.00728158725882E-9,-4.44089209850062E-15,
-1.));
#27104=DIRECTION('',(0.,1.,-1.58603289232165E-16));
#27105=DIRECTION('center_axis',(9.86076131526263E-30,-1.,-8.88178419700124E-15));
#27106=DIRECTION('ref_axis',(-1.,0.,-1.11022302462516E-15));
#27107=DIRECTION('',(0.,-1.,1.58603289232165E-16));
#27108=DIRECTION('center_axis',(-0.33661593132292,-0.848909755674506,-0.407482443180382));
#27109=DIRECTION('ref_axis',(-0.540654873563244,0.52853781957458,-0.654476952208144));
#27110=DIRECTION('center_axis',(0.,-0.210526315789474,-0.9775881905793));
#27111=DIRECTION('ref_axis',(0.,-0.9775881905793,0.210526315789474));
#27112=DIRECTION('center_axis',(-1.,0.,0.));
#27113=DIRECTION('ref_axis',(0.,0.62828086243754,-0.777986605215502));
#27114=DIRECTION('center_axis',(0.392106666069813,0.159229418444589,-0.906034411446615));
#27115=DIRECTION('ref_axis',(-0.839458305969898,-0.340893102399512,-0.423204023225896));
#27116=DIRECTION('center_axis',(-0.700067241886855,0.714076926414047,-1.13254949294063E-16));
#27117=DIRECTION('ref_axis',(4.44089209850063E-15,-4.44089209850063E-15,
-1.));
#27118=DIRECTION('center_axis',(0.,-1.58603289232165E-16,-1.));
#27119=DIRECTION('ref_axis',(-0.707106781186548,0.707106781186548,0.));
#27120=DIRECTION('',(0.,-1.58603289232165E-16,-1.));
#27121=DIRECTION('center_axis',(4.44089209850062E-15,-9.86076131526262E-30,
1.));
#27122=DIRECTION('ref_axis',(2.22044604925031E-15,1.,0.));
#27123=DIRECTION('',(0.,1.58603289232165E-16,1.));
#27124=DIRECTION('center_axis',(0.700212217679577,0.,0.71393476607618));
#27125=DIRECTION('ref_axis',(0.,1.,0.));
#27126=DIRECTION('center_axis',(1.,0.,0.));
#27127=DIRECTION('ref_axis',(0.,1.,0.));
#27128=DIRECTION('center_axis',(1.,0.,0.));
#27129=DIRECTION('ref_axis',(0.,-0.717262041981833,0.696803532663298));
#27130=DIRECTION('center_axis',(-0.70021221767957,0.713934766076186,0.));
#27131=DIRECTION('ref_axis',(0.,0.,-1.));
#27132=DIRECTION('center_axis',(0.,1.58603289232165E-16,1.));
#27133=DIRECTION('ref_axis',(0.,-1.,1.58603289232165E-16));
#27134=DIRECTION('',(-1.,0.,0.));
#27135=DIRECTION('',(0.,-1.,1.58603289232165E-16));
#27136=DIRECTION('',(1.,0.,0.));
#27137=DIRECTION('center_axis',(1.,0.,0.));
#27138=DIRECTION('ref_axis',(0.,-0.773020682523926,-0.634380819689754));
#27139=DIRECTION('',(-1.,0.,0.));
#27140=DIRECTION('center_axis',(1.,0.,0.));
#27141=DIRECTION('ref_axis',(0.,-0.980778988433322,0.195121951219513));
#27142=DIRECTION('center_axis',(1.,0.,0.));
#27143=DIRECTION('ref_axis',(0.,-0.773020682523926,-0.634380819689754));
#27144=DIRECTION('center_axis',(-0.93091161074757,0.339317183161405,0.135157027885253));
#27145=DIRECTION('ref_axis',(-0.365244538597586,-0.864829647402693,-0.344479473986434));
#27146=DIRECTION('center_axis',(0.,-0.195121951219512,-0.980778988433322));
#27147=DIRECTION('ref_axis',(0.,-0.980778988433322,0.195121951219512));
#27148=DIRECTION('center_axis',(-1.,0.,0.));
#27149=DIRECTION('ref_axis',(0.,0.,1.));
#27150=DIRECTION('center_axis',(-1.,0.,0.));
#27151=DIRECTION('ref_axis',(0.,-0.707106781186547,0.707106781186548));
#27152=DIRECTION('center_axis',(1.,0.,0.));
#27153=DIRECTION('ref_axis',(0.,0.,-1.));
#27154=DIRECTION('center_axis',(-1.,0.,0.));
#27155=DIRECTION('ref_axis',(0.,-0.717262041981833,0.696803532663298));
#27156=DIRECTION('center_axis',(2.75992815003008E-16,0.980778988433322,
0.19512195121951));
#27157=DIRECTION('ref_axis',(-0.707106781186547,-0.137972054865666,0.693515473566485));
#27158=DIRECTION('center_axis',(1.,0.,0.));
#27159=DIRECTION('ref_axis',(0.,1.,0.));
#27160=DIRECTION('center_axis',(1.,0.,0.));
#27161=DIRECTION('ref_axis',(0.,-1.,1.83697019872103E-16));
#27162=DIRECTION('',(-1.,0.,0.));
#27163=DIRECTION('center_axis',(1.,0.,0.));
#27164=DIRECTION('ref_axis',(0.,1.,0.));
#27165=DIRECTION('',(1.,0.,0.));
#27166=DIRECTION('center_axis',(1.,0.,0.));
#27167=DIRECTION('ref_axis',(0.,0.,-1.));
#27168=DIRECTION('',(-1.,0.,0.));
#27169=DIRECTION('center_axis',(-1.,0.,0.));
#27170=DIRECTION('ref_axis',(0.,-1.60812264967664E-16,-1.));
#27171=DIRECTION('',(1.,0.,0.));
#27172=DIRECTION('center_axis',(-1.,0.,0.));
#27173=DIRECTION('ref_axis',(0.,0.707106781186547,-0.707106781186548));
#27174=DIRECTION('',(-1.,0.,0.));
#27175=DIRECTION('center_axis',(1.,0.,0.));
#27176=DIRECTION('ref_axis',(0.,1.,0.));
#27177=DIRECTION('',(1.,0.,0.));
#27178=DIRECTION('center_axis',(-1.,0.,0.));
#27179=DIRECTION('ref_axis',(0.,0.707106781186548,0.707106781186547));
#27180=DIRECTION('',(-1.,0.,0.));
#27181=DIRECTION('center_axis',(-1.,0.,0.));
#27182=DIRECTION('ref_axis',(0.,6.12323399573677E-17,1.));
#27183=DIRECTION('',(1.,0.,0.));
#27184=DIRECTION('center_axis',(1.,0.,0.));
#27185=DIRECTION('ref_axis',(0.,1.,0.));
#27186=DIRECTION('center_axis',(1.,0.,0.));
#27187=DIRECTION('ref_axis',(0.,-1.,1.83697019872103E-16));
#27188=DIRECTION('center_axis',(-1.,0.,0.));
#27189=DIRECTION('ref_axis',(0.,0.773020682523925,-0.634380819689755));
#27190=DIRECTION('center_axis',(1.,0.,0.));
#27191=DIRECTION('ref_axis',(0.,0.773020682523925,-0.634380819689755));
#27192=DIRECTION('',(-1.,0.,0.));
#27193=DIRECTION('center_axis',(1.,0.,0.));
#27194=DIRECTION('ref_axis',(0.,0.,-1.));
#27195=DIRECTION('center_axis',(-0.93091161074757,-0.339317183161405,0.135157027885251));
#27196=DIRECTION('ref_axis',(-0.365244538597587,0.864829647402694,-0.344479473986432));
#27197=DIRECTION('center_axis',(0.700212217679577,0.71393476607618,0.));
#27198=DIRECTION('ref_axis',(0.,0.,-1.));
#27199=DIRECTION('center_axis',(0.,0.195121951219512,-0.980778988433322));
#27200=DIRECTION('ref_axis',(0.,0.980778988433322,0.195121951219512));
#27201=DIRECTION('center_axis',(0.392106667949502,-0.159229414617378,-0.906034411305744));
#27202=DIRECTION('ref_axis',(-0.839458309265364,0.340893093909927,-0.423204023527487));
#27203=DIRECTION('center_axis',(-0.700067241886871,-0.714076926414031,0.));
#27204=DIRECTION('ref_axis',(-0.70710678118655,0.693233845981671,0.1393801807484));
#27205=DIRECTION('center_axis',(0.,1.,0.));
#27206=DIRECTION('ref_axis',(-0.707106781186548,0.,-0.707106781186547));
#27207=DIRECTION('center_axis',(0.,0.1971133419404,-0.980380706883345));
#27208=DIRECTION('ref_axis',(0.,0.980380706883345,0.1971133419404));
#27209=DIRECTION('center_axis',(1.,0.,0.));
#27210=DIRECTION('ref_axis',(0.,0.,-1.));
#27211=DIRECTION('center_axis',(1.,3.76456815122937E-17,-3.76456815122937E-17));
#27212=DIRECTION('ref_axis',(0.,0.707106781186547,0.707106781186547));
#27213=DIRECTION('center_axis',(0.,-0.980778988433322,0.195121951219512));
#27214=DIRECTION('ref_axis',(0.,0.195121951219512,0.980778988433322));
#27215=DIRECTION('center_axis',(1.,0.,0.));
#27216=DIRECTION('ref_axis',(0.,1.,0.));
#27217=DIRECTION('center_axis',(-1.,-3.80233094921144E-17,3.80233094921144E-17));
#27218=DIRECTION('ref_axis',(0.,0.707106781186548,0.707106781186548));
#27219=DIRECTION('center_axis',(1.,0.,0.));
#27220=DIRECTION('ref_axis',(0.,0.,-1.));
#27221=DIRECTION('center_axis',(1.,0.,0.));
#27222=DIRECTION('ref_axis',(0.,0.707106781186548,0.707106781186547));
#27223=DIRECTION('center_axis',(4.56684708566872E-15,0.980380706883345,
-0.197113341940397));
#27224=DIRECTION('ref_axis',(-1.,5.55111512312578E-15,4.44089209850062E-15));
#27225=DIRECTION('center_axis',(1.,0.,0.));
#27226=DIRECTION('ref_axis',(0.,0.,-1.));
#27227=DIRECTION('center_axis',(1.,0.,0.));
#27228=DIRECTION('ref_axis',(0.,0.999895356874024,-0.0144663506721044));
#27229=DIRECTION('center_axis',(1.,0.,0.));
#27230=DIRECTION('ref_axis',(0.,0.,-1.));
#27231=DIRECTION('center_axis',(1.,0.,0.));
#27232=DIRECTION('ref_axis',(0.,0.773020682523925,0.634380819689755));
#27233=DIRECTION('',(0.,1.,0.));
#27234=DIRECTION('center_axis',(-1.,0.,0.));
#27235=DIRECTION('ref_axis',(0.,0.99994072112783,-0.0108882611263663));
#27236=DIRECTION('',(0.,-1.,0.));
#27237=DIRECTION('center_axis',(0.,0.,1.));
#27238=DIRECTION('ref_axis',(-0.772461049429072,-0.63506214429372,0.));
#27239=DIRECTION('center_axis',(-0.700067241886868,0.,0.714076926414034));
#27240=DIRECTION('ref_axis',(-0.707106781186553,0.139380180748399,-0.693233845981669));
#27241=DIRECTION('center_axis',(0.,-3.17206578464331E-16,-1.));
#27242=DIRECTION('ref_axis',(-0.707106781186548,-0.707106781186547,0.));
#27243=DIRECTION('center_axis',(0.,-0.980380706883345,-0.1971133419404));
#27244=DIRECTION('ref_axis',(0.,0.1971133419404,-0.980380706883345));
#27245=DIRECTION('center_axis',(1.,0.,0.));
#27246=DIRECTION('ref_axis',(0.,0.,-1.));
#27247=DIRECTION('center_axis',(-6.31716887673555E-15,0.980778988433321,
0.195121951219515));
#27248=DIRECTION('ref_axis',(0.,0.195121951219515,-0.980778988433321));
#27249=DIRECTION('center_axis',(1.,0.,0.));
#27250=DIRECTION('ref_axis',(0.,0.707106781186547,-0.707106781186548));
#27251=DIRECTION('center_axis',(-2.57593294002809E-15,-0.195121951219511,
-0.980778988433322));
#27252=DIRECTION('ref_axis',(-0.707106781186554,0.693515473566478,-0.137972054865664));
#27253=DIRECTION('center_axis',(0.134022231386925,-0.938793849576159,0.317339171064724));
#27254=DIRECTION('ref_axis',(-0.365244538597589,-0.344479473986443,-0.864829647402688));
#27255=DIRECTION('center_axis',(0.700212217679577,0.,-0.71393476607618));
#27256=DIRECTION('ref_axis',(0.,-1.,0.));
#27257=DIRECTION('center_axis',(-1.,0.,0.));
#27258=DIRECTION('ref_axis',(0.,-0.634380819689754,-0.773020682523925));
#27259=DIRECTION('center_axis',(-0.930911610747569,-0.339317183161406,-0.135157027885257));
#27260=DIRECTION('ref_axis',(-0.365244538597591,0.864829647402688,0.344479473986442));
#27261=DIRECTION('center_axis',(0.700212217679577,0.71393476607618,0.));
#27262=DIRECTION('ref_axis',(-0.707106781186547,0.693515473566485,-0.137972054865667));
#27263=DIRECTION('center_axis',(-1.,0.,0.));
#27264=DIRECTION('ref_axis',(0.,0.773020682523925,0.634380819689754));
#27265=DIRECTION('center_axis',(-0.392106667949504,0.159229414617379,-0.906034411305743));
#27266=DIRECTION('ref_axis',(-0.839458309265363,0.340893093909926,0.423204023527489));
#27267=DIRECTION('center_axis',(-0.700067241886868,-0.714076926414034,0.));
#27268=DIRECTION('ref_axis',(0.,0.,1.));
#27269=DIRECTION('center_axis',(0.,0.1971133419404,0.980380706883345));
#27270=DIRECTION('ref_axis',(0.,0.980380706883345,-0.1971133419404));
#27271=DIRECTION('center_axis',(0.,1.,0.));
#27272=DIRECTION('ref_axis',(-0.707106781186548,0.,0.707106781186547));
#27273=DIRECTION('center_axis',(-1.,0.,0.));
#27274=DIRECTION('ref_axis',(0.,-0.634380819689755,-0.773020682523925));
#27275=DIRECTION('center_axis',(1.,0.,0.));
#27276=DIRECTION('ref_axis',(0.,-0.634380819689755,-0.773020682523925));
#27277=DIRECTION('',(-1.,0.,0.));
#27278=DIRECTION('center_axis',(1.,0.,0.));
#27279=DIRECTION('ref_axis',(0.,0.773020682523925,0.634380819689755));
#27280=DIRECTION('',(1.,0.,0.));
#27281=DIRECTION('center_axis',(0.,0.,-1.));
#27282=DIRECTION('ref_axis',(0.,1.,0.));
#27283=DIRECTION('',(0.,1.,0.));
#27284=DIRECTION('',(-1.,0.,0.));
#27285=DIRECTION('center_axis',(0.,1.,0.));
#27286=DIRECTION('ref_axis',(-0.707106781186548,0.,0.707106781186547));
#27287=DIRECTION('',(0.,-1.,0.));
#27288=DIRECTION('center_axis',(0.,-1.,-4.44089209850063E-15));
#27289=DIRECTION('ref_axis',(-1.,0.,0.));
#27290=DIRECTION('center_axis',(1.,0.,0.));
#27291=DIRECTION('ref_axis',(0.,0.,-1.));
#27292=DIRECTION('center_axis',(1.,0.,0.));
#27293=DIRECTION('ref_axis',(0.,-0.999895356874024,-0.0144663506721044));
#27294=DIRECTION('center_axis',(1.,0.,0.));
#27295=DIRECTION('ref_axis',(0.,0.,-1.));
#27296=DIRECTION('center_axis',(-1.,0.,0.));
#27297=DIRECTION('ref_axis',(0.,-1.,-1.22464679914735E-16));
#27298=DIRECTION('',(0.,1.,0.));
#27299=DIRECTION('center_axis',(1.,0.,0.));
#27300=DIRECTION('ref_axis',(0.,-0.773020682523927,0.634380819689752));
#27301=DIRECTION('center_axis',(-0.134022231386924,-0.938793849576159,0.317339171064724));
#27302=DIRECTION('ref_axis',(-0.365244538597589,0.344479473986441,0.864829647402689));
#27303=DIRECTION('center_axis',(-1.,0.,0.));
#27304=DIRECTION('ref_axis',(0.,0.634380819689754,0.773020682523925));
#27305=DIRECTION('center_axis',(0.,0.,1.));
#27306=DIRECTION('ref_axis',(1.,0.,0.));
#27307=DIRECTION('center_axis',(-1.,0.,0.));
#27308=DIRECTION('ref_axis',(0.,0.777986605215495,-0.628280862437548));
#27309=DIRECTION('center_axis',(0.,0.977588190579301,0.210526315789473));
#27310=DIRECTION('ref_axis',(0.,-0.210526315789474,0.977588190579301));
#27311=DIRECTION('center_axis',(1.,0.,0.));
#27312=DIRECTION('ref_axis',(0.,0.777986605215496,-0.628280862437547));
#27313=DIRECTION('',(1.,0.,0.));
#27314=DIRECTION('',(-1.,0.,0.));
#27315=DIRECTION('center_axis',(0.,-1.,1.58603289232165E-16));
#27316=DIRECTION('ref_axis',(0.,-1.58603289232165E-16,-1.));
#27317=DIRECTION('',(-1.,0.,0.));
#27318=DIRECTION('',(0.,-1.58603289232165E-16,-1.));
#27319=DIRECTION('center_axis',(-1.,0.,0.));
#27320=DIRECTION('ref_axis',(0.,0.634380819689755,0.773020682523925));
#27321=DIRECTION('center_axis',(-1.,0.,0.));
#27322=DIRECTION('ref_axis',(0.,0.634380819689755,0.773020682523925));
#27323=DIRECTION('center_axis',(0.,0.,1.));
#27324=DIRECTION('ref_axis',(-0.772461049429072,-0.63506214429372,0.));
#27325=DIRECTION('center_axis',(-0.700067241886871,0.,-0.714076926414031));
#27326=DIRECTION('ref_axis',(0.,-1.,0.));
#27327=DIRECTION('center_axis',(0.,1.58603289232165E-16,1.));
#27328=DIRECTION('ref_axis',(-0.707106781186548,-0.707106781186547,0.));
#27329=DIRECTION('center_axis',(-0.700212217664035,0.,-0.713934766091423));
#27330=DIRECTION('ref_axis',(0.,-1.,0.));
#27331=DIRECTION('center_axis',(1.,0.,0.));
#27332=DIRECTION('ref_axis',(0.,-0.634380819689754,0.773020682523926));
#27333=DIRECTION('center_axis',(1.,0.,0.));
#27334=DIRECTION('ref_axis',(0.,0.195121951219513,0.980778988433322));
#27335=DIRECTION('',(1.,0.,0.));
#27336=DIRECTION('center_axis',(-1.,0.,0.));
#27337=DIRECTION('ref_axis',(0.,-0.634380819689754,0.773020682523926));
#27338=DIRECTION('center_axis',(1.,0.,0.));
#27339=DIRECTION('ref_axis',(0.,-1.22464679914735E-16,1.));
#27340=DIRECTION('center_axis',(1.,0.,0.));
#27341=DIRECTION('ref_axis',(0.,6.12323399573676E-17,1.));
#27342=DIRECTION('center_axis',(0.134022265816183,-0.938793848267554,-0.317339160395456));
#27343=DIRECTION('ref_axis',(-0.365244628135662,-0.344479477552722,0.864829608167439));
#27344=DIRECTION('center_axis',(0.,1.,-1.58603289232165E-16));
#27345=DIRECTION('ref_axis',(0.,1.58603289232165E-16,1.));
#27346=DIRECTION('',(0.,1.58603289232165E-16,1.));
#27347=DIRECTION('',(-1.,0.,0.));
#27348=DIRECTION('',(0.,1.58603289232165E-16,1.));
#27349=DIRECTION('center_axis',(0.,1.58603289232165E-16,1.));
#27350=DIRECTION('ref_axis',(-0.707106781186548,-0.707106781186548,0.));
#27351=DIRECTION('',(0.,-1.58603289232165E-16,-1.));
#27352=DIRECTION('center_axis',(0.,0.,1.));
#27353=DIRECTION('ref_axis',(-1.,0.,0.));
#27354=DIRECTION('center_axis',(-1.,0.,0.));
#27355=DIRECTION('ref_axis',(0.,0.,1.));
#27356=DIRECTION('',(0.,1.,0.));
#27357=DIRECTION('center_axis',(-1.,0.,0.));
#27358=DIRECTION('ref_axis',(0.,0.714764027971838,0.699365701416271));
#27359=DIRECTION('center_axis',(0.,-1.,0.));
#27360=DIRECTION('ref_axis',(-0.707106781186548,0.,-0.707106781186547));
#27361=DIRECTION('',(0.,-1.,0.));
#27362=DIRECTION('center_axis',(0.,1.,0.));
#27363=DIRECTION('ref_axis',(2.22044604925031E-15,0.,-1.));
#27364=DIRECTION('center_axis',(0.336615931322928,-0.848909755674504,0.407482443180381));
#27365=DIRECTION('ref_axis',(-0.540654873563249,-0.528537819574587,-0.654476952208134));
#27366=DIRECTION('center_axis',(-1.,0.,0.));
#27367=DIRECTION('ref_axis',(0.,-0.628280862437545,-0.777986605215498));
#27368=DIRECTION('center_axis',(0.,0.210526315789474,-0.977588190579301));
#27369=DIRECTION('ref_axis',(0.,0.977588190579301,0.210526315789474));
#27370=DIRECTION('center_axis',(1.,0.,0.));
#27371=DIRECTION('ref_axis',(0.,0.,-1.));
#27372=DIRECTION('center_axis',(1.,0.,0.));
#27373=DIRECTION('ref_axis',(0.,-1.60812264967664E-16,-1.));
#27374=DIRECTION('center_axis',(1.,0.,0.));
#27375=DIRECTION('ref_axis',(0.,0.,-1.));
#27376=DIRECTION('center_axis',(1.,0.,0.));
#27377=DIRECTION('ref_axis',(0.,0.634380819689754,-0.773020682523926));
#27378=DIRECTION('',(0.,-3.17206578464331E-16,-1.));
#27379=DIRECTION('center_axis',(-1.,0.,0.));
#27380=DIRECTION('ref_axis',(0.,-1.60812264967664E-16,-1.));
#27381=DIRECTION('',(0.,3.17206578464331E-16,1.));
#27382=DIRECTION('center_axis',(-1.,0.,0.));
#27383=DIRECTION('ref_axis',(0.,-1.22464679914735E-16,-1.));
#27384=DIRECTION('center_axis',(1.,0.,0.));
#27385=DIRECTION('ref_axis',(0.,-1.60812264967664E-16,-1.));
#27386=DIRECTION('center_axis',(1.,0.,0.));
#27387=DIRECTION('ref_axis',(0.,0.,-1.));
#27388=DIRECTION('center_axis',(1.,0.,0.));
#27389=DIRECTION('ref_axis',(0.,0.714764027971838,0.699365701416271));
#27390=DIRECTION('center_axis',(0.,0.9775881905793,-0.210526315789475));
#27391=DIRECTION('ref_axis',(0.,-0.210526315789475,-0.9775881905793));
#27392=DIRECTION('center_axis',(1.,0.,0.));
#27393=DIRECTION('ref_axis',(0.,-0.628280862437546,-0.777986605215497));
#27394=DIRECTION('',(1.,0.,0.));
#27395=DIRECTION('',(-1.,0.,0.));
#27396=DIRECTION('center_axis',(-1.,0.,0.));
#27397=DIRECTION('ref_axis',(0.,0.,1.));
#27398=DIRECTION('center_axis',(1.,0.,0.));
#27399=DIRECTION('ref_axis',(0.,0.99994072112783,-0.0108882611263663));
#27400=DIRECTION('center_axis',(0.,0.,1.));
#27401=DIRECTION('ref_axis',(-0.70710678118655,0.707106781186545,0.));
#27402=DIRECTION('center_axis',(-1.,0.,0.));
#27403=DIRECTION('ref_axis',(0.,-0.777986605215498,-0.628280862437545));
#27404=DIRECTION('center_axis',(-1.,0.,0.));
#27405=DIRECTION('ref_axis',(0.,-0.777986605215497,-0.628280862437546));
#27406=DIRECTION('',(1.,0.,0.));
#27407=DIRECTION('center_axis',(1.,0.,0.));
#27408=DIRECTION('ref_axis',(0.,1.,0.));
#27409=DIRECTION('',(-1.,0.,0.));
#27410=DIRECTION('',(-1.,0.,0.));
#27411=DIRECTION('center_axis',(-1.,0.,0.));
#27412=DIRECTION('ref_axis',(0.,0.715194520129579,0.698925459814293));
#27413=DIRECTION('',(-1.,0.,0.));
#27414=DIRECTION('',(-1.,0.,0.));
#27415=DIRECTION('center_axis',(-1.,0.,0.));
#27416=DIRECTION('ref_axis',(0.,-0.698925459814292,0.71519452012958));
#27417=DIRECTION('',(-1.,0.,0.));
#27418=DIRECTION('',(-1.,0.,0.));
#27419=DIRECTION('center_axis',(1.,0.,0.));
#27420=DIRECTION('ref_axis',(0.,-1.,-1.22464679914735E-16));
#27421=DIRECTION('',(1.,0.,0.));
#27422=DIRECTION('center_axis',(1.,0.,0.));
#27423=DIRECTION('ref_axis',(0.,-0.707106781186547,0.707106781186548));
#27424=DIRECTION('center_axis',(1.,0.,0.));
#27425=DIRECTION('ref_axis',(0.,6.12323399573677E-17,1.));
#27426=DIRECTION('',(-1.,0.,0.));
#27427=DIRECTION('center_axis',(1.,0.,0.));
#27428=DIRECTION('ref_axis',(0.,0.707106781186547,-0.707106781186548));
#27429=DIRECTION('',(1.,0.,0.));
#27430=DIRECTION('',(-1.,0.,0.));
#27431=DIRECTION('center_axis',(1.,0.,0.));
#27432=DIRECTION('ref_axis',(0.,-0.716797558008402,-0.697281335497511));
#27433=DIRECTION('',(-1.,0.,0.));
#27434=DIRECTION('center_axis',(1.,0.,0.));
#27435=DIRECTION('ref_axis',(0.,-1.,-1.22464679914735E-16));
#27436=DIRECTION('',(1.,0.,0.));
#27437=DIRECTION('center_axis',(-1.,0.,0.));
#27438=DIRECTION('ref_axis',(0.,-0.707106781186547,-0.707106781186548));
#27439=DIRECTION('',(-1.,0.,0.));
#27440=DIRECTION('',(-1.,0.,0.));
#27441=DIRECTION('center_axis',(-1.,0.,0.));
#27442=DIRECTION('ref_axis',(0.,0.698925459814293,-0.71519452012958));
#27443=DIRECTION('center_axis',(1.,0.,0.));
#27444=DIRECTION('ref_axis',(0.,-0.996859054590094,-0.0791961191078487));
#27445=DIRECTION('',(1.,0.,0.));
#27446=DIRECTION('center_axis',(1.,0.,0.));
#27447=DIRECTION('ref_axis',(0.,0.,-1.));
#27448=DIRECTION('center_axis',(1.,0.,0.));
#27449=DIRECTION('ref_axis',(0.,0.698925459814293,-0.71519452012958));
#27450=DIRECTION('center_axis',(1.,0.,0.));
#27451=DIRECTION('ref_axis',(0.,0.,-1.));
#27452=DIRECTION('',(0.,0.707106781186548,-0.707106781186548));
#27453=DIRECTION('',(0.,0.707106781186548,0.707106781186548));
#27454=DIRECTION('',(0.,-0.707106781186548,0.707106781186548));
#27455=DIRECTION('center_axis',(1.,0.,0.));
#27456=DIRECTION('ref_axis',(0.,0.996859054590094,0.0791961191078482));
#27457=DIRECTION('',(1.,0.,0.));
#27458=DIRECTION('center_axis',(1.,0.,0.));
#27459=DIRECTION('ref_axis',(0.,0.,-1.));
#27460=DIRECTION('center_axis',(1.,0.,0.));
#27461=DIRECTION('ref_axis',(0.,-0.698925459814292,0.71519452012958));
#27462=DIRECTION('center_axis',(1.,0.,0.));
#27463=DIRECTION('ref_axis',(0.,0.,-1.));
#27464=DIRECTION('',(0.,-0.707106781186548,0.707106781186548));
#27465=DIRECTION('',(0.,-0.707106781186548,-0.707106781186547));
#27466=DIRECTION('',(0.,0.707106781186548,-0.707106781186547));
#27467=DIRECTION('center_axis',(-1.,0.,0.));
#27468=DIRECTION('ref_axis',(0.,0.62828086243754,-0.777986605215502));
#27469=DIRECTION('center_axis',(1.,0.,0.));
#27470=DIRECTION('ref_axis',(0.,0.,-1.));
#27471=DIRECTION('center_axis',(-4.34136367113112E-15,-0.977588190579299,
0.210526315789481));
#27472=DIRECTION('ref_axis',(0.,0.210526315789481,0.977588190579299));
#27473=DIRECTION('center_axis',(-1.,0.,0.));
#27474=DIRECTION('ref_axis',(0.,-0.716797558008402,-0.697281335497511));
#27475=DIRECTION('center_axis',(0.,0.,1.));
#27476=DIRECTION('ref_axis',(-0.707106781186549,0.707106781186546,0.));
#27477=DIRECTION('center_axis',(-1.,0.,0.));
#27478=DIRECTION('ref_axis',(0.,0.777986605215498,0.628280862437544));
#27479=DIRECTION('center_axis',(0.,3.17206578464331E-16,1.));
#27480=DIRECTION('ref_axis',(-0.707106781186548,0.707106781186547,0.));
#27481=DIRECTION('center_axis',(1.,0.,0.));
#27482=DIRECTION('ref_axis',(0.,0.628280862437546,0.777986605215497));
#27483=DIRECTION('',(1.,0.,0.));
#27484=DIRECTION('center_axis',(-1.,0.,0.));
#27485=DIRECTION('ref_axis',(0.,0.,1.));
#27486=DIRECTION('center_axis',(1.,0.,0.));
#27487=DIRECTION('ref_axis',(0.,0.,-1.));
#27488=DIRECTION('center_axis',(-1.,0.,0.));
#27489=DIRECTION('ref_axis',(0.,0.,1.));
#27490=DIRECTION('center_axis',(-1.,0.,0.));
#27491=DIRECTION('ref_axis',(0.,6.12323399573677E-17,1.));
#27492=DIRECTION('center_axis',(1.,0.,0.));
#27493=DIRECTION('ref_axis',(0.,0.,-1.));
#27494=DIRECTION('center_axis',(-1.,0.,0.));
#27495=DIRECTION('ref_axis',(0.,0.777986605215499,0.628280862437544));
#27496=DIRECTION('',(-1.,0.,0.));
#27497=DIRECTION('center_axis',(0.,-3.17206578464331E-16,-1.));
#27498=DIRECTION('ref_axis',(-0.707106781186548,0.707106781186548,0.));
#27499=DIRECTION('',(0.,-3.17206578464331E-16,-1.));
#27500=DIRECTION('center_axis',(0.,0.,1.));
#27501=DIRECTION('ref_axis',(2.22044604925031E-15,1.,0.));
#27502=DIRECTION('',(0.,3.17206578464331E-16,1.));
#27503=DIRECTION('center_axis',(0.472949929361147,-0.380667016315068,-0.794613734469189));
#27504=DIRECTION('ref_axis',(-0.619013384421907,0.498230285022508,-0.607115320999995));
#27505=DIRECTION('center_axis',(-1.,0.,0.));
#27506=DIRECTION('ref_axis',(0.,0.634380819689754,-0.773020682523926));
#27507=DIRECTION('center_axis',(1.,0.,0.));
#27508=DIRECTION('ref_axis',(0.,0.634380819689754,-0.773020682523926));
#27509=DIRECTION('',(1.,0.,0.));
#27510=DIRECTION('center_axis',(0.,-1.,3.17206578464331E-16));
#27511=DIRECTION('ref_axis',(0.,-3.17206578464331E-16,-1.));
#27512=DIRECTION('center_axis',(1.,0.,0.));
#27513=DIRECTION('ref_axis',(0.,0.,-1.));
#27514=DIRECTION('center_axis',(1.,0.,0.));
#27515=DIRECTION('ref_axis',(0.,0.707106781186547,-0.707106781186548));
#27516=DIRECTION('center_axis',(-1.,0.,0.));
#27517=DIRECTION('ref_axis',(0.,0.707106781186547,-0.707106781186548));
#27518=DIRECTION('center_axis',(-1.,0.,0.));
#27519=DIRECTION('ref_axis',(0.,0.,1.));
#27520=DIRECTION('',(0.,-3.17206578464331E-16,-1.));
#27521=DIRECTION('center_axis',(-1.,0.,0.));
#27522=DIRECTION('ref_axis',(0.,0.707106781186547,-0.707106781186548));
#27523=DIRECTION('center_axis',(0.,3.17206578464331E-16,1.));
#27524=DIRECTION('ref_axis',(-0.707106781186548,-0.707106781186548,0.));
#27525=DIRECTION('',(0.,3.17206578464331E-16,1.));
#27526=DIRECTION('center_axis',(-4.44089209850062E-15,0.,1.));
#27527=DIRECTION('ref_axis',(0.,-1.,0.));
#27528=DIRECTION('center_axis',(0.,0.,1.));
#27529=DIRECTION('ref_axis',(1.,0.,0.));
#27530=DIRECTION('center_axis',(-1.,0.,0.));
#27531=DIRECTION('ref_axis',(0.,-0.210526315789473,0.977588190579301));
#27532=DIRECTION('center_axis',(0.,-0.977588190579299,-0.210526315789481));
#27533=DIRECTION('ref_axis',(-1.,0.,0.));
#27534=DIRECTION('center_axis',(0.336615931322922,-0.848909755674508,-0.407482443180376));
#27535=DIRECTION('ref_axis',(-0.540654873563252,-0.528537819574574,0.654476952208142));
#27536=DIRECTION('center_axis',(6.51204550669669E-15,0.210526315789473,
0.977588190579301));
#27537=DIRECTION('ref_axis',(0.,-0.977588190579301,0.210526315789473));
#27538=DIRECTION('center_axis',(-1.,0.,0.));
#27539=DIRECTION('ref_axis',(0.,0.,1.));
#27540=DIRECTION('center_axis',(-1.,0.,0.));
#27541=DIRECTION('ref_axis',(0.,-0.628280862437546,0.777986605215497));
#27542=DIRECTION('center_axis',(1.,0.,0.));
#27543=DIRECTION('ref_axis',(0.,0.,-1.));
#27544=DIRECTION('center_axis',(1.,0.,0.));
#27545=DIRECTION('ref_axis',(0.,-0.777986605215497,0.628280862437546));
#27546=DIRECTION('',(1.,0.,0.));
#27547=DIRECTION('center_axis',(0.,1.,-3.17206578464331E-16));
#27548=DIRECTION('ref_axis',(0.,3.17206578464331E-16,1.));
#27549=DIRECTION('center_axis',(-1.,0.,0.));
#27550=DIRECTION('ref_axis',(0.,0.,1.));
#27551=DIRECTION('center_axis',(1.,0.,0.));
#27552=DIRECTION('ref_axis',(0.,0.,-1.));
#27553=DIRECTION('center_axis',(1.,0.,0.));
#27554=DIRECTION('ref_axis',(0.,-0.773020682523927,0.634380819689752));
#27555=DIRECTION('',(0.,1.,0.));
#27556=DIRECTION('center_axis',(-1.,0.,0.));
#27557=DIRECTION('ref_axis',(0.,-0.773020682523927,0.634380819689752));
#27558=DIRECTION('',(-1.,0.,0.));
#27559=DIRECTION('center_axis',(0.,0.,-1.));
#27560=DIRECTION('ref_axis',(0.,1.,0.));
#27561=DIRECTION('center_axis',(1.,0.,0.));
#27562=DIRECTION('ref_axis',(0.,0.0791961191078487,-0.996859054590094));
#27563=DIRECTION('',(1.,0.,0.));
#27564=DIRECTION('center_axis',(0.,-0.707106781186548,0.707106781186548));
#27565=DIRECTION('ref_axis',(0.,-0.707106781186548,-0.707106781186548));
#27566=DIRECTION('',(0.,-0.707106781186548,-0.707106781186548));
#27567=DIRECTION('',(1.,0.,0.));
#27568=DIRECTION('',(0.,0.707106781186548,0.707106781186548));
#27569=DIRECTION('',(1.,0.,0.));
#27570=DIRECTION('center_axis',(1.,0.,0.));
#27571=DIRECTION('ref_axis',(0.,0.,-1.));
#27572=DIRECTION('center_axis',(1.,0.,0.));
#27573=DIRECTION('ref_axis',(0.,0.71519452012958,0.698925459814293));
#27574=DIRECTION('center_axis',(1.,0.,0.));
#27575=DIRECTION('ref_axis',(0.,0.,-1.));
#27576=DIRECTION('',(0.,0.707106781186548,0.707106781186548));
#27577=DIRECTION('',(0.,-0.707106781186548,0.707106781186548));
#27578=DIRECTION('center_axis',(1.,0.,0.));
#27579=DIRECTION('ref_axis',(0.,0.,-1.));
#27580=DIRECTION('center_axis',(-1.,0.,0.));
#27581=DIRECTION('ref_axis',(0.,-1.,3.06161699786838E-17));
#27582=DIRECTION('center_axis',(-1.,0.,0.));
#27583=DIRECTION('ref_axis',(0.,-1.,3.06161699786838E-17));
#27584=DIRECTION('center_axis',(0.,-1.,-1.22464679914735E-16));
#27585=DIRECTION('ref_axis',(0.,-1.22464679914735E-16,1.));
#27586=DIRECTION('center_axis',(-1.,0.,0.));
#27587=DIRECTION('ref_axis',(0.,1.,0.));
#27588=DIRECTION('center_axis',(1.,0.,0.));
#27589=DIRECTION('ref_axis',(0.,-1.,3.06161699786838E-17));
#27590=DIRECTION('',(-0.707106781186548,-0.707106781186548,-8.65956056235493E-17));
#27591=DIRECTION('center_axis',(1.,0.,0.));
#27592=DIRECTION('ref_axis',(0.,-1.,3.06161699786838E-17));
#27593=DIRECTION('center_axis',(1.,0.,0.));
#27594=DIRECTION('ref_axis',(0.,-1.,3.06161699786838E-17));
#27595=DIRECTION('center_axis',(1.,0.,0.));
#27596=DIRECTION('ref_axis',(0.,-1.,3.06161699786838E-17));
#27597=DIRECTION('center_axis',(-1.,0.,0.));
#27598=DIRECTION('ref_axis',(0.,-0.0791961191078482,-0.996859054590094));
#27599=DIRECTION('',(-1.,0.,0.));
#27600=DIRECTION('center_axis',(0.,0.707106781186548,0.707106781186548));
#27601=DIRECTION('ref_axis',(0.,-0.707106781186548,0.707106781186548));
#27602=DIRECTION('',(-1.,0.,0.));
#27603=DIRECTION('',(0.,-0.707106781186548,0.707106781186548));
#27604=DIRECTION('',(1.,0.,0.));
#27605=DIRECTION('center_axis',(-1.,0.,0.));
#27606=DIRECTION('ref_axis',(0.,-0.996859054590094,0.0791961191078482));
#27607=DIRECTION('',(-1.,0.,0.));
#27608=DIRECTION('center_axis',(0.,0.707106781186548,-0.707106781186548));
#27609=DIRECTION('ref_axis',(0.,0.707106781186548,0.707106781186548));
#27610=DIRECTION('',(-1.,0.,0.));
#27611=DIRECTION('',(0.,0.707106781186547,0.707106781186547));
#27612=DIRECTION('',(1.,0.,0.));
#27613=DIRECTION('center_axis',(-1.,0.,0.));
#27614=DIRECTION('ref_axis',(0.,0.0791961191078487,0.996859054590094));
#27615=DIRECTION('',(-1.,0.,0.));
#27616=DIRECTION('center_axis',(0.,-0.707106781186548,-0.707106781186548));
#27617=DIRECTION('ref_axis',(0.,0.707106781186548,-0.707106781186548));
#27618=DIRECTION('',(-1.,0.,0.));
#27619=DIRECTION('',(0.,0.707106781186548,-0.707106781186548));
#27620=DIRECTION('',(1.,0.,0.));
#27621=DIRECTION('center_axis',(0.,-0.707106781186547,-0.707106781186548));
#27622=DIRECTION('ref_axis',(0.707106781186544,-0.500000000000003,0.500000000000002));
#27623=DIRECTION('',(0.,0.707106781186547,0.707106781186548));
#27624=DIRECTION('center_axis',(0.,-0.707106781186548,-0.707106781186548));
#27625=DIRECTION('ref_axis',(1.,0.,0.));
#27626=DIRECTION('',(0.,-0.707106781186547,-0.707106781186548));
#27627=DIRECTION('center_axis',(0.,-1.,-6.28036983473513E-15));
#27628=DIRECTION('ref_axis',(-1.96261557335473E-16,-6.31439345255561E-15,
1.));
#27629=DIRECTION('center_axis',(1.,0.,0.));
#27630=DIRECTION('ref_axis',(0.,0.,-1.));
#27631=DIRECTION('center_axis',(-1.,0.,0.));
#27632=DIRECTION('ref_axis',(0.,0.0115039628724714,-0.999933827229697));
#27633=DIRECTION('center_axis',(0.,0.809885237104279,-0.586588358834836));
#27634=DIRECTION('ref_axis',(0.,0.586588358834836,0.809885237104279));
#27635=DIRECTION('center_axis',(1.,0.,0.));
#27636=DIRECTION('ref_axis',(0.,0.0115039628724714,-0.999933827229697));
#27637=DIRECTION('center_axis',(-0.0364266962331357,-0.997807365125386,
-0.055259007438373));
#27638=DIRECTION('ref_axis',(0.549169647365281,-0.0661850595039047,0.833085971740707));
#27639=DIRECTION('center_axis',(1.,0.,0.));
#27640=DIRECTION('ref_axis',(0.,-0.0791961191078493,0.996859054590094));
#27641=DIRECTION('center_axis',(1.,0.,0.));
#27642=DIRECTION('ref_axis',(0.,-0.0791961191078487,0.996859054590094));
#27643=DIRECTION('',(-1.,0.,0.));
#27644=DIRECTION('',(1.,0.,0.));
#27645=DIRECTION('center_axis',(1.,0.,0.));
#27646=DIRECTION('ref_axis',(0.,1.,0.));
#27647=DIRECTION('center_axis',(1.,0.,0.));
#27648=DIRECTION('ref_axis',(0.,0.,-1.));
#27649=DIRECTION('center_axis',(-1.,0.,0.));
#27650=DIRECTION('ref_axis',(0.,-1.,1.83697019872103E-16));
#27651=DIRECTION('center_axis',(0.,0.707106781186548,-0.707106781186548));
#27652=DIRECTION('ref_axis',(0.,0.707106781186548,0.707106781186548));
#27653=DIRECTION('',(1.,0.,0.));
#27654=DIRECTION('center_axis',(1.,0.,0.));
#27655=DIRECTION('ref_axis',(0.,0.,-1.));
#27656=DIRECTION('center_axis',(-1.,0.,0.));
#27657=DIRECTION('ref_axis',(0.,-1.,1.83697019872103E-16));
#27658=DIRECTION('center_axis',(1.,0.,0.));
#27659=DIRECTION('ref_axis',(0.,0.,-1.));
#27660=DIRECTION('',(0.,0.707106781186548,-0.707106781186548));
#27661=DIRECTION('center_axis',(1.,0.,0.));
#27662=DIRECTION('ref_axis',(0.,1.,-2.83276944882399E-16));
#27663=DIRECTION('center_axis',(1.,0.,0.));
#27664=DIRECTION('ref_axis',(0.,0.,-1.));
#27665=DIRECTION('center_axis',(-1.,0.,0.));
#27666=DIRECTION('ref_axis',(0.,1.,-2.83276944882399E-16));
#27667=DIRECTION('center_axis',(0.,0.707106781186548,0.707106781186548));
#27668=DIRECTION('ref_axis',(0.,-0.707106781186548,0.707106781186548));
#27669=DIRECTION('center_axis',(1.,0.,0.));
#27670=DIRECTION('ref_axis',(0.,1.22464679914735E-16,1.));
#27671=DIRECTION('center_axis',(-1.,0.,0.));
#27672=DIRECTION('ref_axis',(0.,-1.,1.83697019872103E-16));
#27673=DIRECTION('center_axis',(1.,0.,0.));
#27674=DIRECTION('ref_axis',(0.,0.,-1.));
#27675=DIRECTION('center_axis',(1.,0.,0.));
#27676=DIRECTION('ref_axis',(0.,1.22464679914735E-16,1.));
#27677=DIRECTION('center_axis',(1.,0.,0.));
#27678=DIRECTION('ref_axis',(0.,-1.22464679914735E-16,1.));
#27679=DIRECTION('center_axis',(-1.,0.,0.));
#27680=DIRECTION('ref_axis',(0.,1.22464679914735E-16,1.));
#27681=DIRECTION('center_axis',(0.,-0.707106781186547,0.707106781186548));
#27682=DIRECTION('ref_axis',(0.,-0.707106781186548,-0.707106781186547));
#27683=DIRECTION('',(1.,0.,0.));
#27684=DIRECTION('center_axis',(1.,0.,0.));
#27685=DIRECTION('ref_axis',(0.,0.,-1.));
#27686=DIRECTION('',(0.,-0.707106781186548,0.707106781186547));
#27687=DIRECTION('center_axis',(-1.,0.,0.));
#27688=DIRECTION('ref_axis',(0.,-1.,1.83697019872103E-16));
#27689=DIRECTION('',(0.,-0.707106781186548,-0.707106781186548));
#27690=DIRECTION('center_axis',(1.,0.,0.));
#27691=DIRECTION('ref_axis',(0.,-0.999933827229697,0.0115039628724727));
#27692=DIRECTION('center_axis',(1.,0.,0.));
#27693=DIRECTION('ref_axis',(0.,0.,-1.));
#27694=DIRECTION('center_axis',(0.,-0.586588358834838,0.809885237104277));
#27695=DIRECTION('ref_axis',(1.,0.,0.));
#27696=DIRECTION('center_axis',(-1.,0.,0.));
#27697=DIRECTION('ref_axis',(0.,-0.999933827229697,0.0115039628724727));
#27698=DIRECTION('center_axis',(0.,0.707106781186548,0.707106781186548));
#27699=DIRECTION('ref_axis',(0.707106781186547,0.500000000000001,-0.5));
#27700=DIRECTION('center_axis',(0.,3.14018491736755E-15,-1.));
#27701=DIRECTION('ref_axis',(-1.47196168001603E-16,1.,3.12250225675824E-15));
#27702=DIRECTION('',(0.,0.707106781186548,0.707106781186548));
#27703=DIRECTION('center_axis',(0.,-0.707106781186543,-0.707106781186552));
#27704=DIRECTION('ref_axis',(0.,0.707106781186552,-0.707106781186543));
#27705=DIRECTION('center_axis',(0.,0.,1.));
#27706=DIRECTION('ref_axis',(1.,0.,0.));
#27707=DIRECTION('center_axis',(1.,0.,0.));
#27708=DIRECTION('ref_axis',(0.,0.996859054590094,-0.0791961191078493));
#27709=DIRECTION('center_axis',(1.,0.,0.));
#27710=DIRECTION('ref_axis',(0.,-0.999933827229697,0.0115039628724726));
#27711=DIRECTION('',(1.,0.,0.));
#27712=DIRECTION('',(1.,0.,0.));
#27713=DIRECTION('center_axis',(-1.,0.,0.));
#27714=DIRECTION('ref_axis',(0.,0.996859054590094,-0.0791961191078487));
#27715=DIRECTION('',(-1.,0.,0.));
#27716=DIRECTION('center_axis',(0.,-0.707106781186548,0.707106781186548));
#27717=DIRECTION('ref_axis',(0.,-0.707106781186548,-0.707106781186548));
#27718=DIRECTION('',(1.,0.,0.));
#27719=DIRECTION('',(0.,-0.707106781186548,-0.707106781186548));
#27720=DIRECTION('',(-1.,0.,0.));
#27721=DIRECTION('center_axis',(0.,-0.707106781186548,0.707106781186548));
#27722=DIRECTION('ref_axis',(-0.707106781186547,-0.5,-0.5));
#27723=DIRECTION('',(1.,0.,0.));
#27724=DIRECTION('center_axis',(0.,-0.707106781186548,0.707106781186548));
#27725=DIRECTION('ref_axis',(0.707106781186547,-0.5,-0.5));
#27726=DIRECTION('center_axis',(1.,0.,0.));
#27727=DIRECTION('ref_axis',(0.,0.,-1.));
#27728=DIRECTION('center_axis',(0.,-0.707106781186547,0.707106781186548));
#27729=DIRECTION('ref_axis',(0.707106781186547,0.5,0.5));
#27730=DIRECTION('',(0.,-0.707106781186547,0.707106781186548));
#27731=DIRECTION('center_axis',(0.,0.707106781186548,-0.707106781186547));
#27732=DIRECTION('ref_axis',(0.,0.707106781186547,0.707106781186548));
#27733=DIRECTION('center_axis',(0.,0.707106781186548,-0.707106781186547));
#27734=DIRECTION('ref_axis',(0.707106781186547,-0.5,-0.5));
#27735=DIRECTION('',(1.,0.,0.));
#27736=DIRECTION('center_axis',(0.,0.707106781186548,-0.707106781186547));
#27737=DIRECTION('ref_axis',(-0.707106781186547,-0.5,-0.5));
#27738=DIRECTION('',(1.,0.,0.));
#27739=DIRECTION('',(0.,0.707106781186547,0.707106781186548));
#27740=DIRECTION('',(1.,0.,0.));
#27741=DIRECTION('center_axis',(0.,-0.707106781186548,-0.707106781186547));
#27742=DIRECTION('ref_axis',(0.,0.707106781186547,-0.707106781186548));
#27743=DIRECTION('',(0.,0.707106781186547,-0.707106781186548));
#27744=DIRECTION('center_axis',(0.,-0.707106781186548,0.707106781186548));
#27745=DIRECTION('ref_axis',(-0.707106781186547,-0.5,-0.5));
#27746=DIRECTION('',(0.,-0.707106781186548,0.707106781186548));
#27747=DIRECTION('center_axis',(0.,0.707106781186548,0.707106781186548));
#27748=DIRECTION('ref_axis',(0.,-0.707106781186548,0.707106781186548));
#27749=DIRECTION('',(0.,0.707106781186548,-0.707106781186548));
#27750=DIRECTION('center_axis',(0.,0.707106781186548,-0.707106781186548));
#27751=DIRECTION('ref_axis',(0.707106781186547,-0.5,-0.5));
#27752=DIRECTION('center_axis',(-1.,0.,0.));
#27753=DIRECTION('ref_axis',(0.,0.996859054590094,-0.0791961191078487));
#27754=DIRECTION('center_axis',(1.,0.,0.));
#27755=DIRECTION('ref_axis',(0.,-0.0791961191078487,0.996859054590094));
#27756=DIRECTION('center_axis',(1.,0.,0.));
#27757=DIRECTION('ref_axis',(0.,0.,-1.));
#27758=DIRECTION('center_axis',(1.,0.,0.));
#27759=DIRECTION('ref_axis',(0.,-0.707106781186548,-0.707106781186548));
#27760=DIRECTION('center_axis',(1.,0.,0.));
#27761=DIRECTION('ref_axis',(0.,0.,-1.));
#27762=DIRECTION('center_axis',(0.,-0.707106781186547,-0.707106781186548));
#27763=DIRECTION('ref_axis',(0.,0.707106781186548,-0.707106781186547));
#27764=DIRECTION('center_axis',(0.,0.707106781186548,0.707106781186548));
#27765=DIRECTION('ref_axis',(0.,-0.707106781186548,0.707106781186548));
#27766=DIRECTION('',(1.,0.,0.));
#27767=DIRECTION('center_axis',(1.,0.,0.));
#27768=DIRECTION('ref_axis',(0.,1.,0.));
#27769=DIRECTION('center_axis',(1.,0.,0.));
#27770=DIRECTION('ref_axis',(0.,1.,0.));
#27771=DIRECTION('center_axis',(0.,0.,1.));
#27772=DIRECTION('ref_axis',(0.,-1.,0.));
#27773=DIRECTION('center_axis',(1.,0.,0.));
#27774=DIRECTION('ref_axis',(0.,1.,0.));
#27775=DIRECTION('center_axis',(1.,0.,0.));
#27776=DIRECTION('ref_axis',(0.,1.,0.));
#27777=DIRECTION('',(0.,1.,0.));
#27778=DIRECTION('',(0.,0.,1.));
#27779=DIRECTION('',(0.,1.,0.));
#27780=DIRECTION('',(0.,0.,1.));
#27781=DIRECTION('',(-0.125333233564305,-0.992114701314478,0.));
#27782=DIRECTION('',(0.,0.,1.));
#27783=DIRECTION('',(-0.0836778433323145,0.996492859249504,0.));
#27784=DIRECTION('',(0.,0.,1.));
#27785=DIRECTION('',(0.289031796944471,-0.957319497532068,0.));
#27786=DIRECTION('',(0.,0.,1.));
#27787=DIRECTION('',(0.,1.,0.));
#27788=DIRECTION('',(0.,0.,1.));
#27789=DIRECTION('',(0.,1.,0.));
#27790=DIRECTION('',(0.,0.,1.));
#27791=DIRECTION('',(0.,1.,0.));
#27792=DIRECTION('',(0.,0.,1.));
#27793=DIRECTION('',(-0.908282142847613,-0.418358158739791,0.));
#27794=DIRECTION('',(0.,0.,1.));
#27795=DIRECTION('',(0.418358158739791,-0.908282142847613,0.));
#27796=DIRECTION('',(0.,0.,1.));
#27797=DIRECTION('',(0.908282142847613,0.41835815873979,0.));
#27798=DIRECTION('',(0.,0.,1.));
#27799=DIRECTION('',(-0.418358158739791,0.908282142847614,0.));
#27800=DIRECTION('',(0.,0.,1.));
#27801=DIRECTION('',(0.,1.,0.));
#27802=DIRECTION('',(0.,0.,1.));
#27803=DIRECTION('',(0.,1.,0.));
#27804=DIRECTION('',(0.,0.,1.));
#27805=DIRECTION('',(0.,1.,0.));
#27806=DIRECTION('',(0.,0.,1.));
#27807=DIRECTION('',(0.,1.,0.));
#27808=DIRECTION('',(0.,0.,1.));
#27809=DIRECTION('',(0.,1.,0.));
#27810=DIRECTION('',(0.,0.,1.));
#27811=DIRECTION('',(0.,1.,0.));
#27812=DIRECTION('',(0.,0.,1.));
#27813=DIRECTION('',(0.,1.,0.));
#27814=DIRECTION('',(0.,0.,1.));
#27815=DIRECTION('',(0.,1.,0.));
#27816=DIRECTION('',(0.,0.,1.));
#27817=DIRECTION('',(0.,1.,0.));
#27818=DIRECTION('',(0.,0.,1.));
#27819=CARTESIAN_POINT('',(0.,0.,0.));
#27820=CARTESIAN_POINT('',(0.,0.,0.));
#27821=CARTESIAN_POINT('Origin',(29.75,0.,0.));
#27822=CARTESIAN_POINT('',(32.1628916636063,-6.92198924261957,-0.00637899664044927));
#27823=CARTESIAN_POINT('',(31.9835483363939,-6.9206415740836,-0.000329640349373658));
#27824=CARTESIAN_POINT('',(29.75,-6.933,-8.4904762584886E-16));
#27825=CARTESIAN_POINT('',(31.067,-4.95966987665981,-4.85170944379072));
#27826=CARTESIAN_POINT('Ctrl Pts',(32.1628916636063,-6.92198924261957,-0.00637899664044927));
#27827=CARTESIAN_POINT('Ctrl Pts',(32.1234269345577,-6.91442709372537,1.37132673071421));
#27828=CARTESIAN_POINT('Ctrl Pts',(32.0839622055092,-6.51430118721618,2.75348702170588));
#27829=CARTESIAN_POINT('Ctrl Pts',(32.0444974764607,-5.74807259775006,3.89182548507003));
#27830=CARTESIAN_POINT('Ctrl Pts',(32.0114122090537,-5.10570463048956,4.84615187646083));
#27831=CARTESIAN_POINT('Ctrl Pts',(31.9783269416467,-4.20602826637418,5.62911267424726));
#27832=CARTESIAN_POINT('Ctrl Pts',(31.9452416742396,-3.17855940282965,6.157422342539));
#27833=CARTESIAN_POINT('Ctrl Pts',(31.9121564068326,-2.15109053928511,6.68573201083074));
#27834=CARTESIAN_POINT('Ctrl Pts',(31.8790711394256,-0.995829176311432,
6.95939054962779));
#27835=CARTESIAN_POINT('Ctrl Pts',(31.8459858720186,0.153365723954005,6.93401243877144));
#27836=CARTESIAN_POINT('Ctrl Pts',(31.8129006046115,1.30256062421944,6.90863432791508));
#27837=CARTESIAN_POINT('Ctrl Pts',(31.7798153372045,2.44568906177664,6.58421956740534));
#27838=CARTESIAN_POINT('Ctrl Pts',(31.7467300697975,3.44866898595544,6.0108050971193));
#27839=CARTESIAN_POINT('Ctrl Pts',(31.7136448023905,4.45164891013425,5.43739062683326));
#27840=CARTESIAN_POINT('Ctrl Pts',(31.6805595349835,5.31448032093466,4.61497644677094));
#27841=CARTESIAN_POINT('Ctrl Pts',(31.6474742675765,5.91376424879513,3.63312504742053));
#27842=CARTESIAN_POINT('Ctrl Pts',(31.5813037327624,7.11233210451607,1.66942224871972));
#27843=CARTESIAN_POINT('Ctrl Pts',(31.5151331979484,7.25671002847726,-0.932029427133405));
#27844=CARTESIAN_POINT('Ctrl Pts',(31.4489626631344,6.26478062010639,-2.99981867537784));
#27845=CARTESIAN_POINT('Ctrl Pts',(31.3827921283203,5.27285121173552,-5.06760792362229));
#27846=CARTESIAN_POINT('Ctrl Pts',(31.3166215935063,3.14461447103258,-6.60173474425803));
#27847=CARTESIAN_POINT('Ctrl Pts',(31.2504510586922,0.869393195229573,-6.8908669450609));
#27848=CARTESIAN_POINT('Ctrl Pts',(31.1893007057948,-1.23321311324388,-7.15806345726668));
#27849=CARTESIAN_POINT('Ctrl Pts',(31.1281503528974,-3.46134732907935,-6.3620081845267));
#27850=CARTESIAN_POINT('Ctrl Pts',(31.067,-4.95966987665981,-4.85170944379072));
#27851=CARTESIAN_POINT('',(31.067,-6.933,-8.4904762584886E-16));
#27852=CARTESIAN_POINT('Origin',(31.067,0.,0.));
#27853=CARTESIAN_POINT('',(0.,-6.933,-8.4904762584886E-16));
#27854=CARTESIAN_POINT('',(29.75,-6.933,-8.4904762584886E-16));
#27855=CARTESIAN_POINT('',(0.,-6.60730572926666,-2.1));
#27856=CARTESIAN_POINT('Origin',(0.,0.,0.));
#27857=CARTESIAN_POINT('',(-16.,-6.60730572926666,-2.1));
#27858=CARTESIAN_POINT('',(29.75,-6.60730572926666,-2.1));
#27859=CARTESIAN_POINT('',(-16.,-6.933,-8.4904762584886E-16));
#27860=CARTESIAN_POINT('Origin',(-16.,0.,0.));
#27861=CARTESIAN_POINT('',(-49.48928,-6.933,8.4904762584886E-16));
#27862=CARTESIAN_POINT('',(29.75,-6.933,-8.4904762584886E-16));
#27863=CARTESIAN_POINT('Origin',(-49.48928,0.,0.));
#27864=CARTESIAN_POINT('',(-16.,-6.60730572926666,2.1));
#27865=CARTESIAN_POINT('Origin',(-16.,0.,0.));
#27866=CARTESIAN_POINT('',(0.,-6.60730572926666,2.1));
#27867=CARTESIAN_POINT('',(29.75,-6.60730572926666,2.1));
#27868=CARTESIAN_POINT('Origin',(0.,0.,0.));
#27869=CARTESIAN_POINT('',(31.067,0.728796816009639,-6.89458803707475));
#27870=CARTESIAN_POINT('Origin',(31.067,0.,0.));
#27871=CARTESIAN_POINT('Ctrl Pts',(31.067,0.728796816009639,-6.89458803707475));
#27872=CARTESIAN_POINT('Ctrl Pts',(31.100085267407,1.87539916180616,-6.77338570644206));
#27873=CARTESIAN_POINT('Ctrl Pts',(31.133170534814,2.9888184467541,-6.36193732933414));
#27874=CARTESIAN_POINT('Ctrl Pts',(31.166255802221,3.93811726940023,-5.70670201568804));
#27875=CARTESIAN_POINT('Ctrl Pts',(31.199341069628,4.88741609204636,-5.05146670204194));
#27876=CARTESIAN_POINT('Ctrl Pts',(31.2324263370351,5.67259445239068,-4.15244445185767));
#27877=CARTESIAN_POINT('Ctrl Pts',(31.2655116044421,6.19093045690171,-3.12438071542469));
#27878=CARTESIAN_POINT('Ctrl Pts',(31.2985968718491,6.70926646141273,-2.09631697899172));
#27879=CARTESIAN_POINT('Ctrl Pts',(31.3316821392561,6.96076011009046,-0.93921175631004));
#27880=CARTESIAN_POINT('Ctrl Pts',(31.3647674066631,6.92655811692062,0.214382199295643));
#27881=CARTESIAN_POINT('Ctrl Pts',(31.3978526740702,6.89235612375078,1.36797615490133));
#27882=CARTESIAN_POINT('Ctrl Pts',(31.4309379414772,6.57245848873336,2.51805884343103));
#27883=CARTESIAN_POINT('Ctrl Pts',(31.4640232088842,5.9879843556759,3.50963197083578));
#27884=CARTESIAN_POINT('Ctrl Pts',(31.5301937436983,4.81903608956097,5.49277822564526));
#27885=CARTESIAN_POINT('Ctrl Pts',(31.5963642785123,2.59178183128585,6.84188623595496));
#27886=CARTESIAN_POINT('Ctrl Pts',(31.6625348133263,0.300319744218148,6.93899847482886));
#27887=CARTESIAN_POINT('Ctrl Pts',(31.7287053481403,-1.99114234284955,7.03611071370276));
#27888=CARTESIAN_POINT('Ctrl Pts',(31.7948758829544,-4.34681225870981,5.88122718114086));
#27889=CARTESIAN_POINT('Ctrl Pts',(31.8610464177684,-5.67194850391824,4.00941248465481));
#27890=CARTESIAN_POINT('Ctrl Pts',(31.9018803906436,-6.48969280120721,2.85431179280679));
#27891=CARTESIAN_POINT('Ctrl Pts',(31.9427143635188,-6.91499447673405,1.42619300013786));
#27892=CARTESIAN_POINT('Ctrl Pts',(31.9835483363939,-6.9206415740836,-0.000329640349373658));
#27893=CARTESIAN_POINT('',(-16.,6.60730572926666,-2.1));
#27894=CARTESIAN_POINT('',(0.,6.60730572926666,-2.1));
#27895=CARTESIAN_POINT('',(29.75,6.60730572926666,-2.1));
#27896=CARTESIAN_POINT('',(0.,6.60730572926666,2.1));
#27897=CARTESIAN_POINT('Origin',(0.,0.,0.));
#27898=CARTESIAN_POINT('',(-16.,6.60730572926666,2.1));
#27899=CARTESIAN_POINT('',(29.75,6.60730572926666,2.1));
#27900=CARTESIAN_POINT('Origin',(-16.,0.,0.));
#27901=CARTESIAN_POINT('Origin',(29.75,0.,0.));
#27902=CARTESIAN_POINT('',(33.4128916636063,-6.93491738431276,-0.000440937362671394));
#27903=CARTESIAN_POINT('',(33.2335483363939,-6.94245604902185,-0.00577606699965401));
#27904=CARTESIAN_POINT('',(29.75,-6.933,-8.4904762584886E-16));
#27905=CARTESIAN_POINT('Ctrl Pts',(33.4128916636063,-6.94109895177657,-0.00186250112332087));
#27906=CARTESIAN_POINT('Ctrl Pts',(33.3868687441823,-6.93819580024513,0.904044259585895));
#27907=CARTESIAN_POINT('Ctrl Pts',(33.3608458247584,-6.75124710452186,1.81227878197669));
#27908=CARTESIAN_POINT('Ctrl Pts',(33.3348229053344,-6.40214532506429,2.65136988785769));
#27909=CARTESIAN_POINT('Ctrl Pts',(33.3017376379274,-5.95830097626352,3.718181538182));
#27910=CARTESIAN_POINT('Ctrl Pts',(33.2686523705204,-5.25234729975987,4.67322760256061));
#27911=CARTESIAN_POINT('Ctrl Pts',(33.2355671031134,-4.35830135115629,5.39541883541299));
#27912=CARTESIAN_POINT('Ctrl Pts',(33.2024818357063,-3.46425540255271,6.11761006826537));
#27913=CARTESIAN_POINT('Ctrl Pts',(33.1693965682993,-2.38211718184919,6.60694646959151));
#27914=CARTESIAN_POINT('Ctrl Pts',(33.1363113008923,-1.24582538897172,6.81653407868776));
#27915=CARTESIAN_POINT('Ctrl Pts',(33.1032260334853,-0.109533596094221,
7.026121687784));
#27916=CARTESIAN_POINT('Ctrl Pts',(33.0701407660783,1.08091176895724,6.95596050465035));
#27917=CARTESIAN_POINT('Ctrl Pts',(33.0370554986712,2.17244432217632,6.59294758082586));
#27918=CARTESIAN_POINT('Ctrl Pts',(32.9708849638572,4.35550942861445,5.86692173317689));
#27919=CARTESIAN_POINT('Ctrl Pts',(32.9047144290432,6.14292328772306,3.96948892276462));
#27920=CARTESIAN_POINT('Ctrl Pts',(32.8385438942291,6.72047556257529,1.75078263924961));
#27921=CARTESIAN_POINT('Ctrl Pts',(32.7723733594151,7.29802783742751,-0.467923644265391));
#27922=CARTESIAN_POINT('Ctrl Pts',(32.706202824601,6.66571852802333,-3.00790340088312));
#27923=CARTESIAN_POINT('Ctrl Pts',(32.640032289787,5.11290677397241,-4.6996294346094));
#27924=CARTESIAN_POINT('Ctrl Pts',(32.573861754973,3.5600950199215,-6.39135546833568));
#27925=CARTESIAN_POINT('Ctrl Pts',(32.507691220159,1.08678082122384,-7.23482777917051));
#27926=CARTESIAN_POINT('Ctrl Pts',(32.4415206853449,-1.17608958629167,-6.84435685493866));
#27927=CARTESIAN_POINT('Ctrl Pts',(32.3753501505309,-3.43895999380719,-6.45388593070681));
#27928=CARTESIAN_POINT('Ctrl Pts',(32.3091796157168,-5.49138661014055,-4.82947177140826));
#27929=CARTESIAN_POINT('Ctrl Pts',(32.2430090809028,-6.38984874475651,-2.72020711315945));
#27930=CARTESIAN_POINT('Ctrl Pts',(32.2163032751373,-6.75245961562451,-1.86892772680491));
#27931=CARTESIAN_POINT('Ctrl Pts',(32.1895974693718,-6.92710655330198,-0.938673286853879));
#27932=CARTESIAN_POINT('Ctrl Pts',(32.1628916636063,-6.92198924261957,-0.00637899664044927));
#27933=CARTESIAN_POINT('Ctrl Pts',(31.9835483363939,-6.9206415740836,-0.000329640349373658));
#27934=CARTESIAN_POINT('Ctrl Pts',(32.0088848983328,-6.92414547100318,-0.885454860675154));
#27935=CARTESIAN_POINT('Ctrl Pts',(32.0342214602717,-6.76608556809867,-1.76996557463074));
#27936=CARTESIAN_POINT('Ctrl Pts',(32.0595580222106,-6.4399614979216,-2.58826217872326));
#27937=CARTESIAN_POINT('Ctrl Pts',(32.0926432896176,-6.01409858504077,-3.65681923196416));
#27938=CARTESIAN_POINT('Ctrl Pts',(32.1257285570246,-5.30165357208037,-4.61246834672295));
#27939=CARTESIAN_POINT('Ctrl Pts',(32.1588138244316,-4.40922992098058,-5.34619371087281));
#27940=CARTESIAN_POINT('Ctrl Pts',(32.1918990918386,-3.51680626988078,-6.07991907502267));
#27941=CARTESIAN_POINT('Ctrl Pts',(32.2249843592456,-2.44440398064157,-6.59172068856359));
#27942=CARTESIAN_POINT('Ctrl Pts',(32.2580696266526,-1.31579639281641,-6.80975252112529));
#27943=CARTESIAN_POINT('Ctrl Pts',(32.2911548940597,-0.187188804991247,
-7.02778435368699));
#27944=CARTESIAN_POINT('Ctrl Pts',(32.3242401614667,0.997624081419872,-6.95204640526946));
#27945=CARTESIAN_POINT('Ctrl Pts',(32.3573254288737,2.09923002332463,-6.60381125494117));
#27946=CARTESIAN_POINT('Ctrl Pts',(32.3904106962807,3.20083596522939,-6.25557610461289));
#27947=CARTESIAN_POINT('Ctrl Pts',(32.4234959636878,4.21923496262778,-5.63484375237386));
#27948=CARTESIAN_POINT('Ctrl Pts',(32.4565812310948,5.01276264886046,-4.80196364224421));
#27949=CARTESIAN_POINT('Ctrl Pts',(32.5227517659088,6.59981802132581,-3.13620342198489));
#27950=CARTESIAN_POINT('Ctrl Pts',(32.5889223007228,7.28738814912826,-0.621852170163068));
#27951=CARTESIAN_POINT('Ctrl Pts',(32.6550928355369,6.75595288246311,1.60835144458171));
#27952=CARTESIAN_POINT('Ctrl Pts',(32.7212633703509,6.22451761579797,3.83855505932649));
#27953=CARTESIAN_POINT('Ctrl Pts',(32.787433905165,4.47407695466521,5.78461103699422));
#27954=CARTESIAN_POINT('Ctrl Pts',(32.853604439979,2.30893373876081,6.549597885576));
#27955=CARTESIAN_POINT('Ctrl Pts',(32.919774974793,0.143790522856417,7.31458473415778));
#27956=CARTESIAN_POINT('Ctrl Pts',(32.9859455096071,-2.43605524781962,6.89850245365361));
#27957=CARTESIAN_POINT('Ctrl Pts',(33.0521160444211,-4.25094412584906,5.49161238079396));
#27958=CARTESIAN_POINT('Ctrl Pts',(33.1125934750787,-5.90968568779572,4.20576669338399));
#27959=CARTESIAN_POINT('Ctrl Pts',(33.1730709057363,-6.92943684460085,2.09227087465205));
#27960=CARTESIAN_POINT('Ctrl Pts',(33.2335483363939,-6.94245604902185,-0.00577606699965401));
#27961=CARTESIAN_POINT('Origin',(29.75,0.,0.));
#27962=CARTESIAN_POINT('',(34.6628916636063,-6.933,1.97064586870965E-14));
#27963=CARTESIAN_POINT('',(34.4835483363939,-6.93389555109049,0.00595474732503822));
#27964=CARTESIAN_POINT('',(29.75,-6.933,-8.4904762584886E-16));
#27965=CARTESIAN_POINT('Ctrl Pts',(34.6628916636063,-6.933,-4.9960036108132E-15));
#27966=CARTESIAN_POINT('Ctrl Pts',(34.6056674683212,-6.933,1.99420935701628));
#27967=CARTESIAN_POINT('Ctrl Pts',(34.5484432730361,-6.02307502629249,3.97063309653046));
#27968=CARTESIAN_POINT('Ctrl Pts',(34.491219077751,-4.50798484753983,5.26731066241125));
#27969=CARTESIAN_POINT('Ctrl Pts',(34.4339948824659,-2.99289466878718,6.56398822829205));
#27970=CARTESIAN_POINT('Ctrl Pts',(34.3767706871808,-0.899664345628758,
7.15779044292411));
#27971=CARTESIAN_POINT('Ctrl Pts',(34.3195464918957,1.07062371681849,6.84983604599305));
#27972=CARTESIAN_POINT('Ctrl Pts',(34.2623222966106,3.04091177926574,6.541881649062));
#27973=CARTESIAN_POINT('Ctrl Pts',(34.2050981013255,4.85311303639886,5.33766370386397));
#27974=CARTESIAN_POINT('Ctrl Pts',(34.1478739060404,5.90026971493765,3.64050907030729));
#27975=CARTESIAN_POINT('Ctrl Pts',(34.0906497107553,6.94742639347644,1.9433544367506));
#27976=CARTESIAN_POINT('Ctrl Pts',(34.0334255154702,7.2108600852751,-0.216464293124));
#27977=CARTESIAN_POINT('Ctrl Pts',(33.9762013201851,6.6023393500608,-2.11556236179385));
#27978=CARTESIAN_POINT('Ctrl Pts',(33.9189771249,5.99381861484649,-4.0146604304637));
#27979=CARTESIAN_POINT('Ctrl Pts',(33.8617529296149,4.52419779647289,-5.61916312790447));
#27980=CARTESIAN_POINT('Ctrl Pts',(33.8045287343298,2.68569473000394,-6.39167683923625));
#27981=CARTESIAN_POINT('Ctrl Pts',(33.7473045390447,0.847191663535,-7.16419055056802));
#27982=CARTESIAN_POINT('Ctrl Pts',(33.6900803437597,-1.32739978994181,-7.09093574623785));
#27983=CARTESIAN_POINT('Ctrl Pts',(33.6328561484746,-3.10974706736201,-6.19644754492712));
#27984=CARTESIAN_POINT('Ctrl Pts',(33.5756319531895,-4.89209434478221,-5.3019593436164));
#27985=CARTESIAN_POINT('Ctrl Pts',(33.5184077579044,-6.25040525058661,-3.6021929658266));
#27986=CARTESIAN_POINT('Ctrl Pts',(33.4611835626193,-6.72974280712766,-1.66644854403415));
#27987=CARTESIAN_POINT('Ctrl Pts',(33.4450862629483,-6.86458158035574,-1.12191912096727));
#27988=CARTESIAN_POINT('Ctrl Pts',(33.4289889632773,-6.933,-0.560975745778045));
#27989=CARTESIAN_POINT('Ctrl Pts',(33.4128916636063,-6.933,-1.9151347174784E-14));
#27990=CARTESIAN_POINT('Ctrl Pts',(33.2335483363939,-6.94245604902185,-0.00577606699965401));
#27991=CARTESIAN_POINT('Ctrl Pts',(33.2392414405504,-6.9436816250094,-0.203277839711076));
#27992=CARTESIAN_POINT('Ctrl Pts',(33.2449345447068,-6.93598595639073,-0.400642710826199));
#27993=CARTESIAN_POINT('Ctrl Pts',(33.2506276488632,-6.91906227514061,-0.597167371676744));
#27994=CARTESIAN_POINT('Ctrl Pts',(33.3167981836772,-6.72235956101991,-2.88135918607271));
#27995=CARTESIAN_POINT('Ctrl Pts',(33.3829687184913,-5.27902214739564,-5.05204494964951));
#27996=CARTESIAN_POINT('Ctrl Pts',(33.4491392533053,-3.24890903512377,-6.13441620840687));
#27997=CARTESIAN_POINT('Ctrl Pts',(33.4822245207123,-2.23385247898783,-6.67560183778555));
#27998=CARTESIAN_POINT('Ctrl Pts',(33.5153097881194,-1.07210199819001,-6.94470884095935));
#27999=CARTESIAN_POINT('Ctrl Pts',(33.5483950555264,0.0832496906585477,
-6.92894560771863));
#28000=CARTESIAN_POINT('Ctrl Pts',(33.5814803229334,1.2386013795071,-6.91318237447791));
#28001=CARTESIAN_POINT('Ctrl Pts',(33.6145655903404,2.38755427640638,-6.61254890482264));
#28002=CARTESIAN_POINT('Ctrl Pts',(33.6476508577474,3.39019622543778,-6.05077719223303));
#28003=CARTESIAN_POINT('Ctrl Pts',(33.6807361251545,4.39283817446916,-5.48900547964343));
#28004=CARTESIAN_POINT('Ctrl Pts',(33.7138213925615,5.24916917563268,-4.6660955241195));
#28005=CARTESIAN_POINT('Ctrl Pts',(33.7469066599685,5.86588595288536,-3.68898482420616));
#28006=CARTESIAN_POINT('Ctrl Pts',(33.7799919273755,6.48260273013804,-2.71187412429283));
#28007=CARTESIAN_POINT('Ctrl Pts',(33.8130771947825,6.85970528347988,-1.58056267999009));
#28008=CARTESIAN_POINT('Ctrl Pts',(33.8461624621895,6.92817161952915,-0.432288782485585));
#28009=CARTESIAN_POINT('Ctrl Pts',(33.9123329970036,7.06510429162769,1.86425901252342));
#28010=CARTESIAN_POINT('Ctrl Pts',(33.9785035318176,5.96749209455592,4.22865662033947));
#28011=CARTESIAN_POINT('Ctrl Pts',(34.0446740666317,4.12212534563731,5.58911513351279));
#28012=CARTESIAN_POINT('Ctrl Pts',(34.1108446014457,2.2767585967187,6.94957364668611));
#28013=CARTESIAN_POINT('Ctrl Pts',(34.1770151362597,-0.316362704046755,
7.30609306521667));
#28014=CARTESIAN_POINT('Ctrl Pts',(34.2431856710738,-2.46387742523262,6.49288633327678));
#28015=CARTESIAN_POINT('Ctrl Pts',(34.3093562058878,-4.61139214641846,5.67967960133689));
#28016=CARTESIAN_POINT('Ctrl Pts',(34.3755267407019,-6.31330028802472,3.69674671892656));
#28017=CARTESIAN_POINT('Ctrl Pts',(34.4416972755159,-6.79143541399258,1.45074781472781));
#28018=CARTESIAN_POINT('Ctrl Pts',(34.4556476291419,-6.89223789514245,0.977236771704476));
#28019=CARTESIAN_POINT('Ctrl Pts',(34.4695979827679,-6.93864750106136,0.492033268463616));
#28020=CARTESIAN_POINT('Ctrl Pts',(34.4835483363939,-6.93389555109049,0.00595474732503822));
#28021=CARTESIAN_POINT('Origin',(29.75,0.,0.));
#28022=CARTESIAN_POINT('',(35.9128916636063,-6.92960145208156,-0.00126819834722902));
#28023=CARTESIAN_POINT('',(35.7335483363939,-6.92339125407611,-0.000268698171690447));
#28024=CARTESIAN_POINT('',(29.75,-6.933,-8.4904762584886E-16));
#28025=CARTESIAN_POINT('Ctrl Pts',(35.9128916636063,-6.92960145208156,-0.00126819834722902));
#28026=CARTESIAN_POINT('Ctrl Pts',(35.8806670960245,-6.9318585040595,1.1242479907601));
#28027=CARTESIAN_POINT('Ctrl Pts',(35.8484425284426,-6.6641919565166,2.25237223453277));
#28028=CARTESIAN_POINT('Ctrl Pts',(35.8162179608608,-6.13825503570355,3.2416449596582));
#28029=CARTESIAN_POINT('Ctrl Pts',(35.7500474260468,-5.05828624356125,5.27303623069012));
#28030=CARTESIAN_POINT('Ctrl Pts',(35.6838768912328,-2.88931292936768,6.71895604486874));
#28031=CARTESIAN_POINT('Ctrl Pts',(35.6177063564187,-0.605354648845225,
6.91835745444872));
#28032=CARTESIAN_POINT('Ctrl Pts',(35.5515358216047,1.67860363167723,7.11775886402871));
#28033=CARTESIAN_POINT('Ctrl Pts',(35.4853652867906,4.07754687852859,6.07064186901007));
#28034=CARTESIAN_POINT('Ctrl Pts',(35.4191947519766,5.48658138221935,4.25742756644304));
#28035=CARTESIAN_POINT('Ctrl Pts',(35.3530242171625,6.89561588591012,2.444213263876));
#28036=CARTESIAN_POINT('Ctrl Pts',(35.2868536823485,7.31474164644029,-0.135098346239444));
#28037=CARTESIAN_POINT('Ctrl Pts',(35.2206831475345,6.55232099334528,-2.30116369306058));
#28038=CARTESIAN_POINT('Ctrl Pts',(35.1545126127204,5.78990034025028,-4.46722903988171));
#28039=CARTESIAN_POINT('Ctrl Pts',(35.0883420779064,3.84593327353012,-6.22004812340854));
#28040=CARTESIAN_POINT('Ctrl Pts',(35.0221715430924,1.6163501133428,-6.75407554214492));
#28041=CARTESIAN_POINT('Ctrl Pts',(34.9560010082783,-0.613233046844523,
-7.2881029608813));
#28042=CARTESIAN_POINT('Ctrl Pts',(34.8898304734643,-3.128432300499,-6.60333871482723));
#28043=CARTESIAN_POINT('Ctrl Pts',(34.8236599386502,-4.79603498530099,-5.01841462544935));
#28044=CARTESIAN_POINT('Ctrl Pts',(34.7905746712432,-5.62983632770198,-4.22595258076041));
#28045=CARTESIAN_POINT('Ctrl Pts',(34.7574894038362,-6.25173852788985,-3.20845057524052));
#28046=CARTESIAN_POINT('Ctrl Pts',(34.7244041364292,-6.60130234039749,-2.10713804160215));
#28047=CARTESIAN_POINT('Ctrl Pts',(34.7038999788215,-6.81793989745299,-1.42461414094293));
#28048=CARTESIAN_POINT('Ctrl Pts',(34.6833958212139,-6.92997944340521,-0.709900820990376));
#28049=CARTESIAN_POINT('Ctrl Pts',(34.6628916636063,-6.93227389215358,0.00361668279959731));
#28050=CARTESIAN_POINT('Ctrl Pts',(34.4835483363939,-6.93389555109049,0.00595474732503822));
#28051=CARTESIAN_POINT('Ctrl Pts',(34.535768517582,-6.91610763724059,-1.81357679473825));
#28052=CARTESIAN_POINT('Ctrl Pts',(34.58798869877,-6.18143378983398,-3.64536926224785));
#28053=CARTESIAN_POINT('Ctrl Pts',(34.640208879958,-4.89936216432684,-4.92202954051599));
#28054=CARTESIAN_POINT('Ctrl Pts',(34.706379414772,-3.27479167836381,-6.53974306557382));
#28055=CARTESIAN_POINT('Ctrl Pts',(34.7725499495861,-0.771288596108303,
-7.26610518970229));
#28056=CARTESIAN_POINT('Ctrl Pts',(34.8387204844001,1.47793304890319,-6.78248854273389));
#28057=CARTESIAN_POINT('Ctrl Pts',(34.8718057518071,2.60254387140893,-6.54068021924969));
#28058=CARTESIAN_POINT('Ctrl Pts',(34.9048910192141,3.66358433460367,-5.99637720299127));
#28059=CARTESIAN_POINT('Ctrl Pts',(34.9379762866212,4.53587037073918,-5.2386165409355));
#28060=CARTESIAN_POINT('Ctrl Pts',(34.9710615540282,5.40815640687468,-4.48085587887973));
#28061=CARTESIAN_POINT('Ctrl Pts',(35.0041468214352,6.09168801595097,-3.50963757102659));
#28062=CARTESIAN_POINT('Ctrl Pts',(35.0372320888422,6.49491391291778,-2.43339928941026));
#28063=CARTESIAN_POINT('Ctrl Pts',(35.0703173562492,6.8981398098846,-1.35716100779393));
#28064=CARTESIAN_POINT('Ctrl Pts',(35.1034026236563,7.02105999474195,-0.175902752414387));
#28065=CARTESIAN_POINT('Ctrl Pts',(35.1364878910633,6.8614340140831,0.968476425158562));
#28066=CARTESIAN_POINT('Ctrl Pts',(35.1695731584703,6.70180803342424,2.11285560273151));
#28067=CARTESIAN_POINT('Ctrl Pts',(35.2026584258773,6.2596358872492,3.22035570249786));
#28068=CARTESIAN_POINT('Ctrl Pts',(35.2357436932843,5.57077791340997,4.14160239190325));
#28069=CARTESIAN_POINT('Ctrl Pts',(35.3019142280984,4.19306196573149,5.98409577071403));
#28070=CARTESIAN_POINT('Ctrl Pts',(35.3680847629124,1.82860270739628,7.08157550808095));
#28071=CARTESIAN_POINT('Ctrl Pts',(35.4342552977264,-0.459001209328522,
6.92960619427528));
#28072=CARTESIAN_POINT('Ctrl Pts',(35.5004258325405,-2.74660512605329,6.77763688046961));
#28073=CARTESIAN_POINT('Ctrl Pts',(35.5665963673545,-4.95735370116766,5.37621851549137));
#28074=CARTESIAN_POINT('Ctrl Pts',(35.6327669021686,-6.07274754602132,3.36897640009331));
#28075=CARTESIAN_POINT('Ctrl Pts',(35.666360713577,-6.63901666528224,2.34992897565731));
#28076=CARTESIAN_POINT('Ctrl Pts',(35.6999545249855,-6.92296421607281,1.17473386069699));
#28077=CARTESIAN_POINT('Ctrl Pts',(35.7335483363939,-6.92339125407611,-0.000268698171690447));
#28078=CARTESIAN_POINT('Origin',(29.75,0.,0.));
#28079=CARTESIAN_POINT('',(37.1628916636063,-6.93290463700014,-0.000100259380880677));
#28080=CARTESIAN_POINT('',(36.9835483363939,-6.93502389967407,-0.00589331438187145));
#28081=CARTESIAN_POINT('',(29.75,-6.933,-8.4904762584886E-16));
#28082=CARTESIAN_POINT('Ctrl Pts',(37.1628916636063,-6.92971491769494,-0.00345375376834933));
#28083=CARTESIAN_POINT('Ctrl Pts',(37.111023638242,-6.91260075130355,1.80429354156629));
#28084=CARTESIAN_POINT('Ctrl Pts',(37.0591556128777,-6.19436612714247,3.61861004078152));
#28085=CARTESIAN_POINT('Ctrl Pts',(37.0072875875135,-4.92782277232531,4.89353520916524));
#28086=CARTESIAN_POINT('Ctrl Pts',(36.9411170526994,-3.31203249373178,6.52001857049164));
#28087=CARTESIAN_POINT('Ctrl Pts',(36.8749465178854,-0.803851543980656,
7.26862462506543));
#28088=CARTESIAN_POINT('Ctrl Pts',(36.8087759830714,1.44271150104494,6.79314715502428));
#28089=CARTESIAN_POINT('Ctrl Pts',(36.7426054482574,3.68927454607051,6.31766968498313));
#28090=CARTESIAN_POINT('Ctrl Pts',(36.6764349134433,5.67421968637056,4.61810869032707));
#28091=CARTESIAN_POINT('Ctrl Pts',(36.6102643786292,6.48996666690957,2.47155768847992));
#28092=CARTESIAN_POINT('Ctrl Pts',(36.5440938438152,7.30571364744857,0.325006686632785));
#28093=CARTESIAN_POINT('Ctrl Pts',(36.4779233090012,6.95226246822655,-2.26853432240543));
#28094=CARTESIAN_POINT('Ctrl Pts',(36.4117527741872,5.59398829109631,-4.115509581796));
#28095=CARTESIAN_POINT('Ctrl Pts',(36.3455822393731,4.23571411396608,-5.96248484118655));
#28096=CARTESIAN_POINT('Ctrl Pts',(36.2794117045591,1.87261693892766,-7.06289435092948));
#28097=CARTESIAN_POINT('Ctrl Pts',(36.213241169745,-0.424091389993473,-6.92867833148972));
#28098=CARTESIAN_POINT('Ctrl Pts',(36.180155902338,-1.57244555445406,-6.86157032176984));
#28099=CARTESIAN_POINT('Ctrl Pts',(36.147070634931,-2.70420250738532,-6.48580592975427));
#28100=CARTESIAN_POINT('Ctrl Pts',(36.113985367524,-3.68204209515384,-5.87024610598754));
#28101=CARTESIAN_POINT('Ctrl Pts',(36.0809001001169,-4.65988168292234,-5.25468628222081));
#28102=CARTESIAN_POINT('Ctrl Pts',(36.0478148327099,-5.4838039055281,-4.39933102670292));
#28103=CARTESIAN_POINT('Ctrl Pts',(36.0147295653029,-6.04676165595723,-3.39735371629919));
#28104=CARTESIAN_POINT('Ctrl Pts',(35.9816442978959,-6.60971940638636,-2.39537640589547));
#28105=CARTESIAN_POINT('Ctrl Pts',(35.9485590304889,-6.91171268463887,-1.24677704060591));
#28106=CARTESIAN_POINT('Ctrl Pts',(35.9154737630819,-6.92884269098595,-0.0914456080964819));
#28107=CARTESIAN_POINT('Ctrl Pts',(35.9146130632567,-6.92928832115987,-0.0613901290286256));
#28108=CARTESIAN_POINT('Ctrl Pts',(35.9137523634315,-6.92954116751024,-0.0313300939727322));
#28109=CARTESIAN_POINT('Ctrl Pts',(35.9128916636063,-6.92960145208156,-0.00126819834722902));
#28110=CARTESIAN_POINT('Ctrl Pts',(35.7335483363939,-6.92339125407611,-0.000268698171690447));
#28111=CARTESIAN_POINT('Ctrl Pts',(35.7661250597995,-6.92380536305433,-1.1396968177055));
#28112=CARTESIAN_POINT('Ctrl Pts',(35.7987017832051,-6.65760683712713,-2.27894386431991));
#28113=CARTESIAN_POINT('Ctrl Pts',(35.8312785066107,-6.12370236615607,-3.27544410392846));
#28114=CARTESIAN_POINT('Ctrl Pts',(35.8974490414247,-5.03922422684416,-5.29955662673429));
#28115=CARTESIAN_POINT('Ctrl Pts',(35.9636195762388,-2.85022883362737,-6.73471580652803));
#28116=CARTESIAN_POINT('Ctrl Pts',(36.0297901110528,-0.565224684335127,
-6.92175159729262));
#28117=CARTESIAN_POINT('Ctrl Pts',(36.0959606458668,1.7197794649571,-7.10878738805721));
#28118=CARTESIAN_POINT('Ctrl Pts',(36.1621311806808,4.10079237032479,-6.04769978979263));
#28119=CARTESIAN_POINT('Ctrl Pts',(36.2283017154949,5.50660409421191,-4.22655276524806));
#28120=CARTESIAN_POINT('Ctrl Pts',(36.2613869829019,6.20950995615547,-3.31597925297579));
#28121=CARTESIAN_POINT('Ctrl Pts',(36.2944722503089,6.66861552272889,-2.21539088413354));
#28122=CARTESIAN_POINT('Ctrl Pts',(36.3275575177159,6.84577375546842,-1.07359444140203));
#28123=CARTESIAN_POINT('Ctrl Pts',(36.360642785123,7.02293198820795,0.068202001329485));
#28124=CARTESIAN_POINT('Ctrl Pts',(36.39372805253,6.91814288711357,1.25120651795023));
#28125=CARTESIAN_POINT('Ctrl Pts',(36.426813319937,6.5314703880391,2.33350238220899));
#28126=CARTESIAN_POINT('Ctrl Pts',(36.459898587344,6.14479788896462,3.41579824646776));
#28127=CARTESIAN_POINT('Ctrl Pts',(36.492983854751,5.47624199191003,4.39738545836455));
#28128=CARTESIAN_POINT('Ctrl Pts',(36.5260691221581,4.61568011269898,5.16843500806403));
#28129=CARTESIAN_POINT('Ctrl Pts',(36.5591543895651,3.75511823348794,5.93948455776351));
#28130=CARTESIAN_POINT('Ctrl Pts',(36.5922396569721,2.70255037212044,6.49999644526569));
#28131=CARTESIAN_POINT('Ctrl Pts',(36.6253249243791,1.58178036580302,6.759024175329));
#28132=CARTESIAN_POINT('Ctrl Pts',(36.6914954591931,-0.659759646831825,
7.27707963545561));
#28133=CARTESIAN_POINT('Ctrl Pts',(36.7576659940072,-3.17410823926632,6.58919846582668));
#28134=CARTESIAN_POINT('Ctrl Pts',(36.8238365288212,-4.82329809281977,4.99659080039366));
#28135=CARTESIAN_POINT('Ctrl Pts',(36.8770737980121,-6.15014794263986,3.71526394942559));
#28136=CARTESIAN_POINT('Ctrl Pts',(36.930311067203,-6.91698486849107,1.84831216335871));
#28137=CARTESIAN_POINT('Ctrl Pts',(36.9835483363939,-6.93502389967407,-0.00589331438187144));
#28138=CARTESIAN_POINT('Origin',(29.75,0.,0.));
#28139=CARTESIAN_POINT('',(38.4128916636063,-6.93577359535222,0.000670304473996572));
#28140=CARTESIAN_POINT('',(38.2335483363939,-6.94167024712608,0.00637861567201024));
#28141=CARTESIAN_POINT('',(29.75,-6.933,-8.4904762584886E-16));
#28142=CARTESIAN_POINT('Ctrl Pts',(38.4128916636063,-6.933,2.77555756156289E-16));
#28143=CARTESIAN_POINT('Ctrl Pts',(38.3556674683212,-6.933,1.99420935701628));
#28144=CARTESIAN_POINT('Ctrl Pts',(38.2984432730361,-6.02307502629249,3.97063309653045));
#28145=CARTESIAN_POINT('Ctrl Pts',(38.241219077751,-4.50798484753985,5.26731066241124));
#28146=CARTESIAN_POINT('Ctrl Pts',(38.1839948824659,-2.9928946687872,6.56398822829204));
#28147=CARTESIAN_POINT('Ctrl Pts',(38.1267706871808,-0.899664345628795,
7.1577904429241));
#28148=CARTESIAN_POINT('Ctrl Pts',(38.0695464918957,1.07062371681845,6.84983604599306));
#28149=CARTESIAN_POINT('Ctrl Pts',(38.0123222966106,3.04091177926569,6.54188164906202));
#28150=CARTESIAN_POINT('Ctrl Pts',(37.9550981013255,4.85311303639881,5.33766370386401));
#28151=CARTESIAN_POINT('Ctrl Pts',(37.8978739060404,5.90026971493761,3.64050907030734));
#28152=CARTESIAN_POINT('Ctrl Pts',(37.8406497107553,6.94742639347642,1.94335443675068));
#28153=CARTESIAN_POINT('Ctrl Pts',(37.7834255154702,7.2108600852751,-0.216464293123911));
#28154=CARTESIAN_POINT('Ctrl Pts',(37.7262013201851,6.60233935006083,-2.11556236179376));
#28155=CARTESIAN_POINT('Ctrl Pts',(37.6689771249,5.99381861484655,-4.01466043046361));
#28156=CARTESIAN_POINT('Ctrl Pts',(37.611752929615,4.52419779647298,-5.6191631279044));
#28157=CARTESIAN_POINT('Ctrl Pts',(37.5545287343298,2.68569473000405,-6.3916768392362));
#28158=CARTESIAN_POINT('Ctrl Pts',(37.4973045390448,0.847191663535129,-7.164190550568));
#28159=CARTESIAN_POINT('Ctrl Pts',(37.4400803437597,-1.32739978994167,-7.09093574623788));
#28160=CARTESIAN_POINT('Ctrl Pts',(37.3828561484746,-3.10974706736188,-6.19644754492719));
#28161=CARTESIAN_POINT('Ctrl Pts',(37.3256319531895,-4.89209434478209,-5.3019593436165));
#28162=CARTESIAN_POINT('Ctrl Pts',(37.2684077579044,-6.25040525058653,-3.60219296582674));
#28163=CARTESIAN_POINT('Ctrl Pts',(37.2111835626193,-6.72974280712762,-1.66644854403432));
#28164=CARTESIAN_POINT('Ctrl Pts',(37.1950862629483,-6.86458158035574,-1.12191912096732));
#28165=CARTESIAN_POINT('Ctrl Pts',(37.1789889632773,-6.93300000000001,-0.56097574577799));
#28166=CARTESIAN_POINT('Ctrl Pts',(37.1628916636063,-6.933,1.46271883494364E-13));
#28167=CARTESIAN_POINT('Ctrl Pts',(36.9835483363939,-6.93502389967407,-0.00589331438187144));
#28168=CARTESIAN_POINT('Ctrl Pts',(36.996481602017,-6.93940623530886,-0.45634714734448));
#28169=CARTESIAN_POINT('Ctrl Pts',(37.0094148676402,-6.89959597956175,-0.906048718048468));
#28170=CARTESIAN_POINT('Ctrl Pts',(37.0223481332633,-6.81288640392014,-1.34641880273624));
#28171=CARTESIAN_POINT('Ctrl Pts',(37.0885186680774,-6.36925374679465,-3.59948657919598));
#28172=CARTESIAN_POINT('Ctrl Pts',(37.1546892028914,-4.69795731787126,-5.60828797087832));
#28173=CARTESIAN_POINT('Ctrl Pts',(37.2208597377055,-2.56316717324256,-6.45433488339996));
#28174=CARTESIAN_POINT('Ctrl Pts',(37.2870302725195,-0.428377028613836,
-7.3003817959216));
#28175=CARTESIAN_POINT('Ctrl Pts',(37.3532008073335,2.1699068317202,-6.98367422928253));
#28176=CARTESIAN_POINT('Ctrl Pts',(37.4193713421476,4.03592169067489,-5.65167764699365));
#28177=CARTESIAN_POINT('Ctrl Pts',(37.4855418769616,5.90193654962956,-4.31968106470479));
#28178=CARTESIAN_POINT('Ctrl Pts',(37.5517124117756,7.03568240720489,-1.97239546676614));
#28179=CARTESIAN_POINT('Ctrl Pts',(37.6178829465897,6.93398675840259,0.325982457550818));
#28180=CARTESIAN_POINT('Ctrl Pts',(37.6509682139967,6.88313893400144,1.47517141970932));
#28181=CARTESIAN_POINT('Ctrl Pts',(37.6840534814037,6.52343073300587,2.61213346346238));
#28182=CARTESIAN_POINT('Ctrl Pts',(37.7171387488107,5.92177261965832,3.59858755296438));
#28183=CARTESIAN_POINT('Ctrl Pts',(37.7502240162178,5.32011450631077,4.58504164246637));
#28184=CARTESIAN_POINT('Ctrl Pts',(37.7833092836248,4.47650648061124,5.42098777771728));
#28185=CARTESIAN_POINT('Ctrl Pts',(37.8163945510318,3.48259747344794,5.99807082616737));
#28186=CARTESIAN_POINT('Ctrl Pts',(37.8494798184388,2.48868846628466,6.57515387461745));
#28187=CARTESIAN_POINT('Ctrl Pts',(37.8825650858458,1.34447847765756,6.89337383626672));
#28188=CARTESIAN_POINT('Ctrl Pts',(37.9156503532529,0.18950522617225,6.92685434411176));
#28189=CARTESIAN_POINT('Ctrl Pts',(37.9487356206599,-0.965468025313094,
6.96033485195681));
#28190=CARTESIAN_POINT('Ctrl Pts',(37.9818208880669,-2.13120453965668,6.70907590599762));
#28191=CARTESIAN_POINT('Ctrl Pts',(38.0149061554739,-3.15444121278794,6.18352145329789));
#28192=CARTESIAN_POINT('Ctrl Pts',(38.0810766902879,-5.2009145590504,5.13241254789846));
#28193=CARTESIAN_POINT('Ctrl Pts',(38.147247225102,-6.6773885404635,2.98412161553692));
#28194=CARTESIAN_POINT('Ctrl Pts',(38.213417759916,-6.90909644225956,0.703214384342509));
#28195=CARTESIAN_POINT('Ctrl Pts',(38.2201279520753,-6.93259337409259,0.471913158474033));
#28196=CARTESIAN_POINT('Ctrl Pts',(38.2268381442346,-6.94328976360018,0.239248173925071));
#28197=CARTESIAN_POINT('Ctrl Pts',(38.2335483363939,-6.94167024712608,0.00637861567201024));
#28198=CARTESIAN_POINT('Origin',(29.75,0.,0.));
#28199=CARTESIAN_POINT('',(39.6628916636063,-6.92332261655204,0.00297343908938319));
#28200=CARTESIAN_POINT('',(39.4835483363939,-6.92769178317914,-6.1482564198808E-5));
#28201=CARTESIAN_POINT('',(29.75,-6.933,-8.4904762584886E-16));
#28202=CARTESIAN_POINT('Ctrl Pts',(39.6628916636063,-6.92332261655204,0.00297343908938319));
#28203=CARTESIAN_POINT('Ctrl Pts',(39.6379072574912,-6.92850463656999,0.8768019092153));
#28204=CARTESIAN_POINT('Ctrl Pts',(39.612922851376,-6.77585609379785,1.74910600870471));
#28205=CARTESIAN_POINT('Ctrl Pts',(39.5879384452609,-6.45736297806441,2.55552893049358));
#28206=CARTESIAN_POINT('Ctrl Pts',(39.5217679104469,-5.61384243546796,4.69131858165475));
#28207=CARTESIAN_POINT('Ctrl Pts',(39.4555973756329,-3.60701984478563,6.36499055491544));
#28208=CARTESIAN_POINT('Ctrl Pts',(39.3894268408188,-1.35447852944345,6.81128861951564));
#28209=CARTESIAN_POINT('Ctrl Pts',(39.3232563060048,0.898062785898749,7.25758668411585));
#28210=CARTESIAN_POINT('Ctrl Pts',(39.2570857711907,3.39632282590077,6.47651084005551));
#28211=CARTESIAN_POINT('Ctrl Pts',(39.1909152363767,4.9908806162241,4.82920643515976));
#28212=CARTESIAN_POINT('Ctrl Pts',(39.1247447015627,6.58543840654742,3.18190203026401));
#28213=CARTESIAN_POINT('Ctrl Pts',(39.0585741667487,7.27629394719206,0.668369064532852));
#28214=CARTESIAN_POINT('Ctrl Pts',(38.9924036319346,6.76089092856649,-1.57378231670003));
#28215=CARTESIAN_POINT('Ctrl Pts',(38.9593183645276,6.5031894192537,-2.69485800731648));
#28216=CARTESIAN_POINT('Ctrl Pts',(38.9262330971205,5.94392327012335,-3.74808830180835));
#28217=CARTESIAN_POINT('Ctrl Pts',(38.8931478297135,5.17389243420951,-4.60956184626221));
#28218=CARTESIAN_POINT('Ctrl Pts',(38.8600625623065,4.40386159829564,-5.47103539071609));
#28219=CARTESIAN_POINT('Ctrl Pts',(38.8269772948995,3.42306607559827,-6.14075218513195));
#28220=CARTESIAN_POINT('Ctrl Pts',(38.7938920274925,2.34122846057253,-6.52870493231168));
#28221=CARTESIAN_POINT('Ctrl Pts',(38.7608067600855,1.25939084554681,-6.9166576794914));
#28222=CARTESIAN_POINT('Ctrl Pts',(38.7277214926785,0.0765111381927339,
-7.02284637943501));
#28223=CARTESIAN_POINT('Ctrl Pts',(38.6946362252715,-1.06549411019643,-6.84703918759221));
#28224=CARTESIAN_POINT('Ctrl Pts',(38.6615509578644,-2.20749935858561,-6.67123199574941));
#28225=CARTESIAN_POINT('Ctrl Pts',(38.6284656904574,-3.30863014800987,-6.21342891212019));
#28226=CARTESIAN_POINT('Ctrl Pts',(38.5953804230504,-4.22003466628295,-5.51160088755531));
#28227=CARTESIAN_POINT('Ctrl Pts',(38.534550836569,-5.89571584732849,-4.22124080099123));
#28228=CARTESIAN_POINT('Ctrl Pts',(38.4737212500876,-6.93005765768905,-2.10599335907293));
#28229=CARTESIAN_POINT('Ctrl Pts',(38.4128916636063,-6.94291148540326,0.00239534328771114));
#28230=CARTESIAN_POINT('Ctrl Pts',(38.2335483363939,-6.94167024712608,0.00637861567201024));
#28231=CARTESIAN_POINT('Ctrl Pts',(38.2930086790487,-6.92731939066792,-2.05712469375046));
#28232=CARTESIAN_POINT('Ctrl Pts',(38.3524690217034,-5.94591333167301,-4.1366913009233));
#28233=CARTESIAN_POINT('Ctrl Pts',(38.4119293643581,-4.33465654613917,-5.42577343538037));
#28234=CARTESIAN_POINT('Ctrl Pts',(38.4780998991722,-2.54156692604374,-6.86033049388152));
#28235=CARTESIAN_POINT('Ctrl Pts',(38.5442704339862,0.031554136326008,-7.31592108085652));
#28236=CARTESIAN_POINT('Ctrl Pts',(38.6104409688002,2.20819358647839,-6.58423464266746));
#28237=CARTESIAN_POINT('Ctrl Pts',(38.6766115036143,4.38483303663073,-5.8525482044784));
#28238=CARTESIAN_POINT('Ctrl Pts',(38.7427820384283,6.16499087456564,-3.93358474112524));
#28239=CARTESIAN_POINT('Ctrl Pts',(38.8089525732423,6.73052165696255,-1.71178338114024));
#28240=CARTESIAN_POINT('Ctrl Pts',(38.8751231080564,7.29605243935946,0.510017978844769));
#28241=CARTESIAN_POINT('Ctrl Pts',(38.9412936428704,6.64695616621838,3.03465723546165));
#28242=CARTESIAN_POINT('Ctrl Pts',(39.0074641776845,5.08579358974434,4.72452542493378));
#28243=CARTESIAN_POINT('Ctrl Pts',(39.0405494450915,4.3052123015073,5.56945951966986));
#28244=CARTESIAN_POINT('Ctrl Pts',(39.0736347124985,3.29661443743698,6.20570084761976));
#28245=CARTESIAN_POINT('Ctrl Pts',(39.1067199799055,2.20035984233609,6.57081729311669));
#28246=CARTESIAN_POINT('Ctrl Pts',(39.1398052473125,1.10410524723521,6.93593373861362));
#28247=CARTESIAN_POINT('Ctrl Pts',(39.1728905147195,-0.0798060788962004,
7.0299253016576));
#28248=CARTESIAN_POINT('Ctrl Pts',(39.2059757821266,-1.21143464275791,6.82918479059629));
#28249=CARTESIAN_POINT('Ctrl Pts',(39.2390610495336,-2.34306320661961,6.62844427953498));
#28250=CARTESIAN_POINT('Ctrl Pts',(39.2721463169406,-3.42240900821157,6.13297169436833));
#28251=CARTESIAN_POINT('Ctrl Pts',(39.3052315843476,-4.32619084933698,5.41306715923603));
#28252=CARTESIAN_POINT('Ctrl Pts',(39.3383168517546,-5.22997269046238,4.69316262410372));
#28253=CARTESIAN_POINT('Ctrl Pts',(39.3714021191617,-5.95819057112127,3.74882613900572));
#28254=CARTESIAN_POINT('Ctrl Pts',(39.4044873865687,-6.40052273738413,2.68695843223506));
#28255=CARTESIAN_POINT('Ctrl Pts',(39.4308410365104,-6.7528568117702,1.84114118420078));
#28256=CARTESIAN_POINT('Ctrl Pts',(39.4571946864522,-6.92380449431593,0.920753703537604));
#28257=CARTESIAN_POINT('Ctrl Pts',(39.4835483363939,-6.92013724019376,-0.000148983254069613));
#28258=CARTESIAN_POINT('Origin',(29.75,0.,0.));
#28259=CARTESIAN_POINT('',(40.9128916636063,-6.92852880502623,-0.00501897357509773));
#28260=CARTESIAN_POINT('',(40.7335483363939,-6.93300654955486,-1.27468492755348E-5));
#28261=CARTESIAN_POINT('',(29.75,-6.933,-8.4904762584886E-16));
#28262=CARTESIAN_POINT('Ctrl Pts',(40.9128916636063,-6.92852880502623,-0.00501897357509773));
#28263=CARTESIAN_POINT('Ctrl Pts',(40.8682637997087,-6.91735475736882,1.55301169949673));
#28264=CARTESIAN_POINT('Ctrl Pts',(40.8236359358112,-6.3969852050255,3.11776396156197));
#28265=CARTESIAN_POINT('Ctrl Pts',(40.7790080719136,-5.43089818827215,4.32823400634588));
#28266=CARTESIAN_POINT('Ctrl Pts',(40.7128375370996,-3.9984636285045,6.12301966813749));
#28267=CARTESIAN_POINT('Ctrl Pts',(40.6466670022855,-1.58614038791887,7.1389326981632));
#28268=CARTESIAN_POINT('Ctrl Pts',(40.5804964674715,0.6950393921076,6.90992361478826));
#28269=CARTESIAN_POINT('Ctrl Pts',(40.5143259326574,2.97621917213404,6.68091453141333));
#28270=CARTESIAN_POINT('Ctrl Pts',(40.4481553978434,5.1262554916013,5.20698333463781));
#28271=CARTESIAN_POINT('Ctrl Pts',(40.3819848630294,6.1797849470107,3.16175504064282));
#28272=CARTESIAN_POINT('Ctrl Pts',(40.3488995956224,6.7065496747154,2.13914089364533));
#28273=CARTESIAN_POINT('Ctrl Pts',(40.3158143282154,6.95918768640563,0.973702472342916));
#28274=CARTESIAN_POINT('Ctrl Pts',(40.2827290608083,6.92707370902873,-0.181309583225821));
#28275=CARTESIAN_POINT('Ctrl Pts',(40.2496437934013,6.89495973165184,-1.33632163879456));
#28276=CARTESIAN_POINT('Ctrl Pts',(40.2165585259943,6.57809376520782,-2.48090732862967));
#28277=CARTESIAN_POINT('Ctrl Pts',(40.1834732585873,6.00218706448473,-3.47549841615815));
#28278=CARTESIAN_POINT('Ctrl Pts',(40.1503879911802,5.42628036376162,-4.47008950368665));
#28279=CARTESIAN_POINT('Ctrl Pts',(40.1173027237732,4.59133292875946,-5.31468598890848));
#28280=CARTESIAN_POINT('Ctrl Pts',(40.0842174563662,3.6055913817208,-5.91751080466672));
#28281=CARTESIAN_POINT('Ctrl Pts',(40.0511321889592,2.61984983468214,-6.52033562042496));
#28282=CARTESIAN_POINT('Ctrl Pts',(40.0180469215522,1.48331417560702,-6.88138876671957));
#28283=CARTESIAN_POINT('Ctrl Pts',(39.9849616541452,0.334186178414354,-6.93359621888145));
#28284=CARTESIAN_POINT('Ctrl Pts',(39.9187911193311,-1.96406981597094,-7.03801112320521));
#28285=CARTESIAN_POINT('Ctrl Pts',(39.8526205845171,-4.3126951628264,-5.90704325099806));
#28286=CARTESIAN_POINT('Ctrl Pts',(39.786450049703,-5.64689858899888,-4.04260565036367));
#28287=CARTESIAN_POINT('Ctrl Pts',(39.7452639210041,-6.47733881704471,-2.88213494861335));
#28288=CARTESIAN_POINT('Ctrl Pts',(39.7040777923052,-6.91478019443497,-1.43750954319842));
#28289=CARTESIAN_POINT('Ctrl Pts',(39.6628916636063,-6.92332261655204,0.00297343908938319));
#28290=CARTESIAN_POINT('Ctrl Pts',(39.4835483363939,-6.933,-5.33212363151847E-12));
#28291=CARTESIAN_POINT('Ctrl Pts',(39.540772531679,-6.93299999999847,-1.99420935702161));
#28292=CARTESIAN_POINT('Ctrl Pts',(39.5979967269641,-6.02307502628944,-3.97063309653508));
#28293=CARTESIAN_POINT('Ctrl Pts',(39.6552209222492,-4.50798484753579,-5.26731066241471));
#28294=CARTESIAN_POINT('Ctrl Pts',(39.7124451175343,-2.99289466878215,-6.56398822829434));
#28295=CARTESIAN_POINT('Ctrl Pts',(39.7696693128194,-0.899664345623291,
-7.15779044292479));
#28296=CARTESIAN_POINT('Ctrl Pts',(39.8268935081045,1.07062371682372,-6.84983604599224));
#28297=CARTESIAN_POINT('Ctrl Pts',(39.8841177033896,3.04091177927072,-6.54188164905968));
#28298=CARTESIAN_POINT('Ctrl Pts',(39.9413418986747,4.85311303640291,-5.33766370386027));
#28299=CARTESIAN_POINT('Ctrl Pts',(39.9985660939598,5.90026971494041,-3.64050907030281));
#28300=CARTESIAN_POINT('Ctrl Pts',(40.0557902892449,6.94742639347791,-1.94335443674534));
#28301=CARTESIAN_POINT('Ctrl Pts',(40.11301448453,7.21086008527493,0.216464293129457));
#28302=CARTESIAN_POINT('Ctrl Pts',(40.1702386798151,6.6023393500592,2.11556236179884));
#28303=CARTESIAN_POINT('Ctrl Pts',(40.2274628751002,5.99381861484346,4.01466043046822));
#28304=CARTESIAN_POINT('Ctrl Pts',(40.2846870703853,4.52419779646866,5.61916312790788));
#28305=CARTESIAN_POINT('Ctrl Pts',(40.3419112656703,2.68569472999914,6.39167683923827));
#28306=CARTESIAN_POINT('Ctrl Pts',(40.3991354609554,0.84719166352962,7.16419055056865));
#28307=CARTESIAN_POINT('Ctrl Pts',(40.4563596562405,-1.32739978994712,7.09093574623685));
#28308=CARTESIAN_POINT('Ctrl Pts',(40.5135838515256,-3.10974706736665,6.1964475449248));
#28309=CARTESIAN_POINT('Ctrl Pts',(40.5708080468107,-4.89209434478617,5.30195934361274));
#28310=CARTESIAN_POINT('Ctrl Pts',(40.6280322420958,-6.2504052505893,3.60219296582193));
#28311=CARTESIAN_POINT('Ctrl Pts',(40.6852564373809,-6.7297428071289,1.66644854402914));
#28312=CARTESIAN_POINT('Ctrl Pts',(40.7013537370519,-6.86458158035659,1.12191912096209));
#28313=CARTESIAN_POINT('Ctrl Pts',(40.7174510367229,-6.93300000000043,0.560975745772757));
#28314=CARTESIAN_POINT('Ctrl Pts',(40.7335483363939,-6.933,-5.33018074122538E-12));
#28315=CARTESIAN_POINT('Origin',(29.75,0.,0.));
#28316=CARTESIAN_POINT('',(42.1628916636063,-6.94425388693856,-0.00173762222092533));
#28317=CARTESIAN_POINT('',(41.983548336394,-6.93579090859155,-0.000199833497099776));
#28318=CARTESIAN_POINT('',(29.75,-6.933,-8.4904762584886E-16));
#28319=CARTESIAN_POINT('Ctrl Pts',(42.1628916636063,-6.94425388693856,-0.00173762222092533));
#28320=CARTESIAN_POINT('Ctrl Pts',(42.0986203419263,-6.93743152686536,2.22904201996126));
#28321=CARTESIAN_POINT('Ctrl Pts',(42.0343490202463,-5.76506820550086,4.46620311375873));
#28322=CARTESIAN_POINT('Ctrl Pts',(41.9700776985663,-3.92913448030361,5.72643225354837));
#28323=CARTESIAN_POINT('Ctrl Pts',(41.9039071637522,-2.03894903983166,7.0239010777201));
#28324=CARTESIAN_POINT('Ctrl Pts',(41.8377366289382,0.55460315267518,7.28584834836761));
#28325=CARTESIAN_POINT('Ctrl Pts',(41.7715660941241,2.67938377070186,6.40369733338716));
#28326=CARTESIAN_POINT('Ctrl Pts',(41.7384808267171,3.7417740797152,5.96262182589693));
#28327=CARTESIAN_POINT('Ctrl Pts',(41.7053955593101,4.68697149510849,5.23552174699971));
#28328=CARTESIAN_POINT('Ctrl Pts',(41.6723102919031,5.4079448361866,4.33259229377163));
#28329=CARTESIAN_POINT('Ctrl Pts',(41.6392250244961,6.1289181772647,3.42966284054355));
#28330=CARTESIAN_POINT('Ctrl Pts',(41.606139757089,6.62566744402761,2.35090401298461));
#28331=CARTESIAN_POINT('Ctrl Pts',(41.573054489682,6.82774670134459,1.2195137473861));
#28332=CARTESIAN_POINT('Ctrl Pts',(41.539969222275,7.02982595866158,0.0881234817875855));
#28333=CARTESIAN_POINT('Ctrl Pts',(41.506883954868,6.93723520653264,-1.09589822185049));
#28334=CARTESIAN_POINT('Ctrl Pts',(41.473798687461,6.57341605062311,-2.19258403731697));
#28335=CARTESIAN_POINT('Ctrl Pts',(41.440713420054,6.20959689471358,-3.28926985278344));
#28336=CARTESIAN_POINT('Ctrl Pts',(41.407628152647,5.57454933502346,-4.29861978007831));
#28337=CARTESIAN_POINT('Ctrl Pts',(41.3745428852399,4.73053937671899,-5.08020020605896));
#28338=CARTESIAN_POINT('Ctrl Pts',(41.3083723504259,3.04251946011003,-6.64336105802027));
#28339=CARTESIAN_POINT('Ctrl Pts',(41.2422018156119,0.518649949043639,-7.29544390472471));
#28340=CARTESIAN_POINT('Ctrl Pts',(41.1760312807978,-1.70381896380896,-6.73254224326552));
#28341=CARTESIAN_POINT('Ctrl Pts',(41.1098607459838,-3.92628787666155,-6.16964058180633));
#28342=CARTESIAN_POINT('Ctrl Pts',(41.0436902111697,-5.84735619130035,-4.3917544121835));
#28343=CARTESIAN_POINT('Ctrl Pts',(40.9775196763557,-6.58161740914491,-2.21598218059335));
#28344=CARTESIAN_POINT('Ctrl Pts',(40.9559770054392,-6.8206656173423,-1.50763147274297));
#28345=CARTESIAN_POINT('Ctrl Pts',(40.9344343345228,-6.93392271839034,-0.75710834412651));
#28346=CARTESIAN_POINT('Ctrl Pts',(40.9128916636063,-6.92852880502623,-0.00501897357509773));
#28347=CARTESIAN_POINT('Ctrl Pts',(40.7335483363939,-6.93403978357422,-0.00202363712922985));
#28348=CARTESIAN_POINT('Ctrl Pts',(40.7537217634838,-6.93745058116421,-0.706445496939072));
#28349=CARTESIAN_POINT('Ctrl Pts',(40.7738951905736,-6.83493540187031,-1.410290980689));
#28350=CARTESIAN_POINT('Ctrl Pts',(40.7940686176635,-6.62303379288307,-2.07890844114385));
#28351=CARTESIAN_POINT('Ctrl Pts',(40.8602391524775,-5.92797872206192,-4.2720298551332));
#28352=CARTESIAN_POINT('Ctrl Pts',(40.9264096872915,-4.05604043060457,-6.08613469797778));
#28353=CARTESIAN_POINT('Ctrl Pts',(40.9925802221056,-1.84572944398094,-6.69502852409246));
#28354=CARTESIAN_POINT('Ctrl Pts',(41.0587507569196,0.364581542642692,-7.30392235020714));
#28355=CARTESIAN_POINT('Ctrl Pts',(41.1249212917337,2.91326522443259,-6.70760515959187));
#28356=CARTESIAN_POINT('Ctrl Pts',(41.1910918265477,4.62679641577792,-5.17890139624333));
#28357=CARTESIAN_POINT('Ctrl Pts',(41.2572623613617,6.34032760712328,-3.65019763289477));
#28358=CARTESIAN_POINT('Ctrl Pts',(41.3234328961758,7.21870630802407,-1.18910729681289));
#28359=CARTESIAN_POINT('Ctrl Pts',(41.3896034309898,6.86030974856457,1.07908058031658));
#28360=CARTESIAN_POINT('Ctrl Pts',(41.4557739658038,6.50191318910508,3.34726845744604));
#28361=CARTESIAN_POINT('Ctrl Pts',(41.5219445006179,4.90674136928536,5.42255387562307));
#28362=CARTESIAN_POINT('Ctrl Pts',(41.5881150354319,2.81038650873806,6.35073631875021));
#28363=CARTESIAN_POINT('Ctrl Pts',(41.6542855702459,0.714031648190772,7.27891876187734));
#28364=CARTESIAN_POINT('Ctrl Pts',(41.72045610506,-1.88350625308409,7.05999822995456));
#28365=CARTESIAN_POINT('Ctrl Pts',(41.786626639874,-3.81008929259621,5.80255603254067));
#28366=CARTESIAN_POINT('Ctrl Pts',(41.8197119072811,-4.77338081235228,5.17383493383372));
#28367=CARTESIAN_POINT('Ctrl Pts',(41.8527971746881,-5.56893361666766,4.28548341875398));
#28368=CARTESIAN_POINT('Ctrl Pts',(41.8858824420951,-6.11177954673742,3.26548221666705));
#28369=CARTESIAN_POINT('Ctrl Pts',(41.9184377401947,-6.64593001492546,2.26181968653242));
#28370=CARTESIAN_POINT('Ctrl Pts',(41.9509930382943,-6.93540463039963,1.13069129491634));
#28371=CARTESIAN_POINT('Ctrl Pts',(41.983548336394,-6.93579090859155,-0.000199833497099776));
#28372=CARTESIAN_POINT('Origin',(29.75,0.,0.));
#28373=CARTESIAN_POINT('',(43.4128916636063,-6.93181729306353,0.00373977463357647));
#28374=CARTESIAN_POINT('',(43.2335483363939,-6.93333665186083,0.000459679647765049));
#28375=CARTESIAN_POINT('',(29.75,-6.933,-8.4904762584886E-16));
#28376=CARTESIAN_POINT('Ctrl Pts',(43.4128916636063,-6.93014855072287,0.00901641594148822));
#28377=CARTESIAN_POINT('Ctrl Pts',(43.3951474189579,-6.93567118806017,0.627760842080671));
#28378=CARTESIAN_POINT('Ctrl Pts',(43.3774031743095,-6.85978677319659,1.24489869731294));
#28379=CARTESIAN_POINT('Ctrl Pts',(43.3596589296611,-6.6972076135722,1.83780692661128));
#28380=CARTESIAN_POINT('Ctrl Pts',(43.293488394847,-6.09092934390644,4.04883677914626));
#28381=CARTESIAN_POINT('Ctrl Pts',(43.227317860033,-4.27904055528442,5.92292011921481));
#28382=CARTESIAN_POINT('Ctrl Pts',(43.1611473252189,-2.08674303097735,6.62056949597221));
#28383=CARTESIAN_POINT('Ctrl Pts',(43.1280620578119,-0.990594268823833,
6.96939418435091));
#28384=CARTESIAN_POINT('Ctrl Pts',(43.0949767904049,0.200656677250987,7.02411038190183));
#28385=CARTESIAN_POINT('Ctrl Pts',(43.0618915229979,1.33413363877489,6.79980225956431));
#28386=CARTESIAN_POINT('Ctrl Pts',(43.0288062555909,2.46761060029882,6.57549413722679));
#28387=CARTESIAN_POINT('Ctrl Pts',(42.9957209881839,3.54331357727186,6.07216169500083));
#28388=CARTESIAN_POINT('Ctrl Pts',(42.9626357207769,4.42791770297886,5.33843456580973));
#28389=CARTESIAN_POINT('Ctrl Pts',(42.9295504533698,5.31252182868585,4.60470743661862));
#28390=CARTESIAN_POINT('Ctrl Pts',(42.8964651859628,6.00602710312679,3.64058562046237));
#28391=CARTESIAN_POINT('Ctrl Pts',(42.8633799185557,6.43599643445051,2.56810693527878));
#28392=CARTESIAN_POINT('Ctrl Pts',(42.8302946511487,6.86596576577423,1.49562825009519));
#28393=CARTESIAN_POINT('Ctrl Pts',(42.7972093837417,7.03239915398073,0.314792695884272));
#28394=CARTESIAN_POINT('Ctrl Pts',(42.7641241163347,6.89221272945286,-0.826946564354824));
#28395=CARTESIAN_POINT('Ctrl Pts',(42.6979535815207,6.61183988039712,-3.11042508483302));
#28396=CARTESIAN_POINT('Ctrl Pts',(42.6317830467066,5.10498778040392,-5.23751842942387));
#28397=CARTESIAN_POINT('Ctrl Pts',(42.5656125118926,3.04413503102753,-6.24206424443556));
#28398=CARTESIAN_POINT('Ctrl Pts',(42.4994419770785,0.983282281651154,-7.24661005944724));
#28399=CARTESIAN_POINT('Ctrl Pts',(42.4332714422645,-1.63157111710844,-7.12860834487975));
#28400=CARTESIAN_POINT('Ctrl Pts',(42.3671009074505,-3.5967532801185,-5.94067593687986));
#28401=CARTESIAN_POINT('Ctrl Pts',(42.3009303726365,-5.5619354431286,-4.75274352887994));
#28402=CARTESIAN_POINT('Ctrl Pts',(42.2347598378224,-6.87744637038917,-2.49488042744759));
#28403=CARTESIAN_POINT('Ctrl Pts',(42.1685893030084,-6.94179248980091,-0.199453687883419));
#28404=CARTESIAN_POINT('Ctrl Pts',(42.1666900898743,-6.94363933893783,-0.13357081986297));
#28405=CARTESIAN_POINT('Ctrl Pts',(42.1647908767403,-6.94445548720937,-0.067657007178727));
#28406=CARTESIAN_POINT('Ctrl Pts',(42.1628916636063,-6.94425388693856,-0.00173762222092533));
#28407=CARTESIAN_POINT('Ctrl Pts',(41.983548336394,-6.93579090859155,-0.000199833497099776));
#28408=CARTESIAN_POINT('Ctrl Pts',(41.9840783057013,-6.93579719683334,-0.0186096660913617));
#28409=CARTESIAN_POINT('Ctrl Pts',(41.9846082750087,-6.93572687451181,-0.0370194358091072));
#28410=CARTESIAN_POINT('Ctrl Pts',(41.9851382443161,-6.93557975002843,-0.0554285917301944));
#28411=CARTESIAN_POINT('Ctrl Pts',(42.0182235117232,-6.92639496742555,-1.20468730894637));
#28412=CARTESIAN_POINT('Ctrl Pts',(42.0513087791302,-6.61788634639566,-2.35155385428462));
#28413=CARTESIAN_POINT('Ctrl Pts',(42.0843940465372,-6.05880726310654,-3.36274856089688));
#28414=CARTESIAN_POINT('Ctrl Pts',(42.1174793139442,-5.49972817981741,-4.37394326750917));
#28415=CARTESIAN_POINT('Ctrl Pts',(42.1505645813512,-4.69007863426907,-5.24946613539546));
#28416=CARTESIAN_POINT('Ctrl Pts',(42.1836498487583,-3.71686142459988,-5.8627108131522));
#28417=CARTESIAN_POINT('Ctrl Pts',(42.2498203835723,-1.77042700526154,-7.08920016866564));
#28418=CARTESIAN_POINT('Ctrl Pts',(42.3159909183863,0.830278070560082,-7.26657676366079));
#28419=CARTESIAN_POINT('Ctrl Pts',(42.3821614532004,2.91153018628898,-6.30500722387515));
#28420=CARTESIAN_POINT('Ctrl Pts',(42.4483319880144,4.99278230201796,-5.34343768408949));
#28421=CARTESIAN_POINT('Ctrl Pts',(42.5145025228284,6.55458145765417,-3.24292200952291));
#28422=CARTESIAN_POINT('Ctrl Pts',(42.5806730576425,6.87668020567494,-0.969295669001434));
#28423=CARTESIAN_POINT('Ctrl Pts',(42.6468435924565,7.1987789536957,1.30433067151996));
#28424=CARTESIAN_POINT('Ctrl Pts',(42.7130141272706,6.28117729410115,3.75106767799625));
#28425=CARTESIAN_POINT('Ctrl Pts',(42.7791846620846,4.54343198507275,5.2521891190326));
#28426=CARTESIAN_POINT('Ctrl Pts',(42.8453551968986,2.80568667604431,6.75331056006899));
#28427=CARTESIAN_POINT('Ctrl Pts',(42.9115257317127,0.247797717581995,7.30881643566538));
#28428=CARTESIAN_POINT('Ctrl Pts',(42.9776962665267,-1.95249909982447,6.66467338914477));
#28429=CARTESIAN_POINT('Ctrl Pts',(43.0438668013407,-4.15279591723087,6.02053034262418));
#28430=CARTESIAN_POINT('Ctrl Pts',(43.1100373361548,-5.99550059358143,4.17673837398668));
#28431=CARTESIAN_POINT('Ctrl Pts',(43.1762078709688,-6.6554146239929,1.9727881566635));
#28432=CARTESIAN_POINT('Ctrl Pts',(43.1953213594438,-6.84603208311179,1.33617282331664));
#28433=CARTESIAN_POINT('Ctrl Pts',(43.2144348479189,-6.93796286882622,0.669507523321825));
#28434=CARTESIAN_POINT('Ctrl Pts',(43.2335483363939,-6.93462080470656,0.00221311993343605));
#28435=CARTESIAN_POINT('Origin',(29.75,0.,0.));
#28436=CARTESIAN_POINT('',(44.6628916636063,-6.9275833124368,-0.00244717393932553));
#28437=CARTESIAN_POINT('',(44.4835483363939,-6.92717195859874,0.000292485364254664));
#28438=CARTESIAN_POINT('',(29.75,-6.933,-8.4904762584886E-16));
#28439=CARTESIAN_POINT('Ctrl Pts',(44.6628916636063,-6.933,-1.39055433834301E-13));
#28440=CARTESIAN_POINT('Ctrl Pts',(44.6056674683212,-6.93300000000004,1.99420935701617));
#28441=CARTESIAN_POINT('Ctrl Pts',(44.5484432730361,-6.02307502629254,3.97063309653039));
#28442=CARTESIAN_POINT('Ctrl Pts',(44.491219077751,-4.50798484753988,5.26731066241122));
#28443=CARTESIAN_POINT('Ctrl Pts',(44.4339948824659,-2.99289466878721,6.56398822829204));
#28444=CARTESIAN_POINT('Ctrl Pts',(44.3767706871808,-0.899664345628768,
7.15779044292411));
#28445=CARTESIAN_POINT('Ctrl Pts',(44.3195464918957,1.0706237168185,6.84983604599305));
#28446=CARTESIAN_POINT('Ctrl Pts',(44.2623222966106,3.04091177926578,6.54188164906199));
#28447=CARTESIAN_POINT('Ctrl Pts',(44.2050981013255,4.85311303639891,5.33766370386393));
#28448=CARTESIAN_POINT('Ctrl Pts',(44.1478739060404,5.90026971493769,3.64050907030721));
#28449=CARTESIAN_POINT('Ctrl Pts',(44.0906497107553,6.94742639347648,1.9433544367505));
#28450=CARTESIAN_POINT('Ctrl Pts',(44.0334255154702,7.2108600852751,-0.216464293124145));
#28451=CARTESIAN_POINT('Ctrl Pts',(43.9762013201851,6.60233935006075,-2.115562361794));
#28452=CARTESIAN_POINT('Ctrl Pts',(43.9189771249,5.99381861484639,-4.01466043046386));
#28453=CARTESIAN_POINT('Ctrl Pts',(43.8617529296149,4.52419779647272,-5.61916312790462));
#28454=CARTESIAN_POINT('Ctrl Pts',(43.8045287343298,2.68569473000373,-6.39167683923634));
#28455=CARTESIAN_POINT('Ctrl Pts',(43.7473045390448,0.847191663534734,-7.16419055056806));
#28456=CARTESIAN_POINT('Ctrl Pts',(43.6900803437597,-1.3273997899421,-7.0909357462378));
#28457=CARTESIAN_POINT('Ctrl Pts',(43.6328561484746,-3.10974706736229,-6.19644754492699));
#28458=CARTESIAN_POINT('Ctrl Pts',(43.5756319531895,-4.89209434478247,-5.30195934361617));
#28459=CARTESIAN_POINT('Ctrl Pts',(43.5184077579044,-6.2504052505868,-3.60219296582628));
#28460=CARTESIAN_POINT('Ctrl Pts',(43.4611835626193,-6.72974280712775,-1.66644854403378));
#28461=CARTESIAN_POINT('Ctrl Pts',(43.4450862629483,-6.86458158035576,-1.12191912096703));
#28462=CARTESIAN_POINT('Ctrl Pts',(43.4289889632773,-6.93299999999999,-0.560975745777965));
#28463=CARTESIAN_POINT('Ctrl Pts',(43.4128916636063,-6.933,-9.18709552877317E-14));
#28464=CARTESIAN_POINT('Ctrl Pts',(43.2335483363939,-6.933,-5.62244695245795E-12));
#28465=CARTESIAN_POINT('Ctrl Pts',(43.290772531679,-6.93299999999838,-1.99420935702193));
#28466=CARTESIAN_POINT('Ctrl Pts',(43.3479967269641,-6.02307502628924,-3.97063309653539));
#28467=CARTESIAN_POINT('Ctrl Pts',(43.4052209222492,-4.5079848475355,-5.26731066241496));
#28468=CARTESIAN_POINT('Ctrl Pts',(43.4624451175343,-2.99289466878176,-6.56398822829453));
#28469=CARTESIAN_POINT('Ctrl Pts',(43.5196693128194,-0.89966434562282,-7.15779044292486));
#28470=CARTESIAN_POINT('Ctrl Pts',(43.5768935081045,1.0706237168242,-6.84983604599216));
#28471=CARTESIAN_POINT('Ctrl Pts',(43.6341177033896,3.04091177927121,-6.54188164905946));
#28472=CARTESIAN_POINT('Ctrl Pts',(43.6913418986747,4.85311303640335,-5.33766370385989));
#28473=CARTESIAN_POINT('Ctrl Pts',(43.7485660939598,5.90026971494072,-3.64050907030231));
#28474=CARTESIAN_POINT('Ctrl Pts',(43.8057902892449,6.94742639347808,-1.94335443674474));
#28475=CARTESIAN_POINT('Ctrl Pts',(43.86301448453,7.21086008527492,0.216464293130101));
#28476=CARTESIAN_POINT('Ctrl Pts',(43.9202386798151,6.60233935005901,2.11556236179944));
#28477=CARTESIAN_POINT('Ctrl Pts',(43.9774628751002,5.99381861484309,4.0146604304688));
#28478=CARTESIAN_POINT('Ctrl Pts',(44.0346870703853,4.52419779646809,5.61916312790834));
#28479=CARTESIAN_POINT('Ctrl Pts',(44.0919112656704,2.68569472999846,6.39167683923855));
#28480=CARTESIAN_POINT('Ctrl Pts',(44.1491354609555,0.847191663528831,7.16419055056876));
#28481=CARTESIAN_POINT('Ctrl Pts',(44.2063596562406,-1.32739978994794,7.09093574623671));
#28482=CARTESIAN_POINT('Ctrl Pts',(44.2635838515257,-3.10974706736739,6.19644754492442));
#28483=CARTESIAN_POINT('Ctrl Pts',(44.3208080468107,-4.89209434478684,5.30195934361214));
#28484=CARTESIAN_POINT('Ctrl Pts',(44.3780322420958,-6.25040525058977,3.60219296582113));
#28485=CARTESIAN_POINT('Ctrl Pts',(44.4352564373809,-6.72974280712912,1.66644854402824));
#28486=CARTESIAN_POINT('Ctrl Pts',(44.4513537370519,-6.86458158035669,1.12191912096138));
#28487=CARTESIAN_POINT('Ctrl Pts',(44.4674510367229,-6.93300000000046,0.560975745772253));
#28488=CARTESIAN_POINT('Ctrl Pts',(44.4835483363939,-6.933,-5.62078161792101E-12));
#28489=CARTESIAN_POINT('Origin',(29.75,0.,0.));
#28490=CARTESIAN_POINT('',(45.9128916636063,-6.93405647677003,-0.000332869569125593));
#28491=CARTESIAN_POINT('',(45.7335483363939,-6.94075830301621,-0.00694975155396205));
#28492=CARTESIAN_POINT('',(29.75,-6.933,-8.4904762584886E-16));
#28493=CARTESIAN_POINT('Ctrl Pts',(45.9128916636063,-6.94022992359918,-0.00227796920823947));
#28494=CARTESIAN_POINT('Ctrl Pts',(45.8889457708,-6.93676910672981,0.831764088413885));
#28495=CARTESIAN_POINT('Ctrl Pts',(45.8649998779937,-6.7789353365392,1.66778218659105));
#28496=CARTESIAN_POINT('Ctrl Pts',(45.8410539851874,-6.48203451786819,2.44958197340933));
#28497=CARTESIAN_POINT('Ctrl Pts',(45.8079687177804,-6.07181623707313,3.52976951182737));
#28498=CARTESIAN_POINT('Ctrl Pts',(45.7748834503734,-5.39611816499337,4.50645398362649));
#28499=CARTESIAN_POINT('Ctrl Pts',(45.7417981829664,-4.52512595472309,5.25628898479498));
#28500=CARTESIAN_POINT('Ctrl Pts',(45.7087129155594,-3.65413374445282,6.00612398596347));
#28501=CARTESIAN_POINT('Ctrl Pts',(45.6756276481523,-2.58784739599202,6.52910951650133));
#28502=CARTESIAN_POINT('Ctrl Pts',(45.6425423807453,-1.45867703652056,6.77417778320101));
#28503=CARTESIAN_POINT('Ctrl Pts',(45.6094571133383,-0.329506677049107,
7.01924604990069));
#28504=CARTESIAN_POINT('Ctrl Pts',(45.5763718459313,0.862547693433012,6.9863970527622));
#28505=CARTESIAN_POINT('Ctrl Pts',(45.5432865785243,1.9649124195632,6.65774407076276));
#28506=CARTESIAN_POINT('Ctrl Pts',(45.4771160437103,4.16964187182359,6.00043810676387));
#28507=CARTESIAN_POINT('Ctrl Pts',(45.4109455088962,6.01561274667627,4.15991620332117));
#28508=CARTESIAN_POINT('Ctrl Pts',(45.3447749740822,6.66235862434885,1.96038304403867));
#28509=CARTESIAN_POINT('Ctrl Pts',(45.2786044392681,7.30910450202143,-0.239150115243826));
#28510=CARTESIAN_POINT('Ctrl Pts',(45.2124339044541,6.75662538251391,-2.79769453036612));
#28511=CARTESIAN_POINT('Ctrl Pts',(45.1462633696401,5.25756100615865,-4.53721467550155));
#28512=CARTESIAN_POINT('Ctrl Pts',(45.080092834826,3.75849662980338,-6.27673482063697));
#28513=CARTESIAN_POINT('Ctrl Pts',(45.013922300012,1.31284699660037,-7.19723069578553));
#28514=CARTESIAN_POINT('Ctrl Pts',(44.947751765198,-0.961158843812644,-6.87782221506396));
#28515=CARTESIAN_POINT('Ctrl Pts',(44.8815812303839,-3.23516468422572,-6.55841373434238));
#28516=CARTESIAN_POINT('Ctrl Pts',(44.8154106955699,-5.3375267318488,-4.9991008977506));
#28517=CARTESIAN_POINT('Ctrl Pts',(44.7492401607558,-6.30155803282916,-2.91898792009768));
#28518=CARTESIAN_POINT('Ctrl Pts',(44.7204573283726,-6.72089197695158,-2.01418122113218));
#28519=CARTESIAN_POINT('Ctrl Pts',(44.6916744959895,-6.92484549387806,-1.01083536103422));
#28520=CARTESIAN_POINT('Ctrl Pts',(44.6628916636063,-6.92069769006582,-0.0055579894376756));
#28521=CARTESIAN_POINT('Ctrl Pts',(44.4835483363939,-6.91974231982792,0.000665348317145921));
#28522=CARTESIAN_POINT('Ctrl Pts',(44.5109619249504,-6.92284490954652,-0.957366321970913));
#28523=CARTESIAN_POINT('Ctrl Pts',(44.538375513507,-6.73728033370965,-1.91504791652457));
#28524=CARTESIAN_POINT('Ctrl Pts',(44.5657891020636,-6.35676001150659,-2.78891360290006));
#28525=CARTESIAN_POINT('Ctrl Pts',(44.5988743694706,-5.89751270836997,-3.84357595955975));
#28526=CARTESIAN_POINT('Ctrl Pts',(44.6319596368777,-5.15429468801847,-4.77615284809136));
#28527=CARTESIAN_POINT('Ctrl Pts',(44.6650449042847,-4.23912218741068,-5.48152044742052));
#28528=CARTESIAN_POINT('Ctrl Pts',(44.6981301716917,-3.32394968680288,-6.18688804674967));
#28529=CARTESIAN_POINT('Ctrl Pts',(44.7312154390987,-2.23682270593883,-6.66504635687637));
#28530=CARTESIAN_POINT('Ctrl Pts',(44.7643007065057,-1.10213028992486,-6.84767461418953));
#28531=CARTESIAN_POINT('Ctrl Pts',(44.7973859739127,0.0325621260890784,
-7.03030287150269));
#28532=CARTESIAN_POINT('Ctrl Pts',(44.8304712413197,1.214819977253,-6.91740107600231));
#28533=CARTESIAN_POINT('Ctrl Pts',(44.8635565087267,2.30509895463997,-6.53481003125602));
#28534=CARTESIAN_POINT('Ctrl Pts',(44.8966417761338,3.39537793202696,-6.15221898650973));
#28535=CARTESIAN_POINT('Ctrl Pts',(44.9297270435408,4.39367803563707,-5.49993869251753));
#28536=CARTESIAN_POINT('Ctrl Pts',(44.9628123109478,5.16065519039781,-4.64263663602381));
#28537=CARTESIAN_POINT('Ctrl Pts',(45.0289828457619,6.69460949991927,-2.92803252303641));
#28538=CARTESIAN_POINT('Ctrl Pts',(45.0951533805759,7.30327201404325,-0.393341360043043));
#28539=CARTESIAN_POINT('Ctrl Pts',(45.1613239153899,6.70230282379522,1.81913742662187));
#28540=CARTESIAN_POINT('Ctrl Pts',(45.2274944502039,6.10133363354718,4.03161621328681));
#28541=CARTESIAN_POINT('Ctrl Pts',(45.293664985018,4.2907327389271,5.92188262362324));
#28542=CARTESIAN_POINT('Ctrl Pts',(45.3598355198321,2.10267690769521,6.61868677056951));
#28543=CARTESIAN_POINT('Ctrl Pts',(45.4260060546461,-0.0853789235366806,
7.31549091751577));
#28544=CARTESIAN_POINT('Ctrl Pts',(45.4921765894601,-2.65088969138045,6.81883280107182));
#28545=CARTESIAN_POINT('Ctrl Pts',(45.5583471242741,-4.42082201083547,5.35580035975756));
#28546=CARTESIAN_POINT('Ctrl Pts',(45.616747528314,-5.98291853718214,4.06456573491428));
#28547=CARTESIAN_POINT('Ctrl Pts',(45.675147932354,-6.92530945898835,2.02058625327023));
#28548=CARTESIAN_POINT('Ctrl Pts',(45.7335483363939,-6.94075830301621,-0.00694975155396205));
#28549=CARTESIAN_POINT('Origin',(29.75,0.,0.));
#28550=CARTESIAN_POINT('',(47.1628916636063,-6.933,-3.32511795875234E-13));
#28551=CARTESIAN_POINT('',(46.9835483363939,-6.93618751727322,0.00576443580885351));
#28552=CARTESIAN_POINT('',(29.75,-6.933,-8.4904762584886E-16));
#28553=CARTESIAN_POINT('Ctrl Pts',(47.1628916636063,-6.933,-1.35447209004269E-13));
#28554=CARTESIAN_POINT('Ctrl Pts',(47.1056674683212,-6.93300000000004,1.99420935701617));
#28555=CARTESIAN_POINT('Ctrl Pts',(47.0484432730361,-6.02307502629254,3.97063309653039));
#28556=CARTESIAN_POINT('Ctrl Pts',(46.991219077751,-4.50798484753988,5.26731066241122));
#28557=CARTESIAN_POINT('Ctrl Pts',(46.9339948824659,-2.99289466878721,6.56398822829204));
#28558=CARTESIAN_POINT('Ctrl Pts',(46.8767706871808,-0.899664345628765,
7.15779044292411));
#28559=CARTESIAN_POINT('Ctrl Pts',(46.8195464918957,1.07062371681851,6.84983604599305));
#28560=CARTESIAN_POINT('Ctrl Pts',(46.7623222966106,3.04091177926578,6.54188164906199));
#28561=CARTESIAN_POINT('Ctrl Pts',(46.7050981013255,4.85311303639891,5.33766370386392));
#28562=CARTESIAN_POINT('Ctrl Pts',(46.6478739060404,5.90026971493769,3.64050907030721));
#28563=CARTESIAN_POINT('Ctrl Pts',(46.5906497107553,6.94742639347648,1.94335443675049));
#28564=CARTESIAN_POINT('Ctrl Pts',(46.5334255154702,7.2108600852751,-0.216464293124149));
#28565=CARTESIAN_POINT('Ctrl Pts',(46.4762013201851,6.60233935006075,-2.11556236179401));
#28566=CARTESIAN_POINT('Ctrl Pts',(46.4189771249,5.99381861484639,-4.01466043046386));
#28567=CARTESIAN_POINT('Ctrl Pts',(46.3617529296149,4.52419779647272,-5.61916312790462));
#28568=CARTESIAN_POINT('Ctrl Pts',(46.3045287343298,2.68569473000372,-6.39167683923634));
#28569=CARTESIAN_POINT('Ctrl Pts',(46.2473045390448,0.847191663534731,-7.16419055056806));
#28570=CARTESIAN_POINT('Ctrl Pts',(46.1900803437597,-1.32739978994211,-7.0909357462378));
#28571=CARTESIAN_POINT('Ctrl Pts',(46.1328561484746,-3.10974706736229,-6.19644754492698));
#28572=CARTESIAN_POINT('Ctrl Pts',(46.0756319531895,-4.89209434478247,-5.30195934361617));
#28573=CARTESIAN_POINT('Ctrl Pts',(46.0184077579044,-6.25040525058681,-3.60219296582627));
#28574=CARTESIAN_POINT('Ctrl Pts',(45.9611835626193,-6.72974280712775,-1.66644854403378));
#28575=CARTESIAN_POINT('Ctrl Pts',(45.9450862629483,-6.86458158035576,-1.12191912096703));
#28576=CARTESIAN_POINT('Ctrl Pts',(45.9289889632773,-6.93299999999999,-0.560975745777962));
#28577=CARTESIAN_POINT('Ctrl Pts',(45.9128916636063,-6.933,-8.82627304576999E-14));
#28578=CARTESIAN_POINT('Ctrl Pts',(45.7335483363939,-6.94075830301621,-0.00694975155396205));
#28579=CARTESIAN_POINT('Ctrl Pts',(45.741318467168,-6.94281376034358,-0.276711924704654));
#28580=CARTESIAN_POINT('Ctrl Pts',(45.7490885979422,-6.92846039015388,-0.546183013675027));
#28581=CARTESIAN_POINT('Ctrl Pts',(45.7568587287163,-6.89697457304899,-0.813551385903551));
#28582=CARTESIAN_POINT('Ctrl Pts',(45.8230292635303,-6.62884094474111,-3.09046392406575));
#28583=CARTESIAN_POINT('Ctrl Pts',(45.8891997983443,-5.11821981705906,-5.21488223420553));
#28584=CARTESIAN_POINT('Ctrl Pts',(45.9553703331584,-3.05520819225478,-6.23314846849565));
#28585=CARTESIAN_POINT('Ctrl Pts',(45.9884556005654,-2.02370237985268,-6.74228158564068));
#28586=CARTESIAN_POINT('Ctrl Pts',(46.0215408679724,-0.854098943170027,
-6.97487668382332));
#28587=CARTESIAN_POINT('Ctrl Pts',(46.0546261353794,0.300191666840078,-6.92294072619767));
#28588=CARTESIAN_POINT('Ctrl Pts',(46.0877114027864,1.45448227685025,-6.87100476857203));
#28589=CARTESIAN_POINT('Ctrl Pts',(46.1207966701934,2.59346006018791,-6.53453775513806));
#28590=CARTESIAN_POINT('Ctrl Pts',(46.1538819376005,3.57801869911607,-5.94164295347351));
#28591=CARTESIAN_POINT('Ctrl Pts',(46.1869672050075,4.56257733804423,-5.34874815180897));
#28592=CARTESIAN_POINT('Ctrl Pts',(46.2200524724145,5.39271683256293,-4.49942556191382));
#28593=CARTESIAN_POINT('Ctrl Pts',(46.2531377398216,5.9785317786885,-3.50348128388014));
#28594=CARTESIAN_POINT('Ctrl Pts',(46.2862230072286,6.56434672481405,-2.50753700584648));
#28595=CARTESIAN_POINT('Ctrl Pts',(46.3193082746355,6.9058371225465,-1.36497103967435));
#28596=CARTESIAN_POINT('Ctrl Pts',(46.3523935420426,6.93831117486302,-0.215116175824418));
#28597=CARTESIAN_POINT('Ctrl Pts',(46.4185640768566,7.00325927949605,2.08459355187545));
#28598=CARTESIAN_POINT('Ctrl Pts',(46.4847346116707,5.83214200246525,4.41345887028628));
#28599=CARTESIAN_POINT('Ctrl Pts',(46.5509051464847,3.94507643800014,5.7154611377496));
#28600=CARTESIAN_POINT('Ctrl Pts',(46.6170756812988,2.05801087353504,7.01746340521292));
#28601=CARTESIAN_POINT('Ctrl Pts',(46.6832462161128,-0.545002978364427,
7.29260262172879));
#28602=CARTESIAN_POINT('Ctrl Pts',(46.7494167509268,-2.66599822587748,6.41254381697971));
#28603=CARTESIAN_POINT('Ctrl Pts',(46.8155872857408,-4.78699347339055,5.53248501223062));
#28604=CARTESIAN_POINT('Ctrl Pts',(46.8817578205549,-6.42597011651721,3.49722818621661));
#28605=CARTESIAN_POINT('Ctrl Pts',(46.9479283553689,-6.83353573651531,1.23735770205496));
#28606=CARTESIAN_POINT('Ctrl Pts',(46.9598016823773,-6.90666737882698,0.831857257932137));
#28607=CARTESIAN_POINT('Ctrl Pts',(46.9716750093856,-6.94015126573288,0.419124925177673));
#28608=CARTESIAN_POINT('Ctrl Pts',(46.9835483363939,-6.93618751727322,0.00576443580885351));
#28609=CARTESIAN_POINT('Origin',(29.75,0.,0.));
#28610=CARTESIAN_POINT('',(48.4128916636063,-6.933,-3.80251385934116E-13));
#28611=CARTESIAN_POINT('',(48.2335483363939,-6.92348246561576,0.00082620762749036));
#28612=CARTESIAN_POINT('',(29.75,-6.933,-8.4904762584886E-16));
#28613=CARTESIAN_POINT('Ctrl Pts',(48.4128916636063,-6.930055142889,-0.000658831376577074));
#28614=CARTESIAN_POINT('Ctrl Pts',(48.3827441226422,-6.93264111678612,1.05251277108305));
#28615=CARTESIAN_POINT('Ctrl Pts',(48.352596581678,-6.69957236130202,2.10736732158826));
#28616=CARTESIAN_POINT('Ctrl Pts',(48.3224490407138,-6.23675887648899,3.04783130190406));
#28617=CARTESIAN_POINT('Ctrl Pts',(48.2562785058998,-5.2209342078818,5.11204624483563));
#28618=CARTESIAN_POINT('Ctrl Pts',(48.1901079710858,-3.0983046766226,6.6251798215178));
#28619=CARTESIAN_POINT('Ctrl Pts',(48.1239374362717,-0.821710974525657,
6.89600719207382));
#28620=CARTESIAN_POINT('Ctrl Pts',(48.0577669014577,1.45488272757128,7.16683456262985));
#28621=CARTESIAN_POINT('Ctrl Pts',(47.9915963666437,3.88544060050593,6.19535572705974));
#28622=CARTESIAN_POINT('Ctrl Pts',(47.9254258318296,5.35056611389629,4.42715563380048));
#28623=CARTESIAN_POINT('Ctrl Pts',(47.8592552970156,6.81569162728666,2.6589555405412));
#28624=CARTESIAN_POINT('Ctrl Pts',(47.7930847622015,7.3153847811327,0.0940341895926755));
#28625=CARTESIAN_POINT('Ctrl Pts',(47.7269142273875,6.62116992097035,-2.09484453425644));
#28626=CARTESIAN_POINT('Ctrl Pts',(47.6607436925735,5.92695506080801,-4.28372325810549));
#28627=CARTESIAN_POINT('Ctrl Pts',(47.5945731577595,4.03883218663742,-6.09655935485521));
#28628=CARTESIAN_POINT('Ctrl Pts',(47.5284026229454,1.8270659854587,-6.7001458195751));
#28629=CARTESIAN_POINT('Ctrl Pts',(47.4622320881314,-0.384700215720024,
-7.30373228429499));
#28630=CARTESIAN_POINT('Ctrl Pts',(47.3960615533173,-2.92010974390683,-6.69806911698503));
#28631=CARTESIAN_POINT('Ctrl Pts',(47.3298910185033,-4.63652755541892,-5.1661445156104));
#28632=CARTESIAN_POINT('Ctrl Pts',(47.2968057510963,-5.494736461175,-4.40018221492305));
#28633=CARTESIAN_POINT('Ctrl Pts',(47.2637204836893,-6.14819743776237,-3.40265455571952));
#28634=CARTESIAN_POINT('Ctrl Pts',(47.2306352162822,-6.53207817870433,-2.3128290041811));
#28635=CARTESIAN_POINT('Ctrl Pts',(47.2080540320569,-6.79408246070457,-1.56900695039511));
#28636=CARTESIAN_POINT('Ctrl Pts',(47.1854728478316,-6.93050914286102,-0.782190098558359));
#28637=CARTESIAN_POINT('Ctrl Pts',(47.1628916636063,-6.93309008421871,0.00326550207437409));
#28638=CARTESIAN_POINT('Ctrl Pts',(46.9835483363939,-6.93618751727322,0.00576443580885351));
#28639=CARTESIAN_POINT('Ctrl Pts',(47.0378455441996,-6.9180611341918,-1.88454991114452));
#28640=CARTESIAN_POINT('Ctrl Pts',(47.0921427520053,-6.11680353603182,-3.78800070978208));
#28641=CARTESIAN_POINT('Ctrl Pts',(47.146439959811,-4.74282239922126,-5.07304246071674));
#28642=CARTESIAN_POINT('Ctrl Pts',(47.2126104946251,-3.06838884505966,-6.63908799701747));
#28643=CARTESIAN_POINT('Ctrl Pts',(47.2787810294391,-0.543367139866965,
-7.28669492730971));
#28644=CARTESIAN_POINT('Ctrl Pts',(47.3449515642531,1.68960656755196,-6.73287951586954));
#28645=CARTESIAN_POINT('Ctrl Pts',(47.3780368316602,2.80609342126142,-6.45597181014945));
#28646=CARTESIAN_POINT('Ctrl Pts',(47.4111220990672,3.84956827552745,-5.87870851899626));
#28647=CARTESIAN_POINT('Ctrl Pts',(47.4442073664742,4.69769668825529,-5.09400325485192));
#28648=CARTESIAN_POINT('Ctrl Pts',(47.4772926338812,5.54582510098315,-4.30929799070757));
#28649=CARTESIAN_POINT('Ctrl Pts',(47.5103779012883,6.19860707217283,-3.31715075357204));
#28650=CARTESIAN_POINT('Ctrl Pts',(47.5434631686953,6.5679320432874,-2.22881301874882));
#28651=CARTESIAN_POINT('Ctrl Pts',(47.5765484361023,6.93725701440196,-1.14047528392563));
#28652=CARTESIAN_POINT('Ctrl Pts',(47.6096337035093,7.02312498544144,0.0440529485851764));
#28653=CARTESIAN_POINT('Ctrl Pts',(47.6427189709163,6.82774025790008,1.1828720581437));
#28654=CARTESIAN_POINT('Ctrl Pts',(47.6758042383233,6.63235553035873,2.32169116770218));
#28655=CARTESIAN_POINT('Ctrl Pts',(47.7088895057303,6.15571810423654,3.41480115430832));
#28656=CARTESIAN_POINT('Ctrl Pts',(47.7419747731374,5.43834849684116,4.31402394003972));
#28657=CARTESIAN_POINT('Ctrl Pts',(47.8081453079514,4.00360928205037,6.11246951150258));
#28658=CARTESIAN_POINT('Ctrl Pts',(47.8743158427655,1.60594134216666,7.13536627946652));
#28659=CARTESIAN_POINT('Ctrl Pts',(47.9404863775795,-0.675781576911461,
6.91183357576677));
#28660=CARTESIAN_POINT('Ctrl Pts',(48.0066569123935,-2.95750449598962,6.68830087206702));
#28661=CARTESIAN_POINT('Ctrl Pts',(48.0728274472075,-5.12328239426221,5.21833869670365));
#28662=CARTESIAN_POINT('Ctrl Pts',(48.1389979820216,-6.17527098918003,3.17715170479127));
#28663=CARTESIAN_POINT('Ctrl Pts',(48.1705147668124,-6.67632932642266,2.20494177294425));
#28664=CARTESIAN_POINT('Ctrl Pts',(48.2020315516031,-6.92471540330101,1.10314479520007));
#28665=CARTESIAN_POINT('Ctrl Pts',(48.2335483363939,-6.92348246561576,0.00082620762749036));
#28666=CARTESIAN_POINT('Origin',(29.75,0.,0.));
#28667=CARTESIAN_POINT('',(49.6628916636063,-6.93186465004489,-0.000678253275532354));
#28668=CARTESIAN_POINT('',(49.4835483363939,-6.93271820397492,-0.00595368521987888));
#28669=CARTESIAN_POINT('',(29.75,-6.933,-8.4904762584886E-16));
#28670=CARTESIAN_POINT('Ctrl Pts',(49.6628916636063,-6.933,-4.27990975992998E-13));
#28671=CARTESIAN_POINT('Ctrl Pts',(49.6056674683212,-6.93300000000012,1.99420935701588));
#28672=CARTESIAN_POINT('Ctrl Pts',(49.5484432730361,-6.02307502629271,3.97063309653014));
#28673=CARTESIAN_POINT('Ctrl Pts',(49.491219077751,-4.5079848475401,5.26731066241103));
#28674=CARTESIAN_POINT('Ctrl Pts',(49.4339948824659,-2.99289466878749,6.56398822829192));
#28675=CARTESIAN_POINT('Ctrl Pts',(49.3767706871808,-0.899664345629066,
7.15779044292407));
#28676=CARTESIAN_POINT('Ctrl Pts',(49.3195464918957,1.07062371681822,6.8498360459931));
#28677=CARTESIAN_POINT('Ctrl Pts',(49.2623222966106,3.0409117792655,6.54188164906212));
#28678=CARTESIAN_POINT('Ctrl Pts',(49.2050981013255,4.85311303639869,5.33766370386413));
#28679=CARTESIAN_POINT('Ctrl Pts',(49.1478739060404,5.90026971493754,3.64050907030746));
#28680=CARTESIAN_POINT('Ctrl Pts',(49.0906497107553,6.9474263934764,1.94335443675079));
#28681=CARTESIAN_POINT('Ctrl Pts',(49.0334255154702,7.21086008527511,-0.216464293123844));
#28682=CARTESIAN_POINT('Ctrl Pts',(48.9762013201851,6.60233935006084,-2.11556236179373));
#28683=CARTESIAN_POINT('Ctrl Pts',(48.9189771249,5.99381861484656,-4.01466043046361));
#28684=CARTESIAN_POINT('Ctrl Pts',(48.8617529296149,4.52419779647296,-5.61916312790443));
#28685=CARTESIAN_POINT('Ctrl Pts',(48.8045287343298,2.68569473000399,-6.39167683923622));
#28686=CARTESIAN_POINT('Ctrl Pts',(48.7473045390448,0.847191663535033,-7.16419055056802));
#28687=CARTESIAN_POINT('Ctrl Pts',(48.6900803437597,-1.32739978994181,-7.09093574623786));
#28688=CARTESIAN_POINT('Ctrl Pts',(48.6328561484746,-3.10974706736203,-6.19644754492712));
#28689=CARTESIAN_POINT('Ctrl Pts',(48.5756319531895,-4.89209434478225,-5.30195934361637));
#28690=CARTESIAN_POINT('Ctrl Pts',(48.5184077579044,-6.25040525058665,-3.60219296582654));
#28691=CARTESIAN_POINT('Ctrl Pts',(48.4611835626193,-6.72974280712768,-1.66644854403406));
#28692=CARTESIAN_POINT('Ctrl Pts',(48.4450862629483,-6.86458158035571,-1.12191912096732));
#28693=CARTESIAN_POINT('Ctrl Pts',(48.4289889632773,-6.93299999999997,-0.560975745778254));
#28694=CARTESIAN_POINT('Ctrl Pts',(48.4128916636063,-6.933,-3.80251385934116E-13));
#28695=CARTESIAN_POINT('Ctrl Pts',(48.2335483363939,-6.92348246561576,0.00082620762749036));
#28696=CARTESIAN_POINT('Ctrl Pts',(48.2682020864172,-6.92212680974468,-1.21120963401434));
#28697=CARTESIAN_POINT('Ctrl Pts',(48.3028558364405,-6.61898846170223,-2.42387608794565));
#28698=CARTESIAN_POINT('Ctrl Pts',(48.3375095864637,-6.01812611974246,-3.46560568327387));
#28699=CARTESIAN_POINT('Ctrl Pts',(48.4036801212778,-4.87079336382414,-5.4547642709652));
#28700=CARTESIAN_POINT('Ctrl Pts',(48.4698506560917,-2.63792856042451,-6.82066963788656));
#28701=CARTESIAN_POINT('Ctrl Pts',(48.5360211909058,-0.348187949984992,
-6.93605718476102));
#28702=CARTESIAN_POINT('Ctrl Pts',(48.6021917257198,1.94155266045456,-7.05144473163549));
#28703=CARTESIAN_POINT('Ctrl Pts',(48.6683622605339,4.288169077934,-5.91631445846307));
#28704=CARTESIAN_POINT('Ctrl Pts',(48.734532795348,5.63626081271754,-4.05203664585539));
#28705=CARTESIAN_POINT('Ctrl Pts',(48.767618062755,6.31030668010929,-3.11989773955158));
#28706=CARTESIAN_POINT('Ctrl Pts',(48.800703330162,6.73472137682705,-2.00547194838899));
#28707=CARTESIAN_POINT('Ctrl Pts',(48.833788597569,6.87603656298273,-0.858687673028613));
#28708=CARTESIAN_POINT('Ctrl Pts',(48.866873864976,7.0173517491384,0.288096602331795));
#28709=CARTESIAN_POINT('Ctrl Pts',(48.899959132383,6.87556742473195,1.46723936189003));
#28710=CARTESIAN_POINT('Ctrl Pts',(48.93304439979,6.4551917161997,2.53689548560685));
#28711=CARTESIAN_POINT('Ctrl Pts',(48.9661296671971,6.03481600766747,3.60655160932363));
#28712=CARTESIAN_POINT('Ctrl Pts',(48.9992149346041,5.33584891500949,4.56672109719906));
#28713=CARTESIAN_POINT('Ctrl Pts',(49.0323002020111,4.45156314573267,5.31044338025002));
#28714=CARTESIAN_POINT('Ctrl Pts',(49.0653854694181,3.5672773764558,6.05416566330103));
#28715=CARTESIAN_POINT('Ctrl Pts',(49.0984707368251,2.49767293056012,6.58144074152752));
#28716=CARTESIAN_POINT('Ctrl Pts',(49.1315560042321,1.36934097820534,6.80524372919427));
#28717=CARTESIAN_POINT('Ctrl Pts',(49.1977265390462,-0.887322926504155,
7.25284970452777));
#28718=CARTESIAN_POINT('Ctrl Pts',(49.2638970738602,-3.37889685704989,6.48656731762235));
#28719=CARTESIAN_POINT('Ctrl Pts',(49.3300676086743,-4.97740422569037,4.84309521823281));
#28720=CARTESIAN_POINT('Ctrl Pts',(49.3812278512475,-6.2133021214013,3.57243250554062));
#28721=CARTESIAN_POINT('Ctrl Pts',(49.4323880938207,-6.91534942433851,1.77740994335895));
#28722=CARTESIAN_POINT('Ctrl Pts',(49.4835483363939,-6.93271820397492,-0.00595368521987888));
#28723=CARTESIAN_POINT('Origin',(29.75,0.,0.));
#28724=CARTESIAN_POINT('',(50.9128916636063,-6.94407271247953,0.00085298068625117));
#28725=CARTESIAN_POINT('',(50.7335483363939,-6.94318480280473,0.00509973895979926));
#28726=CARTESIAN_POINT('',(29.75,-6.933,-8.4904762584886E-16));
#28727=CARTESIAN_POINT('Ctrl Pts',(50.9128916636063,-6.94407271247953,0.00085298068625117));
#28728=CARTESIAN_POINT('Ctrl Pts',(50.9096277418913,-6.94453748549343,0.113946146647875));
#28729=CARTESIAN_POINT('Ctrl Pts',(50.9063638201763,-6.9420222511174,0.227031117887721));
#28730=CARTESIAN_POINT('Ctrl Pts',(50.9030998984613,-6.93646428876074,0.339981307628455));
#28731=CARTESIAN_POINT('Ctrl Pts',(50.8369293636473,-6.82378593010814,2.62985683624597));
#28732=CARTESIAN_POINT('Ctrl Pts',(50.7707588288332,-5.46052333404185,4.86433614825873));
#28733=CARTESIAN_POINT('Ctrl Pts',(50.7045882940192,-3.47272360578677,6.0140215748597));
#28734=CARTESIAN_POINT('Ctrl Pts',(50.6384177592051,-1.48492387753177,7.16370700146062));
#28735=CARTESIAN_POINT('Ctrl Pts',(50.5722472243911,1.12741298291193,7.22859854264998));
#28736=CARTESIAN_POINT('Ctrl Pts',(50.5060766895771,3.16984320685072,6.17902571519562));
#28737=CARTESIAN_POINT('Ctrl Pts',(50.439906154763,5.21227343078961,5.12945288774122));
#28738=CARTESIAN_POINT('Ctrl Pts',(50.373735619949,6.68479701822344,2.96541569164298));
#28739=CARTESIAN_POINT('Ctrl Pts',(50.307565085135,6.9110291867925,0.683958842396304));
#28740=CARTESIAN_POINT('Ctrl Pts',(50.2413945503209,7.13726135536154,-1.59749800685027));
#28741=CARTESIAN_POINT('Ctrl Pts',(50.1752240155069,6.11720210506592,-3.99637450924526));
#28742=CARTESIAN_POINT('Ctrl Pts',(50.1090534806928,4.32045530461438,-5.43324055137998));
#28743=CARTESIAN_POINT('Ctrl Pts',(50.0759682132858,3.42208190438857,-6.15167357244737));
#28744=CARTESIAN_POINT('Ctrl Pts',(50.0428829458788,2.32953661662386,-6.62960397844963));
#28745=CARTESIAN_POINT('Ctrl Pts',(50.0097976784718,1.19094947366404,-6.82633596349212));
#28746=CARTESIAN_POINT('Ctrl Pts',(49.9767124110648,0.0523623307042911,
-7.0230679485346));
#28747=CARTESIAN_POINT('Ctrl Pts',(49.9436271436578,-1.13226666745058,-6.93860151261728));
#28748=CARTESIAN_POINT('Ctrl Pts',(49.9105418762507,-2.22104060749918,-6.57056446719955));
#28749=CARTESIAN_POINT('Ctrl Pts',(49.8774566088437,-3.30981454754782,-6.20252742178181));
#28750=CARTESIAN_POINT('Ctrl Pts',(49.8443713414367,-4.30273342949029,-5.55091976686365));
#28751=CARTESIAN_POINT('Ctrl Pts',(49.8112860740297,-5.08844160785031,-4.7037203720868));
#28752=CARTESIAN_POINT('Ctrl Pts',(49.7782008066227,-5.87414978621033,-3.85652097730995));
#28753=CARTESIAN_POINT('Ctrl Pts',(49.7451155392157,-6.45264726098789,-2.81372984267439));
#28754=CARTESIAN_POINT('Ctrl Pts',(49.7120302718086,-6.73087574473247,-1.69757139387494));
#28755=CARTESIAN_POINT('Ctrl Pts',(49.6956507357412,-6.868618427251,-1.14499440109481));
#28756=CARTESIAN_POINT('Ctrl Pts',(49.6792711996737,-6.9327667757156,-0.574435469491616));
#28757=CARTESIAN_POINT('Ctrl Pts',(49.6628916636063,-6.92759240687057,-0.00323047333067872));
#28758=CARTESIAN_POINT('Ctrl Pts',(49.4835483363939,-6.93271820397492,-0.00595368521987888));
#28759=CARTESIAN_POINT('Ctrl Pts',(49.4985586286347,-6.93781416218575,-0.529188288697132));
#28760=CARTESIAN_POINT('Ctrl Pts',(49.5135689208755,-6.88397152104115,-1.05141926610295));
#28761=CARTESIAN_POINT('Ctrl Pts',(49.5285792131163,-6.76738092568683,-1.55910876840476));
#28762=CARTESIAN_POINT('Ctrl Pts',(49.5947497479304,-6.25340945030763,-3.79717884377907));
#28763=CARTESIAN_POINT('Ctrl Pts',(49.6609202827444,-4.52002569281411,-5.75265718265399));
#28764=CARTESIAN_POINT('Ctrl Pts',(49.7270908175585,-2.35978801703893,-6.53143669185472));
#28765=CARTESIAN_POINT('Ctrl Pts',(49.7932613523725,-0.199550341263754,
-7.31021620105544));
#28766=CARTESIAN_POINT('Ctrl Pts',(49.8594318871866,2.38754125279309,-6.91229688058191));
#28767=CARTESIAN_POINT('Ctrl Pts',(49.9256024220006,4.21092850274789,-5.52251801839842));
#28768=CARTESIAN_POINT('Ctrl Pts',(49.9917729568146,6.03431575270265,-4.13273915621496));
#28769=CARTESIAN_POINT('Ctrl Pts',(50.0579434916286,7.09399865855549,-1.75110075232157));
#28770=CARTESIAN_POINT('Ctrl Pts',(50.1241140264427,6.92037756701128,0.542965245975702));
#28771=CARTESIAN_POINT('Ctrl Pts',(50.1571992938497,6.83356702123917,1.68999824512437));
#28772=CARTESIAN_POINT('Ctrl Pts',(50.1902845612568,6.4384304761178,2.815138142874));
#28773=CARTESIAN_POINT('Ctrl Pts',(50.2233698286638,5.80617594701643,3.78226707248107));
#28774=CARTESIAN_POINT('Ctrl Pts',(50.2564550960708,5.17392141791508,4.74939600208811));
#28775=CARTESIAN_POINT('Ctrl Pts',(50.2895403634778,4.30454890483377,5.55851396355256));
#28776=CARTESIAN_POINT('Ctrl Pts',(50.3226256308848,3.29305560594214,6.10418901853135));
#28777=CARTESIAN_POINT('Ctrl Pts',(50.3557108982918,2.28156230705047,6.64986407351015));
#28778=CARTESIAN_POINT('Ctrl Pts',(50.3887961656989,1.1279482223485,6.93209622200326));
#28779=CARTESIAN_POINT('Ctrl Pts',(50.4218814331059,-0.0275070301753554,
6.92939150997962));
#28780=CARTESIAN_POINT('Ctrl Pts',(50.4549667005129,-1.18296228269921,6.92668679795597));
#28781=CARTESIAN_POINT('Ctrl Pts',(50.4880519679199,-2.34025870304492,6.63904522541559));
#28782=CARTESIAN_POINT('Ctrl Pts',(50.521137235327,-3.34653541563076,6.08170515893852));
#28783=CARTESIAN_POINT('Ctrl Pts',(50.587307770141,-5.35908884080245,4.96702502598438));
#28784=CARTESIAN_POINT('Ctrl Pts',(50.653478304955,-6.76756343493463,2.77355091728346));
#28785=CARTESIAN_POINT('Ctrl Pts',(50.719648839769,-6.92772948095231,0.486506276972989));
#28786=CARTESIAN_POINT('Ctrl Pts',(50.7242820053106,-6.93894407680581,0.326370705310355));
#28787=CARTESIAN_POINT('Ctrl Pts',(50.7289151708523,-6.94403871679269,0.165776394880989));
#28788=CARTESIAN_POINT('Ctrl Pts',(50.7335483363939,-6.94318480280473,0.00509973895979926));
#28789=CARTESIAN_POINT('Origin',(29.75,0.,0.));
#28790=CARTESIAN_POINT('',(52.1628916636063,-6.92485909669474,0.00398171681318865));
#28791=CARTESIAN_POINT('',(51.9835483363939,-6.92875907966107,0.000287925818791141));
#28792=CARTESIAN_POINT('',(29.75,-6.933,-8.4904762584886E-16));
#28793=CARTESIAN_POINT('Ctrl Pts',(52.1628916636063,-6.92485909669474,0.00398171681318865));
#28794=CARTESIAN_POINT('Ctrl Pts',(52.1399842841088,-6.93057837326804,0.804739728972275));
#28795=CARTESIAN_POINT('Ctrl Pts',(52.1170769046114,-6.80294244975768,1.60389401713382));
#28796=CARTESIAN_POINT('Ctrl Pts',(52.0941695251139,-6.53422410442902,2.35205869360553));
#28797=CARTESIAN_POINT('Ctrl Pts',(52.0279989902999,-5.7580010263276,4.51321627064897));
#28798=CARTESIAN_POINT('Ctrl Pts',(51.9618284554859,-3.80457490977705,6.24891243983584));
#28799=CARTESIAN_POINT('Ctrl Pts',(51.8956579206719,-1.56711450642194,6.76553152892132));
#28800=CARTESIAN_POINT('Ctrl Pts',(51.8294873858578,0.67034589693314,7.28215061800679));
#28801=CARTESIAN_POINT('Ctrl Pts',(51.7633168510438,3.19184058709277,6.5796926269909));
#28802=CARTESIAN_POINT('Ctrl Pts',(51.6971463162297,4.83720281076991,4.98313085181089));
#28803=CARTESIAN_POINT('Ctrl Pts',(51.6309757814157,6.48256503444705,3.38656907663088));
#28804=CARTESIAN_POINT('Ctrl Pts',(51.5648052466017,7.25179479164169,0.895903517286758));
#28805=CARTESIAN_POINT('Ctrl Pts',(51.4986347117877,6.80685910234047,-1.36128839310964));
#28806=CARTESIAN_POINT('Ctrl Pts',(51.4655494443806,6.58439125768985,-2.48988434830787));
#28807=CARTESIAN_POINT('Ctrl Pts',(51.4324641769736,6.05838205141525,-3.56011189126916));
#28808=CARTESIAN_POINT('Ctrl Pts',(51.3993789095666,5.31570653195091,-4.44527697691168));
#28809=CARTESIAN_POINT('Ctrl Pts',(51.3662936421595,4.57303101248661,-5.33044206255415));
#28810=CARTESIAN_POINT('Ctrl Pts',(51.3332083747525,3.6136891798326,-6.03054469087787));
#28811=CARTESIAN_POINT('Ctrl Pts',(51.3001231073455,2.54453117246911,-6.45218566922238));
#28812=CARTESIAN_POINT('Ctrl Pts',(51.2670378399385,1.47537316510556,-6.87382664756691));
#28813=CARTESIAN_POINT('Ctrl Pts',(51.2339525725315,0.296398983032527,-7.01700597593221));
#28814=CARTESIAN_POINT('Ctrl Pts',(51.2008673051245,-0.850551686782959,
-6.87704770693045));
#28815=CARTESIAN_POINT('Ctrl Pts',(51.1677820377175,-1.99750235659838,-6.73708943792869));
#28816=CARTESIAN_POINT('Ctrl Pts',(51.1346967703104,-3.11242951415625,-6.31399357155991));
#28817=CARTESIAN_POINT('Ctrl Pts',(51.1016115029034,-4.04536526565498,-5.64105103644369));
#28818=CARTESIAN_POINT('Ctrl Pts',(51.0387048898043,-5.81920096248678,-4.36155296941387));
#28819=CARTESIAN_POINT('Ctrl Pts',(50.9757982767053,-6.93511499268184,-2.17882798488593));
#28820=CARTESIAN_POINT('Ctrl Pts',(50.9128916636063,-6.94407271247953,0.00085298068625117));
#28821=CARTESIAN_POINT('Ctrl Pts',(50.7335483363939,-6.94318480280473,0.00509973895979926));
#28822=CARTESIAN_POINT('Ctrl Pts',(50.7950857056663,-6.93184317904203,-2.12899597163449));
#28823=CARTESIAN_POINT('Ctrl Pts',(50.8566230749388,-5.87111952376545,-4.27761821756149));
#28824=CARTESIAN_POINT('Ctrl Pts',(50.9181604442112,-4.16261867540694,-5.55885514366222));
#28825=CARTESIAN_POINT('Ctrl Pts',(50.9843309790252,-2.32548432594074,-6.93655675206683));
#28826=CARTESIAN_POINT('Ctrl Pts',(51.0505015138392,0.260641870894862,-7.31134479695605));
#28827=CARTESIAN_POINT('Ctrl Pts',(51.1166720486532,2.41330049815419,-6.51185422523226));
#28828=CARTESIAN_POINT('Ctrl Pts',(51.1828425834673,4.56595912541357,-5.71236365350845));
#28829=CARTESIAN_POINT('Ctrl Pts',(51.2490131182814,6.28515018309664,-3.73859446517156));
#28830=CARTESIAN_POINT('Ctrl Pts',(51.3151836530954,6.78082632587978,-1.50017280906083));
#28831=CARTESIAN_POINT('Ctrl Pts',(51.3813541879094,7.27650246866292,0.738248847049866));
#28832=CARTESIAN_POINT('Ctrl Pts',(51.4475247227234,6.54866369654615,3.24132297093438));
#28833=CARTESIAN_POINT('Ctrl Pts',(51.5136952575375,4.93534739297613,4.88147344958201));
#28834=CARTESIAN_POINT('Ctrl Pts',(51.5467805249445,4.12868924119113,5.70154868890581));
#28835=CARTESIAN_POINT('Ctrl Pts',(51.5798657923515,3.10066170654277,6.30589301692042));
#28836=CARTESIAN_POINT('Ctrl Pts',(51.6129510597585,1.99351089896141,6.63650040541012));
#28837=CARTESIAN_POINT('Ctrl Pts',(51.6460363271656,0.886360091380012,6.96710779389984));
#28838=CARTESIAN_POINT('Ctrl Pts',(51.6791215945726,-0.299913989134387,
7.02397824286466));
#28839=CARTESIAN_POINT('Ctrl Pts',(51.7122068619796,-1.42470120777253,6.78789844254885));
#28840=CARTESIAN_POINT('Ctrl Pts',(51.7452921293866,-2.54948842641068,6.55181864223305));
#28841=CARTESIAN_POINT('Ctrl Pts',(51.7783773967936,-3.61278878317257,6.02278859263659));
#28842=CARTESIAN_POINT('Ctrl Pts',(51.8114626642007,-4.49358304177177,5.27493457608602));
#28843=CARTESIAN_POINT('Ctrl Pts',(51.8445479316077,-5.37437730037094,4.52708055953547));
#28844=CARTESIAN_POINT('Ctrl Pts',(51.8776331990147,-6.07266546080745,3.56040257603086));
#28845=CARTESIAN_POINT('Ctrl Pts',(51.9107184664217,-6.48152754865665,2.48520372692769));
#28846=CARTESIAN_POINT('Ctrl Pts',(51.9349950897458,-6.78153391632782,1.69626655023685));
#28847=CARTESIAN_POINT('Ctrl Pts',(51.9592717130699,-6.92571249345945,0.848901442148907));
#28848=CARTESIAN_POINT('Ctrl Pts',(51.9835483363939,-6.92116679875715,0.000803383211501455));
#28849=CARTESIAN_POINT('Origin',(29.75,0.,0.));
#28850=CARTESIAN_POINT('',(53.4128916636063,-6.92692581532746,-0.0043983532947317));
#28851=CARTESIAN_POINT('',(53.2335483363939,-6.933,-5.95370974743048E-12));
#28852=CARTESIAN_POINT('',(29.75,-6.933,-8.4904762584886E-16));
#28853=CARTESIAN_POINT('Ctrl Pts',(53.4128916636063,-6.92692581532746,-0.0043983532947317));
#28854=CARTESIAN_POINT('Ctrl Pts',(53.3703408263264,-6.91775456656079,1.48198715944652));
#28855=CARTESIAN_POINT('Ctrl Pts',(53.3277899890465,-6.44830631727461,2.97362567138676));
#28856=CARTESIAN_POINT('Ctrl Pts',(53.2852391517666,-5.56377625673586,4.15603880035411));
#28857=CARTESIAN_POINT('Ctrl Pts',(53.2190686169526,-4.18824921880831,5.99480189214149));
#28858=CARTESIAN_POINT('Ctrl Pts',(53.1528980821386,-1.80892314934302,7.0857602583535));
#28859=CARTESIAN_POINT('Ctrl Pts',(53.0867275473245,0.478309390730293,6.92830024216106));
#28860=CARTESIAN_POINT('Ctrl Pts',(53.0205570125105,2.76554193080364,6.77084022596862));
#28861=CARTESIAN_POINT('Ctrl Pts',(52.9543864776965,4.96068094148503,5.36496182737171));
#28862=CARTESIAN_POINT('Ctrl Pts',(52.8882159428824,6.07774144758688,3.3537286450479));
#28863=CARTESIAN_POINT('Ctrl Pts',(52.8551306754754,6.6362717006378,2.34811205388602));
#28864=CARTESIAN_POINT('Ctrl Pts',(52.8220454080684,6.92528232754384,1.19115676679243));
#28865=CARTESIAN_POINT('Ctrl Pts',(52.7889601406614,6.92935411498852,0.0357055230789582));
#28866=CARTESIAN_POINT('Ctrl Pts',(52.7558748732543,6.9334259024332,-1.11974572063455));
#28867=CARTESIAN_POINT('Ctrl Pts',(52.7227896058473,6.65255885041648,-2.27369292096794));
#28868=CARTESIAN_POINT('Ctrl Pts',(52.6897043384403,6.10808092604286,-3.28583112753789));
#28869=CARTESIAN_POINT('Ctrl Pts',(52.6566190710333,5.56360300166923,-4.29796933410788));
#28870=CARTESIAN_POINT('Ctrl Pts',(52.6235338036263,4.75551420493866,-5.16829854691442));
#28871=CARTESIAN_POINT('Ctrl Pts',(52.5904485362193,3.78913400442954,-5.80169689244124));
#28872=CARTESIAN_POINT('Ctrl Pts',(52.5573632688123,2.82275380392046,-6.43509523796805));
#28873=CARTESIAN_POINT('Ctrl Pts',(52.5242780014052,1.69808219963283,-6.83156271621516));
#28874=CARTESIAN_POINT('Ctrl Pts',(52.4911927339982,0.551152713248234,-6.91973031374846));
#28875=CARTESIAN_POINT('Ctrl Pts',(52.4250221991841,-1.74270625952099,-7.09606550881507));
#28876=CARTESIAN_POINT('Ctrl Pts',(52.3588516643701,-4.12559676067808,-6.0392011810264));
#28877=CARTESIAN_POINT('Ctrl Pts',(52.2926811295561,-5.51753199143044,-4.21745952468206));
#28878=CARTESIAN_POINT('Ctrl Pts',(52.2494179742395,-6.42759732863707,-3.02638116258884));
#28879=CARTESIAN_POINT('Ctrl Pts',(52.2061548189229,-6.91405760145096,-1.50833959671446));
#28880=CARTESIAN_POINT('Ctrl Pts',(52.1628916636063,-6.92485909669474,0.00398171681318865));
#28881=CARTESIAN_POINT('Ctrl Pts',(51.9835483363939,-6.933,-5.90610893524968E-12));
#28882=CARTESIAN_POINT('Ctrl Pts',(52.040772531679,-6.9329999999983,-1.99420935702222));
#28883=CARTESIAN_POINT('Ctrl Pts',(52.0979967269641,-6.02307502628908,-3.97063309653564));
#28884=CARTESIAN_POINT('Ctrl Pts',(52.1552209222492,-4.50798484753529,-5.26731066241515));
#28885=CARTESIAN_POINT('Ctrl Pts',(52.2124451175343,-2.99289466878149,-6.56398822829465));
#28886=CARTESIAN_POINT('Ctrl Pts',(52.2696693128194,-0.899664345622527,
-7.1577904429249));
#28887=CARTESIAN_POINT('Ctrl Pts',(52.3268935081045,1.07062371682448,-6.84983604599212));
#28888=CARTESIAN_POINT('Ctrl Pts',(52.3841177033896,3.04091177927148,-6.54188164905934));
#28889=CARTESIAN_POINT('Ctrl Pts',(52.4413418986747,4.85311303640357,-5.33766370385969));
#28890=CARTESIAN_POINT('Ctrl Pts',(52.4985660939598,5.90026971494087,-3.64050907030207));
#28891=CARTESIAN_POINT('Ctrl Pts',(52.5557902892449,6.94742639347817,-1.94335443674444));
#28892=CARTESIAN_POINT('Ctrl Pts',(52.61301448453,7.21086008527491,0.216464293130433));
#28893=CARTESIAN_POINT('Ctrl Pts',(52.6702386798151,6.6023393500589,2.11556236179976));
#28894=CARTESIAN_POINT('Ctrl Pts',(52.7274628751002,5.99381861484289,4.01466043046909));
#28895=CARTESIAN_POINT('Ctrl Pts',(52.7846870703853,4.52419779646782,5.61916312790856));
#28896=CARTESIAN_POINT('Ctrl Pts',(52.8419112656704,2.68569472999816,6.39167683923868));
#28897=CARTESIAN_POINT('Ctrl Pts',(52.8991354609555,0.847191663528488,7.1641905505688));
#28898=CARTESIAN_POINT('Ctrl Pts',(52.9563596562406,-1.32739978994829,7.09093574623664));
#28899=CARTESIAN_POINT('Ctrl Pts',(53.0135838515257,-3.10974706736769,6.19644754492427));
#28900=CARTESIAN_POINT('Ctrl Pts',(53.0708080468108,-4.89209434478709,5.3019593436119));
#28901=CARTESIAN_POINT('Ctrl Pts',(53.1280322420959,-6.25040525058995,3.60219296582083));
#28902=CARTESIAN_POINT('Ctrl Pts',(53.1852564373809,-6.7297428071292,1.66644854402792));
#28903=CARTESIAN_POINT('Ctrl Pts',(53.2013537370519,-6.86458158035674,1.12191912096105));
#28904=CARTESIAN_POINT('Ctrl Pts',(53.2174510367229,-6.93300000000048,0.56097574577192));
#28905=CARTESIAN_POINT('Ctrl Pts',(53.2335483363939,-6.933,-5.95370974743048E-12));
#28906=CARTESIAN_POINT('Origin',(29.75,0.,0.));
#28907=CARTESIAN_POINT('',(54.6628916636063,-6.94327184494755,-0.00291245565295251));
#28908=CARTESIAN_POINT('',(54.483548336394,-6.93556957250402,-0.00097039555626976));
#28909=CARTESIAN_POINT('',(29.75,-6.933,-8.4904762584886E-16));
#28910=CARTESIAN_POINT('Ctrl Pts',(54.6628916636063,-6.94327184494755,-0.00291245565295251));
#28911=CARTESIAN_POINT('Ctrl Pts',(54.600697368544,-6.93190021454453,2.15659674677899));
#28912=CARTESIAN_POINT('Ctrl Pts',(54.5385030734816,-5.84407642554417,4.32603973215319));
#28913=CARTESIAN_POINT('Ctrl Pts',(54.4763087784193,-4.10653465994407,5.60058007758731));
#28914=CARTESIAN_POINT('Ctrl Pts',(54.4101382436052,-2.25790742208785,6.95660503477874));
#28915=CARTESIAN_POINT('Ctrl Pts',(54.3439677087913,0.32616968197601,7.29964274132155));
#28916=CARTESIAN_POINT('Ctrl Pts',(54.2777971739772,2.47753336573461,6.48446338180748));
#28917=CARTESIAN_POINT('Ctrl Pts',(54.2447119065702,3.55321520761379,6.07687370205049));
#28918=CARTESIAN_POINT('Ctrl Pts',(54.2116266391631,4.5207186944167,5.37972975577934));
#28919=CARTESIAN_POINT('Ctrl Pts',(54.1785413717561,5.26961429958365,4.49982093742742));
#28920=CARTESIAN_POINT('Ctrl Pts',(54.1454561043491,6.01850990475068,3.6199121190754));
#28921=CARTESIAN_POINT('Ctrl Pts',(54.1123708369421,6.54879762828172,2.55723842864254));
#28922=CARTESIAN_POINT('Ctrl Pts',(54.0792855695351,6.78620805577826,1.43273131517245));
#28923=CARTESIAN_POINT('Ctrl Pts',(54.0462003021281,7.02361848327481,0.308224201702331));
#28924=CARTESIAN_POINT('Ctrl Pts',(54.013115034721,6.96815161473686,-0.878116334804946));
#28925=CARTESIAN_POINT('Ctrl Pts',(53.980029767314,6.63885438353871,-1.98565752572177));
#28926=CARTESIAN_POINT('Ctrl Pts',(53.946944499907,6.3095571523406,-3.0931987166385));
#28927=CARTESIAN_POINT('Ctrl Pts',(53.9138592325,5.70642955848233,-4.12194056196472));
#28928=CARTESIAN_POINT('Ctrl Pts',(53.880773965093,4.8873092910417,-4.92956842147746));
#28929=CARTESIAN_POINT('Ctrl Pts',(53.814603430279,3.24906875616034,-6.54482414050303));
#28930=CARTESIAN_POINT('Ctrl Pts',(53.7484328954649,0.746857526949387,-7.27562391627462));
#28931=CARTESIAN_POINT('Ctrl Pts',(53.6822623606508,-1.49214902185302,-6.78259650984583));
#28932=CARTESIAN_POINT('Ctrl Pts',(53.6160918258368,-3.73115557065537,-6.28956910341706));
#28933=CARTESIAN_POINT('Ctrl Pts',(53.5499212910228,-5.70695743904921,-4.57271451478797));
#28934=CARTESIAN_POINT('Ctrl Pts',(53.4837507562088,-6.50899437005123,-2.42100331179203));
#28935=CARTESIAN_POINT('Ctrl Pts',(53.4601310586746,-6.79528296927026,-1.65294592887326));
#28936=CARTESIAN_POINT('Ctrl Pts',(53.4365113611405,-6.93201671684027,-0.829481441534794));
#28937=CARTESIAN_POINT('Ctrl Pts',(53.4128916636063,-6.92692581532746,-0.0043983532947317));
#28938=CARTESIAN_POINT('Ctrl Pts',(53.2335483363939,-6.9329724241112,-0.00157606328284038));
#28939=CARTESIAN_POINT('Ctrl Pts',(53.2557987901015,-6.93641591712985,-0.778738933088749));
#28940=CARTESIAN_POINT('Ctrl Pts',(53.278049243809,-6.81138105671096,-1.55551720174311));
#28941=CARTESIAN_POINT('Ctrl Pts',(53.3002996975165,-6.55468300132901,-2.28529378426906));
#28942=CARTESIAN_POINT('Ctrl Pts',(53.3664702323305,-5.79128968658476,-4.45557342868741));
#28943=CARTESIAN_POINT('Ctrl Pts',(53.4326407671446,-3.863459532006,-6.21016746804625));
#28944=CARTESIAN_POINT('Ctrl Pts',(53.4988113019586,-1.63516466953287,-6.74954521596095));
#28945=CARTESIAN_POINT('Ctrl Pts',(53.5649818367726,0.593130192940265,-7.28892296387565));
#28946=CARTESIAN_POINT('Ctrl Pts',(53.6311523715867,3.1218897633078,-6.6130844203462));
#28947=CARTESIAN_POINT('Ctrl Pts',(53.6973229064007,4.78670810869231,-5.03146998671818));
#28948=CARTESIAN_POINT('Ctrl Pts',(53.7634934412148,6.45152645407682,-3.44985555309015));
#28949=CARTESIAN_POINT('Ctrl Pts',(53.8296639760288,7.25240357447835,-0.962465229363512));
#28950=CARTESIAN_POINT('Ctrl Pts',(53.8958345108428,6.82315289555494,1.29338675922819));
#28951=CARTESIAN_POINT('Ctrl Pts',(53.9620050456569,6.39390221663153,3.5492387478199));
#28952=CARTESIAN_POINT('Ctrl Pts',(54.0281755804709,4.73452373838319,5.57355240127669));
#28953=CARTESIAN_POINT('Ctrl Pts',(54.094346115285,2.61013036397045,6.43563078508));
#28954=CARTESIAN_POINT('Ctrl Pts',(54.160516650099,0.485736989557669,7.29770916888332));
#28955=CARTESIAN_POINT('Ctrl Pts',(54.226687184913,-2.10367128101945,6.99755228303315));
#28956=CARTESIAN_POINT('Ctrl Pts',(54.2928577197271,-3.98993172841131,5.6803945048691));
#28957=CARTESIAN_POINT('Ctrl Pts',(54.3259429871341,-4.93306195210724,5.02181561578707));
#28958=CARTESIAN_POINT('Ctrl Pts',(54.3590282545411,-5.70040522000687,4.10898650362653));
#28959=CARTESIAN_POINT('Ctrl Pts',(54.3921135219481,-6.21104285301366,3.07248596633321));
#28960=CARTESIAN_POINT('Ctrl Pts',(54.4225917934301,-6.68144414118274,2.11765781342223));
#28961=CARTESIAN_POINT('Ctrl Pts',(54.453070064912,-6.93400084389427,1.05788007359531));
#28962=CARTESIAN_POINT('Ctrl Pts',(54.483548336394,-6.93556957250402,-0.00097039555626976));
#28963=CARTESIAN_POINT('Origin',(29.75,0.,0.));
#28964=CARTESIAN_POINT('',(55.9128916636063,-6.93279366535694,0.00322938497813596));
#28965=CARTESIAN_POINT('',(55.7335483363939,-6.93303840625552,3.40981942736484E-5));
#28966=CARTESIAN_POINT('',(29.75,-6.933,-8.4904762584886E-16));
#28967=CARTESIAN_POINT('Ctrl Pts',(55.9128916636063,-6.93241833981259,0.00910368052880667));
#28968=CARTESIAN_POINT('Ctrl Pts',(55.8972244455755,-6.9374986604769,0.554924718265877));
#28969=CARTESIAN_POINT('Ctrl Pts',(55.8815572275448,-6.87855946148903,1.09943300383134));
#28970=CARTESIAN_POINT('Ctrl Pts',(55.8658900095141,-6.75147513749155,1.6271777980981));
#28971=CARTESIAN_POINT('Ctrl Pts',(55.7997194747001,-6.21473417499926,3.85610926592132));
#28972=CARTESIAN_POINT('Ctrl Pts',(55.7335489398861,-4.46242227668877,5.78601401976182));
#28973=CARTESIAN_POINT('Ctrl Pts',(55.667378405072,-2.29304736038406,6.55197456736258));
#28974=CARTESIAN_POINT('Ctrl Pts',(55.634293137665,-1.20835990223168,6.93495484116297));
#28975=CARTESIAN_POINT('Ctrl Pts',(55.6012078702579,-0.0194066895807528,
7.02694906340341));
#28976=CARTESIAN_POINT('Ctrl Pts',(55.5681226028509,1.12053871685304,6.83824658222559));
#28977=CARTESIAN_POINT('Ctrl Pts',(55.5350373354439,2.26048412328677,6.64954410104778));
#28978=CARTESIAN_POINT('Ctrl Pts',(55.5019520680369,3.35142172350335,6.18014491645175));
#28979=CARTESIAN_POINT('Ctrl Pts',(55.4688668006299,4.25856916975443,5.47447964871574));
#28980=CARTESIAN_POINT('Ctrl Pts',(55.4357815332229,5.16571661600551,4.76881438097973));
#28981=CARTESIAN_POINT('Ctrl Pts',(55.4026962658158,5.88907390829107,3.82688303010377));
#28982=CARTESIAN_POINT('Ctrl Pts',(55.3696109984088,6.35241778199036,2.76839514129382));
#28983=CARTESIAN_POINT('Ctrl Pts',(55.3365257310018,6.81576165568967,1.70990725248383));
#28984=CARTESIAN_POINT('Ctrl Pts',(55.3034404635948,7.0190921108027,0.534862825739778));
#28985=CARTESIAN_POINT('Ctrl Pts',(55.2703551961878,6.91472880905904,-0.610706497017424));
#28986=CARTESIAN_POINT('Ctrl Pts',(55.2041846613738,6.70600220557173,-2.90184514253183));
#28987=CARTESIAN_POINT('Ctrl Pts',(55.1380141265597,5.26650057465781,-5.07508337209913));
#28988=CARTESIAN_POINT('Ctrl Pts',(55.0718435917456,3.23811664294813,-6.14367355296912));
#28989=CARTESIAN_POINT('Ctrl Pts',(55.0056730569316,1.20973271123846,-7.21226373383911));
#28990=CARTESIAN_POINT('Ctrl Pts',(54.9395025221176,-1.40753352126693,-7.17620586601176));
#28991=CARTESIAN_POINT('Ctrl Pts',(54.8733319873035,-3.40895278540716,-6.05039714828136));
#28992=CARTESIAN_POINT('Ctrl Pts',(54.8071614524895,-5.4103720495474,-4.92458843055096));
#28993=CARTESIAN_POINT('Ctrl Pts',(54.7409909176755,-6.79594434532244,-2.70902886291751));
#28994=CARTESIAN_POINT('Ctrl Pts',(54.6748203828614,-6.93214180738565,-0.416742975180784));
#28995=CARTESIAN_POINT('Ctrl Pts',(54.6708441431097,-6.94032602055938,-0.278997703894782));
#28996=CARTESIAN_POINT('Ctrl Pts',(54.666867903358,-6.94399886225364,-0.140975381300478));
#28997=CARTESIAN_POINT('Ctrl Pts',(54.6628916636063,-6.94327184494755,-0.00291245565295251));
#28998=CARTESIAN_POINT('Ctrl Pts',(54.483548336394,-6.93556957250402,-0.00097039555626976));
#28999=CARTESIAN_POINT('Ctrl Pts',(54.486155332319,-6.93570375560872,-0.0915404549499743));
#29000=CARTESIAN_POINT('Ctrl Pts',(54.4887623282441,-6.93400159931765,-0.182103730019941));
#29001=CARTESIAN_POINT('Ctrl Pts',(54.4913693241692,-6.93044236180577,-0.272593960816664));
#29002=CARTESIAN_POINT('Ctrl Pts',(54.5244545915762,-6.88527223947709,-1.42100138824727));
#29003=CARTESIAN_POINT('Ctrl Pts',(54.5575398589832,-6.54099999670573,-2.55764428068227));
#29004=CARTESIAN_POINT('Ctrl Pts',(54.5906251263902,-5.95052884467048,-3.55083508544557));
#29005=CARTESIAN_POINT('Ctrl Pts',(54.6237103937972,-5.36005769263525,-4.54402589020884));
#29006=CARTESIAN_POINT('Ctrl Pts',(54.6567956612043,-4.52338763133613,-5.39376460730039));
#29007=CARTESIAN_POINT('Ctrl Pts',(54.6898809286113,-3.53144355466652,-5.97623153404674));
#29008=CARTESIAN_POINT('Ctrl Pts',(54.7560514634254,-1.54755540132733,-7.14116538753941));
#29009=CARTESIAN_POINT('Ctrl Pts',(54.8222219982394,1.05742881349393,-7.23701207965144));
#29010=CARTESIAN_POINT('Ctrl Pts',(54.8883925330534,3.10754793880998,-6.21073827550217));
#29011=CARTESIAN_POINT('Ctrl Pts',(54.9545630678674,5.15766706412604,-5.1844644713529));
#29012=CARTESIAN_POINT('Ctrl Pts',(55.0207336026815,6.65292109993693,-3.03607017094233));
#29013=CARTESIAN_POINT('Ctrl Pts',(55.0869041374955,6.90366166557409,-0.753472197462701));
#29014=CARTESIAN_POINT('Ctrl Pts',(55.1530746723096,7.15440223121126,1.52912577601692));
#29015=CARTESIAN_POINT('Ctrl Pts',(55.2192452071236,6.16062932667472,3.94592742256563));
#29016=CARTESIAN_POINT('Ctrl Pts',(55.2854157419376,4.37672763385377,5.39189391254384));
#29017=CARTESIAN_POINT('Ctrl Pts',(55.3515862767517,2.59282594103279,6.83786040252208));
#29018=CARTESIAN_POINT('Ctrl Pts',(55.4177568115657,0.0187954599274759,
7.31299173592979));
#29019=CARTESIAN_POINT('Ctrl Pts',(55.4839273463797,-2.16025041450548,6.60026077253155));
#29020=CARTESIAN_POINT('Ctrl Pts',(55.5500978811938,-4.3392962889384,5.88752980913332));
#29021=CARTESIAN_POINT('Ctrl Pts',(55.6162684160078,-6.1233575566989,3.98693654892914));
#29022=CARTESIAN_POINT('Ctrl Pts',(55.6824389508218,-6.71392967766051,1.76340160251706));
#29023=CARTESIAN_POINT('Ctrl Pts',(55.6994754126792,-6.86598012490355,1.19092371021159));
#29024=CARTESIAN_POINT('Ctrl Pts',(55.7165118745365,-6.93891754636801,0.597038925338642));
#29025=CARTESIAN_POINT('Ctrl Pts',(55.7335483363939,-6.93581065002168,0.00249537752124046));
#29026=CARTESIAN_POINT('Origin',(29.75,0.,0.));
#29027=CARTESIAN_POINT('',(57.1628916636063,-6.933,-6.1478599988618E-13));
#29028=CARTESIAN_POINT('',(56.9835483363939,-6.92793287508387,0.000631348358467133));
#29029=CARTESIAN_POINT('',(29.75,-6.933,-8.4904762584886E-16));
#29030=CARTESIAN_POINT('Ctrl Pts',(57.1628916636063,-6.933,-6.1478599988618E-13));
#29031=CARTESIAN_POINT('Ctrl Pts',(57.1056674683212,-6.93300000000018,1.99420935701573));
#29032=CARTESIAN_POINT('Ctrl Pts',(57.0484432730361,-6.02307502629278,3.97063309653004));
#29033=CARTESIAN_POINT('Ctrl Pts',(56.991219077751,-4.50798484754016,5.26731066241097));
#29034=CARTESIAN_POINT('Ctrl Pts',(56.9339948824659,-2.99289466878755,6.5639882282919));
#29035=CARTESIAN_POINT('Ctrl Pts',(56.8767706871808,-0.899664345629088,
7.15779044292408));
#29036=CARTESIAN_POINT('Ctrl Pts',(56.8195464918957,1.07062371681823,6.8498360459931));
#29037=CARTESIAN_POINT('Ctrl Pts',(56.7623222966106,3.04091177926555,6.54188164906211));
#29038=CARTESIAN_POINT('Ctrl Pts',(56.7050981013255,4.85311303639876,5.33766370386408));
#29039=CARTESIAN_POINT('Ctrl Pts',(56.6478739060404,5.9002697149376,3.64050907030736));
#29040=CARTESIAN_POINT('Ctrl Pts',(56.5906497107553,6.94742639347645,1.94335443675065));
#29041=CARTESIAN_POINT('Ctrl Pts',(56.5334255154702,7.21086008527512,-0.216464293124029));
#29042=CARTESIAN_POINT('Ctrl Pts',(56.4762013201851,6.60233935006077,-2.11556236179393));
#29043=CARTESIAN_POINT('Ctrl Pts',(56.4189771249,5.99381861484643,-4.01466043046382));
#29044=CARTESIAN_POINT('Ctrl Pts',(56.3617529296149,4.52419779647274,-5.61916312790461));
#29045=CARTESIAN_POINT('Ctrl Pts',(56.3045287343298,2.68569473000371,-6.39167683923634));
#29046=CARTESIAN_POINT('Ctrl Pts',(56.2473045390448,0.847191663534686,-7.16419055056807));
#29047=CARTESIAN_POINT('Ctrl Pts',(56.1900803437596,-1.32739978994219,-7.0909357462378));
#29048=CARTESIAN_POINT('Ctrl Pts',(56.1328561484746,-3.10974706736239,-6.19644754492693));
#29049=CARTESIAN_POINT('Ctrl Pts',(56.0756319531895,-4.89209434478259,-5.30195934361607));
#29050=CARTESIAN_POINT('Ctrl Pts',(56.0184077579044,-6.25040525058691,-3.60219296582612));
#29051=CARTESIAN_POINT('Ctrl Pts',(55.9611835626193,-6.7297428071278,-1.66644854403358));
#29052=CARTESIAN_POINT('Ctrl Pts',(55.9450862629483,-6.86458158035573,-1.12191912096708));
#29053=CARTESIAN_POINT('Ctrl Pts',(55.9289889632773,-6.93299999999995,-0.560975745778276));
#29054=CARTESIAN_POINT('Ctrl Pts',(55.9128916636063,-6.933,-6.65856259018938E-13));
#29055=CARTESIAN_POINT('Ctrl Pts',(55.7335483363939,-6.933,-5.85170800704304E-12));
#29056=CARTESIAN_POINT('Ctrl Pts',(55.790772531679,-6.93299999999832,-1.99420935702216));
#29057=CARTESIAN_POINT('Ctrl Pts',(55.8479967269641,-6.02307502628911,-3.97063309653559));
#29058=CARTESIAN_POINT('Ctrl Pts',(55.9052209222492,-4.50798484753533,-5.26731066241511));
#29059=CARTESIAN_POINT('Ctrl Pts',(55.9624451175343,-2.99289466878154,-6.56398822829463));
#29060=CARTESIAN_POINT('Ctrl Pts',(56.0196693128194,-0.899664345622583,
-7.15779044292489));
#29061=CARTESIAN_POINT('Ctrl Pts',(56.0768935081045,1.07062371682442,-6.84983604599213));
#29062=CARTESIAN_POINT('Ctrl Pts',(56.1341177033896,3.04091177927143,-6.54188164905936));
#29063=CARTESIAN_POINT('Ctrl Pts',(56.1913418986747,4.85311303640352,-5.33766370385973));
#29064=CARTESIAN_POINT('Ctrl Pts',(56.2485660939598,5.90026971494084,-3.64050907030211));
#29065=CARTESIAN_POINT('Ctrl Pts',(56.3057902892449,6.94742639347816,-1.94335443674449));
#29066=CARTESIAN_POINT('Ctrl Pts',(56.36301448453,7.21086008527492,0.216464293130376));
#29067=CARTESIAN_POINT('Ctrl Pts',(56.4202386798151,6.60233935005892,2.11556236179971));
#29068=CARTESIAN_POINT('Ctrl Pts',(56.4774628751002,5.99381861484291,4.01466043046907));
#29069=CARTESIAN_POINT('Ctrl Pts',(56.5346870703853,4.52419779646782,5.61916312790858));
#29070=CARTESIAN_POINT('Ctrl Pts',(56.5919112656704,2.68569472999811,6.3916768392387));
#29071=CARTESIAN_POINT('Ctrl Pts',(56.6491354609555,0.847191663528411,7.16419055056882));
#29072=CARTESIAN_POINT('Ctrl Pts',(56.7063596562406,-1.3273997899484,7.09093574623663));
#29073=CARTESIAN_POINT('Ctrl Pts',(56.7635838515257,-3.10974706736782,6.19644754492421));
#29074=CARTESIAN_POINT('Ctrl Pts',(56.8208080468108,-4.89209434478723,5.30195934361179));
#29075=CARTESIAN_POINT('Ctrl Pts',(56.8780322420959,-6.25040525059006,3.60219296582064));
#29076=CARTESIAN_POINT('Ctrl Pts',(56.935256437381,-6.72974280712926,1.66644854402768));
#29077=CARTESIAN_POINT('Ctrl Pts',(56.951353737052,-6.86458158035676,1.12191912096091));
#29078=CARTESIAN_POINT('Ctrl Pts',(56.9674510367229,-6.93300000000048,0.560975745771875));
#29079=CARTESIAN_POINT('Ctrl Pts',(56.9835483363939,-6.933,-5.89944759710193E-12));
#29080=CARTESIAN_POINT('Origin',(29.75,0.,0.));
#29081=CARTESIAN_POINT('',(58.4128916636063,-6.933,-4.64905891561784E-13));
#29082=CARTESIAN_POINT('',(58.2335483363939,-6.93876249354147,-0.00788840371280948));
#29083=CARTESIAN_POINT('',(29.75,-6.933,-8.4904762584886E-16));
#29084=CARTESIAN_POINT('Ctrl Pts',(58.4128916636063,-6.933,-4.64905891561784E-13));
#29085=CARTESIAN_POINT('Ctrl Pts',(58.3556674683212,-6.93300000000013,1.99420935701588));
#29086=CARTESIAN_POINT('Ctrl Pts',(58.2984432730361,-6.0230750262927,3.97063309653017));
#29087=CARTESIAN_POINT('Ctrl Pts',(58.241219077751,-4.50798484754005,5.26731066241107));
#29088=CARTESIAN_POINT('Ctrl Pts',(58.1839948824659,-2.9928946687874,6.56398822829196));
#29089=CARTESIAN_POINT('Ctrl Pts',(58.1267706871808,-0.899664345628934,
7.1577904429241));
#29090=CARTESIAN_POINT('Ctrl Pts',(58.0695464918957,1.07062371681838,6.84983604599307));
#29091=CARTESIAN_POINT('Ctrl Pts',(58.0123222966106,3.04091177926569,6.54188164906204));
#29092=CARTESIAN_POINT('Ctrl Pts',(57.9550981013255,4.85311303639887,5.33766370386397));
#29093=CARTESIAN_POINT('Ctrl Pts',(57.8978739060404,5.90026971493768,3.64050907030724));
#29094=CARTESIAN_POINT('Ctrl Pts',(57.8406497107553,6.94742639347649,1.9433544367505));
#29095=CARTESIAN_POINT('Ctrl Pts',(57.7834255154702,7.21086008527511,-0.216464293124184));
#29096=CARTESIAN_POINT('Ctrl Pts',(57.7262013201851,6.60233935006073,-2.11556236179407));
#29097=CARTESIAN_POINT('Ctrl Pts',(57.6689771249,5.99381861484634,-4.01466043046395));
#29098=CARTESIAN_POINT('Ctrl Pts',(57.6117529296149,4.52419779647262,-5.61916312790471));
#29099=CARTESIAN_POINT('Ctrl Pts',(57.5545287343298,2.68569473000357,-6.3916768392364));
#29100=CARTESIAN_POINT('Ctrl Pts',(57.4973045390447,0.847191663534532,-7.16419055056809));
#29101=CARTESIAN_POINT('Ctrl Pts',(57.4400803437596,-1.32739978994234,-7.09093574623777));
#29102=CARTESIAN_POINT('Ctrl Pts',(57.3828561484745,-3.10974706736252,-6.19644754492687));
#29103=CARTESIAN_POINT('Ctrl Pts',(57.3256319531895,-4.8920943447827,-5.30195934361597));
#29104=CARTESIAN_POINT('Ctrl Pts',(57.2684077579043,-6.25040525058699,-3.60219296582598));
#29105=CARTESIAN_POINT('Ctrl Pts',(57.2111835626193,-6.72974280712784,-1.66644854403343));
#29106=CARTESIAN_POINT('Ctrl Pts',(57.1950862629483,-6.86458158035575,-1.12191912096696));
#29107=CARTESIAN_POINT('Ctrl Pts',(57.1789889632773,-6.93299999999995,-0.560975745778193));
#29108=CARTESIAN_POINT('Ctrl Pts',(57.1628916636063,-6.933,-6.1478599988618E-13));
#29109=CARTESIAN_POINT('Ctrl Pts',(56.9835483363939,-6.91923797360895,0.00171470667456418));
#29110=CARTESIAN_POINT('Ctrl Pts',(57.0130389515682,-6.92101525208908,-1.02900630106465));
#29111=CARTESIAN_POINT('Ctrl Pts',(57.0425295667424,-6.70489479915974,-2.0598170771908));
#29112=CARTESIAN_POINT('Ctrl Pts',(57.0720201819166,-6.26630550510988,-2.98661216848789));
#29113=CARTESIAN_POINT('Ctrl Pts',(57.1051054493236,-5.77425595003048,-4.02637560665029));
#29114=CARTESIAN_POINT('Ctrl Pts',(57.1381907167306,-5.00219814537272,-4.93522071175101));
#29115=CARTESIAN_POINT('Ctrl Pts',(57.1712759841377,-4.06538541530075,-5.61158308860758));
#29116=CARTESIAN_POINT('Ctrl Pts',(57.2043612515447,-3.12857268522872,-6.2879454654642));
#29117=CARTESIAN_POINT('Ctrl Pts',(57.2374465189517,-2.02700502974241,-6.73182511407668));
#29118=CARTESIAN_POINT('Ctrl Pts',(57.2705317863588,-0.88714999921381,-6.87883010959571));
#29119=CARTESIAN_POINT('Ctrl Pts',(57.3036170537658,0.252705031314849,-7.02583510511475));
#29120=CARTESIAN_POINT('Ctrl Pts',(57.3367023211728,1.43084743688566,-6.87596544754036));
#29121=CARTESIAN_POINT('Ctrl Pts',(57.3697875885798,2.50861057196623,-6.45941919475009));
#29122=CARTESIAN_POINT('Ctrl Pts',(57.4028728559868,3.58637370704667,-6.04287294195987));
#29123=CARTESIAN_POINT('Ctrl Pts',(57.4359581233938,4.56375757163673,-5.35965009395384));
#29124=CARTESIAN_POINT('Ctrl Pts',(57.4690433908008,5.3035115407242,-4.47875007850801));
#29125=CARTESIAN_POINT('Ctrl Pts',(57.5352139256149,6.7830194788992,-2.71695004761632));
#29126=CARTESIAN_POINT('Ctrl Pts',(57.6013844604289,7.31200783506392,-0.164441346965323));
#29127=CARTESIAN_POINT('Ctrl Pts',(57.667554995243,6.64204806609351,2.02813254164841));
#29128=CARTESIAN_POINT('Ctrl Pts',(57.733725530057,5.97208829712309,4.2207064302622));
#29129=CARTESIAN_POINT('Ctrl Pts',(57.799896064871,4.10318040301745,6.0533455068388));
#29130=CARTESIAN_POINT('Ctrl Pts',(57.8660665996851,1.89437680725851,6.6812873951947));
#29131=CARTESIAN_POINT('Ctrl Pts',(57.9322371344991,-0.31442678850043,7.3092292835506));
#29132=CARTESIAN_POINT('Ctrl Pts',(57.9984076693131,-2.86312608591256,6.73247398368588));
#29133=CARTESIAN_POINT('Ctrl Pts',(58.0645782041272,-4.58637444068998,5.21473242217204));
#29134=CARTESIAN_POINT('Ctrl Pts',(58.1209015815494,-6.0531778714189,3.92285332464293));
#29135=CARTESIAN_POINT('Ctrl Pts',(58.1772249589717,-6.92192873783322,1.94921445473074));
#29136=CARTESIAN_POINT('Ctrl Pts',(58.2335483363939,-6.93876249354147,-0.00788840371280948));
#29137=CARTESIAN_POINT('Origin',(29.75,0.,0.));
#29138=CARTESIAN_POINT('',(59.6628916636063,-6.933,-3.15580894749701E-13));
#29139=CARTESIAN_POINT('',(59.483548336394,-6.93838776086578,0.00532365672661986));
#29140=CARTESIAN_POINT('',(29.75,-6.933,-8.4904762584886E-16));
#29141=CARTESIAN_POINT('Ctrl Pts',(59.6628916636063,-6.933,-1.18793863634892E-13));
#29142=CARTESIAN_POINT('Ctrl Pts',(59.6056674683212,-6.93300000000003,1.99420935701622));
#29143=CARTESIAN_POINT('Ctrl Pts',(59.5484432730361,-6.0230750262925,3.97063309653047));
#29144=CARTESIAN_POINT('Ctrl Pts',(59.491219077751,-4.50798484753979,5.26731066241129));
#29145=CARTESIAN_POINT('Ctrl Pts',(59.4339948824659,-2.99289466878708,6.56398822829211));
#29146=CARTESIAN_POINT('Ctrl Pts',(59.3767706871808,-0.899664345628577,
7.15779044292415));
#29147=CARTESIAN_POINT('Ctrl Pts',(59.3195464918957,1.07062371681872,6.84983604599302));
#29148=CARTESIAN_POINT('Ctrl Pts',(59.2623222966106,3.04091177926602,6.54188164906189));
#29149=CARTESIAN_POINT('Ctrl Pts',(59.2050981013255,4.85311303639914,5.33766370386373));
#29150=CARTESIAN_POINT('Ctrl Pts',(59.1478739060404,5.90026971493786,3.64050907030694));
#29151=CARTESIAN_POINT('Ctrl Pts',(59.0906497107553,6.94742639347658,1.94335443675015));
#29152=CARTESIAN_POINT('Ctrl Pts',(59.0334255154702,7.2108600852751,-0.216464293124544));
#29153=CARTESIAN_POINT('Ctrl Pts',(58.9762013201851,6.60233935006062,-2.1155623617944));
#29154=CARTESIAN_POINT('Ctrl Pts',(58.9189771249,5.99381861484614,-4.01466043046425));
#29155=CARTESIAN_POINT('Ctrl Pts',(58.8617529296149,4.52419779647234,-5.61916312790494));
#29156=CARTESIAN_POINT('Ctrl Pts',(58.8045287343298,2.68569473000325,-6.39167683923653));
#29157=CARTESIAN_POINT('Ctrl Pts',(58.7473045390447,0.847191663534174,-7.16419055056813));
#29158=CARTESIAN_POINT('Ctrl Pts',(58.6900803437596,-1.3273997899427,-7.0909357462377));
#29159=CARTESIAN_POINT('Ctrl Pts',(58.6328561484745,-3.10974706736283,-6.19644754492671));
#29160=CARTESIAN_POINT('Ctrl Pts',(58.5756319531895,-4.89209434478297,-5.30195934361572));
#29161=CARTESIAN_POINT('Ctrl Pts',(58.5184077579043,-6.25040525058717,-3.60219296582567));
#29162=CARTESIAN_POINT('Ctrl Pts',(58.4611835626192,-6.72974280712792,-1.66644854403309));
#29163=CARTESIAN_POINT('Ctrl Pts',(58.4450862629483,-6.86458158035579,-1.12191912096668));
#29164=CARTESIAN_POINT('Ctrl Pts',(58.4289889632773,-6.93299999999996,-0.560975745777977));
#29165=CARTESIAN_POINT('Ctrl Pts',(58.4128916636063,-6.933,-4.64905891561784E-13));
#29166=CARTESIAN_POINT('Ctrl Pts',(58.2335483363939,-6.93876249354147,-0.00788840371280948));
#29167=CARTESIAN_POINT('Ctrl Pts',(58.2433954937857,-6.94170558128835,-0.350053606884688));
#29168=CARTESIAN_POINT('Ctrl Pts',(58.2532426511775,-6.9186086245689,-0.691713363612853));
#29169=CARTESIAN_POINT('Ctrl Pts',(58.2630898085693,-6.86811497086886,-1.02913598018768));
#29170=CARTESIAN_POINT('Ctrl Pts',(58.3292603433833,-6.52880973412778,-3.2965349978707));
#29171=CARTESIAN_POINT('Ctrl Pts',(58.3954308781973,-4.95240184850311,-5.37260521007374));
#29172=CARTESIAN_POINT('Ctrl Pts',(58.4616014130114,-2.85851431917938,-6.32576736968542));
#29173=CARTESIAN_POINT('Ctrl Pts',(58.4946866804184,-1.81157055451755,-6.80234844949124));
#29174=CARTESIAN_POINT('Ctrl Pts',(58.5277719478254,-0.635256878931015,
-6.99820251614922));
#29175=CARTESIAN_POINT('Ctrl Pts',(58.5608572152324,0.516841190274217,-6.91014460914694));
#29176=CARTESIAN_POINT('Ctrl Pts',(58.5939424826395,1.66893925947945,-6.82208670214467));
#29177=CARTESIAN_POINT('Ctrl Pts',(58.6270277500465,2.79682172230348,-6.45011682148206));
#29178=CARTESIAN_POINT('Ctrl Pts',(58.6601130174535,3.76233056023795,-5.82668066340393));
#29179=CARTESIAN_POINT('Ctrl Pts',(58.6931982848605,4.72783939817248,-5.20324450532576));
#29180=CARTESIAN_POINT('Ctrl Pts',(58.7262835522675,5.53097461121756,-4.32834206983201));
#29181=CARTESIAN_POINT('Ctrl Pts',(58.7593688196746,6.08531354531465,-3.31454105276985));
#29182=CARTESIAN_POINT('Ctrl Pts',(58.7924540870816,6.63965247941167,-2.30074003570779));
#29183=CARTESIAN_POINT('Ctrl Pts',(58.8255393544886,6.94519513456072,-1.14804043707739));
#29184=CARTESIAN_POINT('Ctrl Pts',(58.8586246218956,6.94164474653778,0.00226742029728548));
#29185=CARTESIAN_POINT('Ctrl Pts',(58.9247951567097,6.9345439704919,2.30288313504689));
#29186=CARTESIAN_POINT('Ctrl Pts',(58.9909656915237,5.69107102175774,4.5939318847734));
#29187=CARTESIAN_POINT('Ctrl Pts',(59.0571362263377,3.76415786551684,5.83620079180433));
#29188=CARTESIAN_POINT('Ctrl Pts',(59.1233067611518,1.83724470927605,7.07846969883519));
#29189=CARTESIAN_POINT('Ctrl Pts',(59.1894772959658,-0.773108654471531,
7.27195876317054));
#29190=CARTESIAN_POINT('Ctrl Pts',(59.2556478307798,-2.86550398523472,6.32591113245124));
#29191=CARTESIAN_POINT('Ctrl Pts',(59.3218183655939,-4.95789931599796,5.37986350173191));
#29192=CARTESIAN_POINT('Ctrl Pts',(59.3879889004079,-6.53233661377687,3.29427917595797));
#29193=CARTESIAN_POINT('Ctrl Pts',(59.454159435222,-6.86893290788461,1.02275385701864));
#29194=CARTESIAN_POINT('Ctrl Pts',(59.4639557356126,-6.91876473131977,0.686463022557893));
#29195=CARTESIAN_POINT('Ctrl Pts',(59.4737520360033,-6.94146593200598,0.34609678994491));
#29196=CARTESIAN_POINT('Ctrl Pts',(59.483548336394,-6.93838776086578,0.00532365672661986));
#29197=CARTESIAN_POINT('Origin',(29.75,0.,0.));
#29198=CARTESIAN_POINT('',(60.9128916636063,-6.933,-1.66533453693773E-13));
#29199=CARTESIAN_POINT('',(60.7335483363939,-6.9239281092218,0.00189150495899608));
#29200=CARTESIAN_POINT('',(29.75,-6.933,-8.4904762584886E-16));
#29201=CARTESIAN_POINT('Ctrl Pts',(60.9128916636063,-6.93063399872081,-3.45088283915107E-5));
#29202=CARTESIAN_POINT('Ctrl Pts',(60.8848211492598,-6.93354690158584,0.980671123326722));
#29203=CARTESIAN_POINT('Ctrl Pts',(60.8567506349133,-6.73243917945665,1.96229231020105));
#29204=CARTESIAN_POINT('Ctrl Pts',(60.8286801205668,-6.32914499442313,2.85102798441176));
#29205=CARTESIAN_POINT('Ctrl Pts',(60.7625095857528,-5.3784608857645,4.94604178234169));
#29206=CARTESIAN_POINT('Ctrl Pts',(60.6963390509388,-3.30425725422927,6.52490486785065));
#29207=CARTESIAN_POINT('Ctrl Pts',(60.6301685161248,-1.03726127266794,6.86689254109988));
#29208=CARTESIAN_POINT('Ctrl Pts',(60.5639979813107,1.22973470889339,7.2088802143491));
#29209=CARTESIAN_POINT('Ctrl Pts',(60.4978274464967,3.6895230404809,6.31399247533858));
#29210=CARTESIAN_POINT('Ctrl Pts',(60.4316569116826,5.20930240162831,4.59254104319776));
#29211=CARTESIAN_POINT('Ctrl Pts',(60.3654863768686,6.72908176277572,2.87108961105695));
#29212=CARTESIAN_POINT('Ctrl Pts',(60.2993158420546,7.30885215348307,0.323074485785975));
#29213=CARTESIAN_POINT('Ctrl Pts',(60.2331453072406,6.68352405143822,-1.88647051366126));
#29214=CARTESIAN_POINT('Ctrl Pts',(60.1669747724266,6.05819594939336,-4.09601551310856));
#29215=CARTESIAN_POINT('Ctrl Pts',(60.1008042376125,4.22776935459611,-5.96709038673199));
#29216=CARTESIAN_POINT('Ctrl Pts',(60.0346337027984,2.03598966376562,-6.63964383139859));
#29217=CARTESIAN_POINT('Ctrl Pts',(59.9684631679844,-0.155790027064813,
-7.31219727606518));
#29218=CARTESIAN_POINT('Ctrl Pts',(59.9022926331704,-2.70892281392854,-6.78622929177505));
#29219=CARTESIAN_POINT('Ctrl Pts',(59.8361220983563,-4.4724720920668,-5.30880686350652));
#29220=CARTESIAN_POINT('Ctrl Pts',(59.8030368309493,-5.3542467311359,-4.57009564937227));
#29221=CARTESIAN_POINT('Ctrl Pts',(59.7699515635423,-6.03862549302366,-3.59352082424343));
#29222=CARTESIAN_POINT('Ctrl Pts',(59.7368662961352,-6.45644661012001,-2.51625128036857));
#29223=CARTESIAN_POINT('Ctrl Pts',(59.7122080852923,-6.7678456710154,-1.71337006980382));
#29224=CARTESIAN_POINT('Ctrl Pts',(59.6875498744493,-6.93118226952631,-0.854556837411979));
#29225=CARTESIAN_POINT('Ctrl Pts',(59.6628916636063,-6.93388706352457,0.00279784803854183));
#29226=CARTESIAN_POINT('Ctrl Pts',(59.483548336394,-6.93838776086578,0.00532365672661986));
#29227=CARTESIAN_POINT('Ctrl Pts',(59.5399225708173,-6.92067397764835,-1.9557048674237));
#29228=CARTESIAN_POINT('Ctrl Pts',(59.5962968052407,-6.04925198579133,-3.9302082888362));
#29229=CARTESIAN_POINT('Ctrl Pts',(59.6526710396641,-4.58163035911404,-5.21907916889889));
#29230=CARTESIAN_POINT('Ctrl Pts',(59.7188415744781,-2.85897622579923,-6.73192056377248));
#29231=CARTESIAN_POINT('Ctrl Pts',(59.7850121092921,-0.314912668733032,
-7.30013704141502));
#29232=CARTESIAN_POINT('Ctrl Pts',(59.8511826441062,1.89962274248406,-6.67666611150862));
#29233=CARTESIAN_POINT('Ctrl Pts',(59.8842679115132,3.00689044809264,-6.36493064655541));
#29234=CARTESIAN_POINT('Ctrl Pts',(59.9173531789202,4.03177611723897,-5.75527332971494));
#29235=CARTESIAN_POINT('Ctrl Pts',(59.9504384463273,4.85491496267529,-4.94439319234203));
#29236=CARTESIAN_POINT('Ctrl Pts',(59.9835237137343,5.67805380811161,-4.13351305496913));
#29237=CARTESIAN_POINT('Ctrl Pts',(60.0166089811413,6.29944582983796,-3.12141009706376));
#29238=CARTESIAN_POINT('Ctrl Pts',(60.0496942485483,6.63450760188871,-2.02204047394371));
#29239=CARTESIAN_POINT('Ctrl Pts',(60.0827795159553,6.96956937393944,-0.922670850823727));
#29240=CARTESIAN_POINT('Ctrl Pts',(60.1158647833623,7.01830089631462,0.263965437510784));
#29241=CARTESIAN_POINT('Ctrl Pts',(60.1489500507693,6.7873490757456,1.39610739531813));
#29242=CARTESIAN_POINT('Ctrl Pts',(60.1820353181763,6.55639725517657,2.52824935312553));
#29243=CARTESIAN_POINT('Ctrl Pts',(60.2151205855834,6.04576209166327,3.60589698040562));
#29244=CARTESIAN_POINT('Ctrl Pts',(60.2482058529904,5.30058452960073,4.48221380267472));
#29245=CARTESIAN_POINT('Ctrl Pts',(60.3143763878044,3.81022940547564,6.23484744721291));
#29246=CARTESIAN_POINT('Ctrl Pts',(60.3805469226185,1.38170468715351,7.18215787170724));
#29247=CARTESIAN_POINT('Ctrl Pts',(60.4467174574325,-0.891899061462053,
6.88728104428395));
#29248=CARTESIAN_POINT('Ctrl Pts',(60.5128879922466,-3.16550281007755,6.59240421686066));
#29249=CARTESIAN_POINT('Ctrl Pts',(60.5790585270606,-5.28418558898654,5.05534013751981));
#29250=CARTESIAN_POINT('Ctrl Pts',(60.6452290618746,-6.27173702357961,2.98221049762208));
#29251=CARTESIAN_POINT('Ctrl Pts',(60.6746688200477,-6.71110592848,2.05985985572997));
#29252=CARTESIAN_POINT('Ctrl Pts',(60.7041085782208,-6.92657579720744,1.03139902341889));
#29253=CARTESIAN_POINT('Ctrl Pts',(60.7335483363939,-6.9239281092218,0.00189150495899608));
#29254=CARTESIAN_POINT('Origin',(29.75,0.,0.));
#29255=CARTESIAN_POINT('',(62.1628916636063,-6.93103310215991,-0.000748976776520713));
#29256=CARTESIAN_POINT('',(61.9835483363939,-6.93044600006181,-0.00576111198420661));
#29257=CARTESIAN_POINT('',(29.75,-6.933,-8.4904762584886E-16));
#29258=CARTESIAN_POINT('Ctrl Pts',(62.1628916636063,-6.933,-1.69309011255336E-14));
#29259=CARTESIAN_POINT('Ctrl Pts',(62.1056674683212,-6.93300000000001,1.99420935701633));
#29260=CARTESIAN_POINT('Ctrl Pts',(62.0484432730361,-6.02307502629244,3.97063309653056));
#29261=CARTESIAN_POINT('Ctrl Pts',(61.991219077751,-4.50798484753971,5.26731066241136));
#29262=CARTESIAN_POINT('Ctrl Pts',(61.9339948824659,-2.99289466878698,6.56398822829216));
#29263=CARTESIAN_POINT('Ctrl Pts',(61.8767706871808,-0.899664345628471,
7.15779044292416));
#29264=CARTESIAN_POINT('Ctrl Pts',(61.8195464918957,1.07062371681882,6.849836045993));
#29265=CARTESIAN_POINT('Ctrl Pts',(61.7623222966106,3.04091177926611,6.54188164906185));
#29266=CARTESIAN_POINT('Ctrl Pts',(61.7050981013255,4.85311303639922,5.33766370386366));
#29267=CARTESIAN_POINT('Ctrl Pts',(61.6478739060404,5.90026971493791,3.64050907030685));
#29268=CARTESIAN_POINT('Ctrl Pts',(61.5906497107553,6.94742639347661,1.94335443675005));
#29269=CARTESIAN_POINT('Ctrl Pts',(61.5334255154702,7.2108600852751,-0.21646429312465));
#29270=CARTESIAN_POINT('Ctrl Pts',(61.4762013201851,6.60233935006059,-2.11556236179449));
#29271=CARTESIAN_POINT('Ctrl Pts',(61.4189771249,5.99381861484609,-4.01466043046434));
#29272=CARTESIAN_POINT('Ctrl Pts',(61.3617529296149,4.52419779647225,-5.619163127905));
#29273=CARTESIAN_POINT('Ctrl Pts',(61.3045287343298,2.68569473000316,-6.39167683923658));
#29274=CARTESIAN_POINT('Ctrl Pts',(61.2473045390447,0.847191663534068,-7.16419055056815));
#29275=CARTESIAN_POINT('Ctrl Pts',(61.1900803437596,-1.3273997899428,-7.09093574623768));
#29276=CARTESIAN_POINT('Ctrl Pts',(61.1328561484745,-3.10974706736292,-6.19644754492667));
#29277=CARTESIAN_POINT('Ctrl Pts',(61.0756319531895,-4.89209434478304,-5.30195934361565));
#29278=CARTESIAN_POINT('Ctrl Pts',(61.0184077579043,-6.25040525058722,-3.60219296582558));
#29279=CARTESIAN_POINT('Ctrl Pts',(60.9611835626192,-6.72974280712794,-1.66644854403299));
#29280=CARTESIAN_POINT('Ctrl Pts',(60.9450862629483,-6.86458158035582,-1.12191912096652));
#29281=CARTESIAN_POINT('Ctrl Pts',(60.9289889632773,-6.93299999999999,-0.560975745777744));
#29282=CARTESIAN_POINT('Ctrl Pts',(60.9128916636063,-6.933,-1.66533453693773E-13));
#29283=CARTESIAN_POINT('Ctrl Pts',(60.7335483363939,-6.9239281092218,0.00189150495899608));
#29284=CARTESIAN_POINT('Ctrl Pts',(60.7702791130349,-6.9206246977113,-1.28258272503899));
#29285=CARTESIAN_POINT('Ctrl Pts',(60.8070098896758,-6.57778798958841,-2.56868628191917));
#29286=CARTESIAN_POINT('Ctrl Pts',(60.8437406663167,-5.90664661057516,-3.65236780224111));
#29287=CARTESIAN_POINT('Ctrl Pts',(60.9099112011308,-4.69758467270039,-5.60462126175199));
#29288=CARTESIAN_POINT('Ctrl Pts',(60.9760817359448,-2.42304070667363,-6.89993298031901));
#29289=CARTESIAN_POINT('Ctrl Pts',(61.0422522707589,-0.130809673177829,
-6.94355909805576));
#29290=CARTESIAN_POINT('Ctrl Pts',(61.1084228055729,2.16142136031784,-6.98718521579251));
#29291=CARTESIAN_POINT('Ctrl Pts',(61.1745933403869,4.47133946128256,-5.77912573269915));
#29292=CARTESIAN_POINT('Ctrl Pts',(61.240763875201,5.76038884520191,-3.87354582784349));
#29293=CARTESIAN_POINT('Ctrl Pts',(61.273849142608,6.40491353716163,-2.9207558754156));
#29294=CARTESIAN_POINT('Ctrl Pts',(61.306934410015,6.79422104985998,-1.79358581754712));
#29295=CARTESIAN_POINT('Ctrl Pts',(61.340019677422,6.89955457142813,-0.642938606067334));
#29296=CARTESIAN_POINT('Ctrl Pts',(61.373104944829,7.00488809299628,0.507708605412388));
#29297=CARTESIAN_POINT('Ctrl Pts',(61.4061902122361,6.82624762343428,1.68183297050341));
#29298=CARTESIAN_POINT('Ctrl Pts',(61.4392754796431,6.37258105776411,2.73780011323174));
#29299=CARTESIAN_POINT('Ctrl Pts',(61.4723607470501,5.91891449209395,3.79376725596006));
#29300=CARTESIAN_POINT('Ctrl Pts',(61.5054460144571,5.19022183031563,4.73157717632567));
#29301=CARTESIAN_POINT('Ctrl Pts',(61.5385312818641,4.28307957908654,5.44724266528475));
#29302=CARTESIAN_POINT('Ctrl Pts',(61.5716165492711,3.3759373278574,6.16290815424387));
#29303=CARTESIAN_POINT('Ctrl Pts',(61.6047018166782,2.29034548717748,6.65642921179643));
#29304=CARTESIAN_POINT('Ctrl Pts',(61.6377870840852,1.15555838515488,6.84478792562842));
#29305=CARTESIAN_POINT('Ctrl Pts',(61.7039576188993,-1.11401581889026,7.22150535329239));
#29306=CARTESIAN_POINT('Ctrl Pts',(61.7701281537132,-3.58037106830612,6.37757340607417));
#29307=CARTESIAN_POINT('Ctrl Pts',(61.8362986885273,-5.12662795410679,4.68484897717745));
#29308=CARTESIAN_POINT('Ctrl Pts',(61.8853819044828,-6.27359254887378,3.42923937797663));
#29309=CARTESIAN_POINT('Ctrl Pts',(61.9344651204383,-6.91430020443789,1.70660679429336));
#29310=CARTESIAN_POINT('Ctrl Pts',(61.9835483363939,-6.93044600006181,-0.00576111198420661));
#29311=CARTESIAN_POINT('Origin',(29.75,0.,0.));
#29312=CARTESIAN_POINT('',(63.4128916636063,-6.94470568062749,-0.000764679492917131));
#29313=CARTESIAN_POINT('',(63.2335483363939,-6.94425137989254,0.00364565552205904));
#29314=CARTESIAN_POINT('',(29.75,-6.933,-8.4904762584886E-16));
#29315=CARTESIAN_POINT('Ctrl Pts',(63.4128916636063,-6.94470568062749,-0.000764679492917131));
#29316=CARTESIAN_POINT('Ctrl Pts',(63.411704768509,-6.94477403368304,0.0403562036678778));
#29317=CARTESIAN_POINT('Ctrl Pts',(63.4105178734116,-6.94444287705134,0.081477862393955));
#29318=CARTESIAN_POINT('Ctrl Pts',(63.4093309783143,-6.94370900561522,0.122594307078241));
#29319=CARTESIAN_POINT('Ctrl Pts',(63.3431604435003,-6.90279497241768,2.41487535244701));
#29320=CARTESIAN_POINT('Ctrl Pts',(63.2769899086863,-5.61017528801263,4.69095027501292));
#29321=CARTESIAN_POINT('Ctrl Pts',(63.2108193738722,-3.65935369701219,5.90232117604843));
#29322=CARTESIAN_POINT('Ctrl Pts',(63.1446488390582,-1.70853210601164,7.11369207708401));
#29323=CARTESIAN_POINT('Ctrl Pts',(63.0784783042442,0.900491391584395,7.26035895658904));
#29324=CARTESIAN_POINT('Ctrl Pts',(63.0123077694301,2.97478800230089,6.27526103731416));
#29325=CARTESIAN_POINT('Ctrl Pts',(62.9461372346161,5.0490846130174,5.29016311803928));
#29326=CARTESIAN_POINT('Ctrl Pts',(62.879966699802,6.58865433685436,3.17330039998448));
#29327=CARTESIAN_POINT('Ctrl Pts',(62.813796164988,6.88622097301192,0.900047126344276));
#29328=CARTESIAN_POINT('Ctrl Pts',(62.747625630174,7.18378760916946,-1.37320614729579));
#29329=CARTESIAN_POINT('Ctrl Pts',(62.68145509536,6.23935115764776,-3.80284997652125));
#29330=CARTESIAN_POINT('Ctrl Pts',(62.6152845605459,4.48848205404005,-5.29527768666486));
#29331=CARTESIAN_POINT('Ctrl Pts',(62.5821992931389,3.61304750223614,-6.04149154173671));
#29332=CARTESIAN_POINT('Ctrl Pts',(62.5491140257318,2.53600478741071,-6.55340136703808));
#29333=CARTESIAN_POINT('Ctrl Pts',(62.5160287583248,1.40413687274796,-6.78569252013943));
#29334=CARTESIAN_POINT('Ctrl Pts',(62.4829434909178,0.272268958085274,-7.01798367324077));
#29335=CARTESIAN_POINT('Ctrl Pts',(62.4498582235108,-0.914424156414728,
-6.97065615414214));
#29336=CARTESIAN_POINT('Ctrl Pts',(62.4167729561038,-2.01418943852191,-6.63689533618939));
#29337=CARTESIAN_POINT('Ctrl Pts',(62.3836876886968,-3.11395472062909,-6.30313451823664));
#29338=CARTESIAN_POINT('Ctrl Pts',(62.3506024212897,-4.12679217034345,-5.68294040142978));
#29339=CARTESIAN_POINT('Ctrl Pts',(62.3175171538827,-4.93864563719572,-4.86076152526476));
#29340=CARTESIAN_POINT('Ctrl Pts',(62.2844318864757,-5.75049910404804,-4.03858264909971));
#29341=CARTESIAN_POINT('Ctrl Pts',(62.2513466190687,-6.36136858803824,-3.01441901357648));
#29342=CARTESIAN_POINT('Ctrl Pts',(62.2182613516617,-6.67441389900069,-1.90752091290157));
#29343=CARTESIAN_POINT('Ctrl Pts',(62.1998047889765,-6.84904571726545,-1.29003960529028));
#29344=CARTESIAN_POINT('Ctrl Pts',(62.1813482262914,-6.93099619848535,-0.646811761486181));
#29345=CARTESIAN_POINT('Ctrl Pts',(62.1628916636063,-6.92559703060158,-0.00281898329623498));
#29346=CARTESIAN_POINT('Ctrl Pts',(61.9835483363939,-6.93044600006181,-0.00576111198420661));
#29347=CARTESIAN_POINT('Ctrl Pts',(62.0006356552524,-6.93606682894759,-0.601887014657739));
#29348=CARTESIAN_POINT('Ctrl Pts',(62.0177229741109,-6.86599438447961,-1.19676889799133));
#29349=CARTESIAN_POINT('Ctrl Pts',(62.0348102929694,-6.71523723016996,-1.77026938277931));
#29350=CARTESIAN_POINT('Ctrl Pts',(62.1009808277835,-6.13143109824698,-3.99114640326435));
#29351=CARTESIAN_POINT('Ctrl Pts',(62.1671513625975,-4.33766031221545,-5.89138353365921));
#29352=CARTESIAN_POINT('Ctrl Pts',(62.2333218974115,-2.15409411222323,-6.60213172397762));
#29353=CARTESIAN_POINT('Ctrl Pts',(62.2994924322255,0.0294720877690602,
-7.31287991429606));
#29354=CARTESIAN_POINT('Ctrl Pts',(62.3656629670396,2.60283370172207,-6.83413916453793));
#29355=CARTESIAN_POINT('Ctrl Pts',(62.4318335018536,4.38180475697552,-5.38794127571344));
#29356=CARTESIAN_POINT('Ctrl Pts',(62.4980040366677,6.16077581222893,-3.94174338688899));
#29357=CARTESIAN_POINT('Ctrl Pts',(62.5641745714817,7.14535630878282,-1.52808835899822));
#29358=CARTESIAN_POINT('Ctrl Pts',(62.6303451062957,6.8999800818199,0.759415432302316));
#29359=CARTESIAN_POINT('Ctrl Pts',(62.6634303737028,6.77729196833845,1.90316732795255));
#29360=CARTESIAN_POINT('Ctrl Pts',(62.6965156411098,6.3471146739778,3.01538141445524));
#29361=CARTESIAN_POINT('Ctrl Pts',(62.7296009085168,5.68488391631017,3.9622365140618));
#29362=CARTESIAN_POINT('Ctrl Pts',(62.7626861759238,5.02265315864249,4.90909161366842));
#29363=CARTESIAN_POINT('Ctrl Pts',(62.7957714433308,4.1283689376678,5.6905877263789));
#29364=CARTESIAN_POINT('Ctrl Pts',(62.8288567107379,3.10028353477502,6.20431952769911));
#29365=CARTESIAN_POINT('Ctrl Pts',(62.8619419781449,2.07219813188224,6.71805132901933));
#29366=CARTESIAN_POINT('Ctrl Pts',(62.8950272455519,0.910311547071365,6.96401881894927));
#29367=CARTESIAN_POINT('Ctrl Pts',(62.9281125129589,-0.244492304498008,
6.92513154014622));
#29368=CARTESIAN_POINT('Ctrl Pts',(62.9611977803659,-1.39929615606738,6.88624426134317));
#29369=CARTESIAN_POINT('Ctrl Pts',(62.994283047773,-2.54701727439525,6.56250221380711));
#29370=CARTESIAN_POINT('Ctrl Pts',(63.02736831518,-3.53534695572987,5.97392323611058));
#29371=CARTESIAN_POINT('Ctrl Pts',(63.093538849994,-5.51200631839906,4.79676528071754));
#29372=CARTESIAN_POINT('Ctrl Pts',(63.1597093848081,-6.8510999330953,2.56025960468261));
#29373=CARTESIAN_POINT('Ctrl Pts',(63.2258799196221,-6.93956701425102,0.269320948886368));
#29374=CARTESIAN_POINT('Ctrl Pts',(63.228436058546,-6.94298445904371,0.180822986962495));
#29375=CARTESIAN_POINT('Ctrl Pts',(63.23099219747,-6.94453566485637,0.092243797792992));
#29376=CARTESIAN_POINT('Ctrl Pts',(63.2335483363939,-6.94425137989254,0.00364565552205904));
#29377=CARTESIAN_POINT('Origin',(29.75,0.,0.));
#29378=CARTESIAN_POINT('',(64.6628916636063,-6.9266679019854,0.00480994512238903));
#29379=CARTESIAN_POINT('',(64.483548336394,-6.92953670012574,0.00054474835552538));
#29380=CARTESIAN_POINT('',(29.75,-6.933,-8.4904762584886E-16));
#29381=CARTESIAN_POINT('Ctrl Pts',(64.6628916636063,-6.9266679019854,0.00480994512238903));
#29382=CARTESIAN_POINT('Ctrl Pts',(64.6420613107265,-6.93261174586027,0.732499836952666));
#29383=CARTESIAN_POINT('Ctrl Pts',(64.6212309578468,-6.82760440508976,1.45863474940064));
#29384=CARTESIAN_POINT('Ctrl Pts',(64.600400604967,-6.60467572025062,2.14628128990626));
#29385=CARTESIAN_POINT('Ctrl Pts',(64.534230070153,-5.89651151456714,4.33068688355847));
#29386=CARTESIAN_POINT('Ctrl Pts',(64.4680595353389,-3.99839801476722,6.12670468035998));
#29387=CARTESIAN_POINT('Ctrl Pts',(64.4018890005249,-1.77821327916756,6.71313803514095));
#29388=CARTESIAN_POINT('Ctrl Pts',(64.3357184657109,0.441971456432111,7.29957138992192));
#29389=CARTESIAN_POINT('Ctrl Pts',(64.2695479308968,2.9842274278316,6.67642030268235));
#29390=CARTESIAN_POINT('Ctrl Pts',(64.2033773960828,4.67878012636471,5.13216724668294));
#29391=CARTESIAN_POINT('Ctrl Pts',(64.1372068612687,6.37333282489787,3.58791419068348));
#29392=CARTESIAN_POINT('Ctrl Pts',(64.0710363264547,7.22018225056462,1.12255916592427));
#29393=CARTESIAN_POINT('Ctrl Pts',(64.0048657916407,6.84615033414182,-1.14745916295991));
#29394=CARTESIAN_POINT('Ctrl Pts',(63.9717805242337,6.65913437593043,-2.28246832740194));
#29395=CARTESIAN_POINT('Ctrl Pts',(63.9386952568267,6.16689808219666,-3.3686433178752));
#29396=CARTESIAN_POINT('Ctrl Pts',(63.9056099894197,5.45230637984183,-4.27663167406574));
#29397=CARTESIAN_POINT('Ctrl Pts',(63.8725247220126,4.73771467748695,-5.18462003025633));
#29398=CARTESIAN_POINT('Ctrl Pts',(63.8394394546056,3.80076756651095,-5.9144217521642));
#29399=CARTESIAN_POINT('Ctrl Pts',(63.8063541871985,2.7453379186447,-6.36933736822265));
#29400=CARTESIAN_POINT('Ctrl Pts',(63.7732689197915,1.68990827077845,-6.8242529842811));
#29401=CARTESIAN_POINT('Ctrl Pts',(63.7401836523845,0.515996086021923,-7.00428249449014));
#29402=CARTESIAN_POINT('Ctrl Pts',(63.7070983849775,-0.634774945489243,
-6.90031043532577));
#29403=CARTESIAN_POINT('Ctrl Pts',(63.6740131175705,-1.78554597700034,-6.7963383761614));
#29404=CARTESIAN_POINT('Ctrl Pts',(63.6409278501635,-2.91317585526612,-6.40836474762363));
#29405=CARTESIAN_POINT('Ctrl Pts',(63.6078425827564,-3.86672771044496,-5.76496780056987));
#29406=CARTESIAN_POINT('Ctrl Pts',(63.5428589430397,-5.73962386829838,-4.50125501602957));
#29407=CARTESIAN_POINT('Ctrl Pts',(63.477875303323,-6.94096328557867,-2.25217229100375));
#29408=CARTESIAN_POINT('Ctrl Pts',(63.4128916636063,-6.94470568062749,-0.000764679492917131));
#29409=CARTESIAN_POINT('Ctrl Pts',(63.2335483363939,-6.94425137989254,0.00364565552205904));
#29410=CARTESIAN_POINT('Ctrl Pts',(63.297162732284,-6.93717640596789,-2.20128821749584));
#29411=CARTESIAN_POINT('Ctrl Pts',(63.3607771281741,-5.79327512818524,-4.41796084971756));
#29412=CARTESIAN_POINT('Ctrl Pts',(63.4243915240642,-3.98649763460576,-5.6864840942668));
#29413=CARTESIAN_POINT('Ctrl Pts',(63.4905620588782,-2.10712062618958,-7.00597884606616));
#29414=CARTESIAN_POINT('Ctrl Pts',(63.5567325936923,0.489473938257958,-7.29959671410731));
#29415=CARTESIAN_POINT('Ctrl Pts',(63.6229031285063,2.61604017008766,-6.43308624017697));
#29416=CARTESIAN_POINT('Ctrl Pts',(63.6890736633204,4.74260640191736,-5.56657576624663));
#29417=CARTESIAN_POINT('Ctrl Pts',(63.7552441981344,6.39914430112923,-3.53993695034479));
#29418=CARTESIAN_POINT('Ctrl Pts',(63.8214147329484,6.82447958873384,-1.28709069678286));
#29419=CARTESIAN_POINT('Ctrl Pts',(63.8875852677624,7.24981487633844,0.965755556779008));
#29420=CARTESIAN_POINT('Ctrl Pts',(63.9537558025765,6.44394755233585,3.44480924800095));
#29421=CARTESIAN_POINT('Ctrl Pts',(64.0199263373905,4.78006004588273,5.03363316959887));
#29422=CARTESIAN_POINT('Ctrl Pts',(64.0530116047975,3.94811629265612,5.82804513039787));
#29423=CARTESIAN_POINT('Ctrl Pts',(64.0860968722045,2.90166749381685,6.39989964879084));
#29424=CARTESIAN_POINT('Ctrl Pts',(64.1191821396116,1.78470649325174,6.69567368292629));
#29425=CARTESIAN_POINT('Ctrl Pts',(64.1522674070186,0.667745492686632,6.99144771706174));
#29426=CARTESIAN_POINT('Ctrl Pts',(64.1853526744256,-0.519727709604317,
7.01114126693967));
#29427=CARTESIAN_POINT('Ctrl Pts',(64.2184379418327,-1.63657026372325,6.73995375130146));
#29428=CARTESIAN_POINT('Ctrl Pts',(64.2515232092397,-2.75341281784225,6.46876623566324));
#29429=CARTESIAN_POINT('Ctrl Pts',(64.2846084766467,-3.79962472378922,5.90669765450884));
#29430=CARTESIAN_POINT('Ctrl Pts',(64.3176937440537,-4.6565674166262,5.13162773685908));
#29431=CARTESIAN_POINT('Ctrl Pts',(64.3507790114607,-5.51351010946303,4.35655781920945));
#29432=CARTESIAN_POINT('Ctrl Pts',(64.3838642788677,-6.18118358918994,3.36848656506454));
#29433=CARTESIAN_POINT('Ctrl Pts',(64.4169495462748,-6.55617454016449,2.281011251009));
#29434=CARTESIAN_POINT('Ctrl Pts',(64.4391491429812,-6.80778646694058,1.55133561915753));
#29435=CARTESIAN_POINT('Ctrl Pts',(64.4613487396876,-6.92762805264689,0.776906694603623));
#29436=CARTESIAN_POINT('Ctrl Pts',(64.483548336394,-6.92250999810812,0.0016499903344943));
#29437=CARTESIAN_POINT('Origin',(29.75,0.,0.));
#29438=CARTESIAN_POINT('',(65.9128916636062,-6.92558145942544,-0.00361457160125256));
#29439=CARTESIAN_POINT('',(65.7335483363939,-6.933,-5.0499882053856E-12));
#29440=CARTESIAN_POINT('',(29.75,-6.933,-8.4904762584886E-16));
#29441=CARTESIAN_POINT('Ctrl Pts',(65.9128916636062,-6.92558145942544,-0.00361457160125256));
#29442=CARTESIAN_POINT('Ctrl Pts',(65.8724178529441,-6.91851212277228,1.41090647206241));
#29443=CARTESIAN_POINT('Ctrl Pts',(65.8319440422819,-6.49691708916176,2.82927471017481));
#29444=CARTESIAN_POINT('Ctrl Pts',(65.7914702316197,-5.69119674035493,3.97976687862786));
#29445=CARTESIAN_POINT('Ctrl Pts',(65.7252996968056,-4.37392649772603,5.86070373237007));
#29446=CARTESIAN_POINT('Ctrl Pts',(65.6591291619916,-2.02993151309655,7.02563729856908));
#29447=CARTESIAN_POINT('Ctrl Pts',(65.5929586271776,0.261110209086824,6.93988080424563));
#29448=CARTESIAN_POINT('Ctrl Pts',(65.5267880923635,2.55215193127013,6.85412430992217));
#29449=CARTESIAN_POINT('Ctrl Pts',(65.4606175575495,4.79024039100734,5.51767775507631));
#29450=CARTESIAN_POINT('Ctrl Pts',(65.3944470227355,5.96973620774678,3.54241253078668));
#29451=CARTESIAN_POINT('Ctrl Pts',(65.3613617553284,6.55948411611648,2.55477991864189));
#29452=CARTESIAN_POINT('Ctrl Pts',(65.3282764879214,6.88458386373675,1.40744263913616));
#29453=CARTESIAN_POINT('Ctrl Pts',(65.2951912205144,6.92483742193198,0.252685605335446));
#29454=CARTESIAN_POINT('Ctrl Pts',(65.2621059531074,6.96509098012721,-0.902071428465336));
#29455=CARTESIAN_POINT('Ctrl Pts',(65.2290206857003,6.72049834889736,-2.06424821656111));
#29456=CARTESIAN_POINT('Ctrl Pts',(65.1959354182933,6.20798328677723,-3.09294072184353));
#29457=CARTESIAN_POINT('Ctrl Pts',(65.1628501508863,5.69546822465709,-4.12163322712596));
#29458=CARTESIAN_POINT('Ctrl Pts',(65.1297648834793,4.91503073164666,-5.01684144959503));
#29459=CARTESIAN_POINT('Ctrl Pts',(65.0966796160723,3.96895981333477,-5.6801920157194));
#29460=CARTESIAN_POINT('Ctrl Pts',(65.0635943486653,3.02288889502287,-6.34354258184377));
#29461=CARTESIAN_POINT('Ctrl Pts',(65.0305090812582,1.91118455140951,-6.77503549162344));
#29462=CARTESIAN_POINT('Ctrl Pts',(64.9974238138512,0.767578614783853,-6.89907674971449));
#29463=CARTESIAN_POINT('Ctrl Pts',(64.9312532790372,-1.5196332584674,-7.14715926589657));
#29464=CARTESIAN_POINT('Ctrl Pts',(64.8650827442231,-3.93445150376781,-6.16543517532421));
#29465=CARTESIAN_POINT('Ctrl Pts',(64.7989122094091,-5.38275317063448,-4.38817643478656));
#29466=CARTESIAN_POINT('Ctrl Pts',(64.7535720274748,-6.37513235052187,-3.17039521438781));
#29467=CARTESIAN_POINT('Ctrl Pts',(64.7082318455406,-6.91373029289969,-1.57910907333059));
#29468=CARTESIAN_POINT('Ctrl Pts',(64.6628916636063,-6.9266679019854,0.00480994512238903));
#29469=CARTESIAN_POINT('Ctrl Pts',(64.4835483363939,-6.933,-5.39651656694673E-12));
#29470=CARTESIAN_POINT('Ctrl Pts',(64.540772531679,-6.93299999999845,-1.99420935702167));
#29471=CARTESIAN_POINT('Ctrl Pts',(64.5979967269641,-6.0230750262894,-3.97063309653513));
#29472=CARTESIAN_POINT('Ctrl Pts',(64.6552209222492,-4.50798484753575,-5.26731066241475));
#29473=CARTESIAN_POINT('Ctrl Pts',(64.7124451175343,-2.99289466878209,-6.56398822829437));
#29474=CARTESIAN_POINT('Ctrl Pts',(64.7696693128194,-0.899664345623224,
-7.1577904429248));
#29475=CARTESIAN_POINT('Ctrl Pts',(64.8268935081045,1.07062371682378,-6.84983604599223));
#29476=CARTESIAN_POINT('Ctrl Pts',(64.8841177033896,3.04091177927078,-6.54188164905966));
#29477=CARTESIAN_POINT('Ctrl Pts',(64.9413418986747,4.85311303640296,-5.33766370386023));
#29478=CARTESIAN_POINT('Ctrl Pts',(64.9985660939598,5.90026971494045,-3.64050907030275));
#29479=CARTESIAN_POINT('Ctrl Pts',(65.0557902892449,6.94742639347793,-1.94335443674527));
#29480=CARTESIAN_POINT('Ctrl Pts',(65.11301448453,7.21086008527493,0.216464293129524));
#29481=CARTESIAN_POINT('Ctrl Pts',(65.1702386798151,6.60233935005918,2.1155623617989));
#29482=CARTESIAN_POINT('Ctrl Pts',(65.2274628751002,5.99381861484343,4.01466043046827));
#29483=CARTESIAN_POINT('Ctrl Pts',(65.2846870703853,4.5241977964686,5.61916312790792));
#29484=CARTESIAN_POINT('Ctrl Pts',(65.3419112656703,2.68569472999908,6.39167683923829));
#29485=CARTESIAN_POINT('Ctrl Pts',(65.3991354609554,0.847191663529553,7.16419055056866));
#29486=CARTESIAN_POINT('Ctrl Pts',(65.4563596562406,-1.32739978994719,7.09093574623684));
#29487=CARTESIAN_POINT('Ctrl Pts',(65.5135838515256,-3.1097470673667,6.19644754492477));
#29488=CARTESIAN_POINT('Ctrl Pts',(65.5708080468107,-4.89209434478622,5.30195934361269));
#29489=CARTESIAN_POINT('Ctrl Pts',(65.6280322420958,-6.25040525058933,3.60219296582188));
#29490=CARTESIAN_POINT('Ctrl Pts',(65.6852564373809,-6.72974280712892,1.66644854402908));
#29491=CARTESIAN_POINT('Ctrl Pts',(65.7013537370519,-6.86458158035656,1.1219191209622));
#29492=CARTESIAN_POINT('Ctrl Pts',(65.7174510367229,-6.93300000000039,0.560975745773053));
#29493=CARTESIAN_POINT('Ctrl Pts',(65.7335483363939,-6.933,-4.85292361851464E-12));
#29494=CARTESIAN_POINT('Origin',(29.75,0.,0.));
#29495=CARTESIAN_POINT('',(67.1628916636063,-6.94182785481333,-0.00394764471083664));
#29496=CARTESIAN_POINT('',(66.9835483363939,-6.933,-4.50639525695351E-12));
#29497=CARTESIAN_POINT('',(29.75,-6.933,-8.4904762584886E-16));
#29498=CARTESIAN_POINT('Ctrl Pts',(67.1628916636063,-6.94182785481333,-0.00394764471083664));
#29499=CARTESIAN_POINT('Ctrl Pts',(67.1027743951617,-6.92719609612228,2.08459150757714));
#29500=CARTESIAN_POINT('Ctrl Pts',(67.042657126717,-5.92001797146785,4.18526716644349));
#29501=CARTESIAN_POINT('Ctrl Pts',(66.9825398582723,-4.27990668625507,5.4692342224079));
#29502=CARTESIAN_POINT('Ctrl Pts',(66.9163693234583,-2.47465099675213,6.88248517300629));
#29503=CARTESIAN_POINT('Ctrl Pts',(66.8501987886443,0.0974162692902572,
7.30627680879808));
#29504=CARTESIAN_POINT('Ctrl Pts',(66.7840282538302,2.27325271597746,6.55886872652768));
#29505=CARTESIAN_POINT('Ctrl Pts',(66.7509429864232,3.36117093932118,6.18516468539243));
#29506=CARTESIAN_POINT('Ctrl Pts',(66.7178577190162,4.35003145782598,5.51866071474172));
#29507=CARTESIAN_POINT('Ctrl Pts',(66.6847724516092,5.12611472467068,4.66263564681462));
#29508=CARTESIAN_POINT('Ctrl Pts',(66.6516871842021,5.90219799151526,3.80661057888767));
#29509=CARTESIAN_POINT('Ctrl Pts',(66.6186019167951,6.46550400669962,2.76106441368453));
#29510=CARTESIAN_POINT('Ctrl Pts',(66.5855166493881,6.738012725561,1.64454349610523));
#29511=CARTESIAN_POINT('Ctrl Pts',(66.5524313819811,7.01052144442241,0.528022578525872));
#29512=CARTESIAN_POINT('Ctrl Pts',(66.519346114574,6.99223286696077,-0.659473091429799));
#29513=CARTESIAN_POINT('Ctrl Pts',(66.486260847167,6.69778057245195,-1.77678325488286));
#29514=CARTESIAN_POINT('Ctrl Pts',(66.45317557976,6.40332827794312,-2.89409341833599));
#29515=CARTESIAN_POINT('Ctrl Pts',(66.420090312353,5.8327122663871,-3.94121807528664));
#29516=CARTESIAN_POINT('Ctrl Pts',(66.387005044946,5.03928517632311,-4.77410115534899));
#29517=CARTESIAN_POINT('Ctrl Pts',(66.320834510132,3.45243099619514,-6.43986731547369));
#29518=CARTESIAN_POINT('Ctrl Pts',(66.2546639753179,0.974332502035366,-7.24866716804506));
#29519=CARTESIAN_POINT('Ctrl Pts',(66.1884934405039,-1.27901541039728,-6.82599763384204));
#29520=CARTESIAN_POINT('Ctrl Pts',(66.1223229056898,-3.5323633228298,-6.40332809963903));
#29521=CARTESIAN_POINT('Ctrl Pts',(66.0561523708758,-5.56096065353515,-4.74918917866183));
#29522=CARTESIAN_POINT('Ctrl Pts',(65.9899818360618,-6.42998656857364,-2.62364964753062));
#29523=CARTESIAN_POINT('Ctrl Pts',(65.9642851119099,-6.76746486283719,-1.79821574165669));
#29524=CARTESIAN_POINT('Ctrl Pts',(65.9385883877581,-6.93006976410791,-0.901690548913561));
#29525=CARTESIAN_POINT('Ctrl Pts',(65.9128916636062,-6.92558145942544,-0.00361457160125256));
#29526=CARTESIAN_POINT('Ctrl Pts',(65.7335483363939,-6.93201917574831,-0.00104661053196153));
#29527=CARTESIAN_POINT('Ctrl Pts',(65.7578758167191,-6.93536664097712,-0.850911801504528));
#29528=CARTESIAN_POINT('Ctrl Pts',(65.7822032970444,-6.78541196678331,-1.70071837762845));
#29529=CARTESIAN_POINT('Ctrl Pts',(65.8065307773696,-6.47990263081343,-2.48943745121956));
#29530=CARTESIAN_POINT('Ctrl Pts',(65.8727013121836,-5.64891989517595,-4.63474646883597));
#29531=CARTESIAN_POINT('Ctrl Pts',(65.9388718469976,-3.66708891267972,-6.32810859915136));
#29532=CARTESIAN_POINT('Ctrl Pts',(66.0050423818116,-1.42299593951584,-6.79744118581012));
#29533=CARTESIAN_POINT('Ctrl Pts',(66.0712129166256,0.821097033647975,-7.26677377246886));
#29534=CARTESIAN_POINT('Ctrl Pts',(66.1373834514397,3.32745199747944,-6.51207681547106));
#29535=CARTESIAN_POINT('Ctrl Pts',(66.2035539862538,4.94192445361747,-4.87910313893728));
#29536=CARTESIAN_POINT('Ctrl Pts',(66.2697245210678,6.55639690975559,-3.24612946240341));
#29537=CARTESIAN_POINT('Ctrl Pts',(66.3358950558818,7.27898685820016,-0.734879066333458));
#29538=CARTESIAN_POINT('Ctrl Pts',(66.4020655906958,6.77930311774462,1.50642423731264));
#29539=CARTESIAN_POINT('Ctrl Pts',(66.4682361255099,6.2796193772891,3.74772754095867));
#29540=CARTESIAN_POINT('Ctrl Pts',(66.534406660324,4.55766194793354,5.71908375218086));
#29541=CARTESIAN_POINT('Ctrl Pts',(66.600577195138,2.40731390636405,6.51421245228286));
#29542=CARTESIAN_POINT('Ctrl Pts',(66.666747729952,0.256965864794573,7.30934115238486));
#29543=CARTESIAN_POINT('Ctrl Pts',(66.7329182647661,-2.32177278898883,6.92824234136667));
#29544=CARTESIAN_POINT('Ctrl Pts',(66.7990887995801,-4.16586038519456,5.55266099999641));
#29545=CARTESIAN_POINT('Ctrl Pts',(66.8321740669871,-5.08790418329745,4.86487032931126));
#29546=CARTESIAN_POINT('Ctrl Pts',(66.8652593343941,-5.82628521700591,3.92845902603808));
#29547=CARTESIAN_POINT('Ctrl Pts',(66.8983446018012,-6.3042136615862,2.87647587172514));
#29548=CARTESIAN_POINT('Ctrl Pts',(66.9267458466654,-6.71447973606366,1.97342646332384));
#29549=CARTESIAN_POINT('Ctrl Pts',(66.9551470915296,-6.93281966865977,0.98521276627255));
#29550=CARTESIAN_POINT('Ctrl Pts',(66.9835483363939,-6.93511079172564,-0.00169474912669407));
#29551=CARTESIAN_POINT('Origin',(29.75,0.,0.));
#29552=CARTESIAN_POINT('',(68.4128916636063,-6.93357857970305,0.00297544388368854));
#29553=CARTESIAN_POINT('',(68.2335483363939,-6.933,-4.7509218781272E-12));
#29554=CARTESIAN_POINT('',(29.75,-6.933,-8.4904762584886E-16));
#29555=CARTESIAN_POINT('Ctrl Pts',(68.4128916636063,-6.93473393447276,0.0089170509982972));
#29556=CARTESIAN_POINT('Ctrl Pts',(68.3993014721933,-6.93916860973486,0.481932871115519));
#29557=CARTESIAN_POINT('Ctrl Pts',(68.3857112807802,-6.89496607960317,0.95394242452496));
#29558=CARTESIAN_POINT('Ctrl Pts',(68.3721210893672,-6.79911921480736,1.41495069786618));
#29559=CARTESIAN_POINT('Ctrl Pts',(68.3059505545531,-6.33244158599193,3.65959634512357));
#29560=CARTESIAN_POINT('Ctrl Pts',(68.239780019739,-4.6414273666631,5.643433719458));
#29561=CARTESIAN_POINT('Ctrl Pts',(68.173609484925,-2.49710289781263,6.47695380660065));
#29562=CARTESIAN_POINT('Ctrl Pts',(68.140524217518,-1.42494066338746,6.89371385017195));
#29563=CARTESIAN_POINT('Ctrl Pts',(68.107438950111,-0.239450866581887,7.02289457194535));
#29564=CARTESIAN_POINT('Ctrl Pts',(68.074353682704,0.905844897653366,6.86998260787669));
#29565=CARTESIAN_POINT('Ctrl Pts',(68.041268415297,2.05114066188868,6.71707064380802));
#29566=CARTESIAN_POINT('Ctrl Pts',(68.0081831478899,3.15624239355368,6.28206599389726));
#29567=CARTESIAN_POINT('Ctrl Pts',(67.9750978804829,4.08504323520468,5.60515498849634));
#29568=CARTESIAN_POINT('Ctrl Pts',(67.9420126130759,5.01384407685567,4.92824398309542));
#29569=CARTESIAN_POINT('Ctrl Pts',(67.9089273456688,5.76634402849265,4.00942662220434));
#29570=CARTESIAN_POINT('Ctrl Pts',(67.8758420782618,6.26260800157698,2.96596768737957));
#29571=CARTESIAN_POINT('Ctrl Pts',(67.8427568108548,6.75887197466129,1.92250875255486));
#29572=CARTESIAN_POINT('Ctrl Pts',(67.8096715434478,6.99889996919296,0.754408243796477));
#29573=CARTESIAN_POINT('Ctrl Pts',(67.7765862760408,6.93046212332443,-0.39386735146852));
#29574=CARTESIAN_POINT('Ctrl Pts',(67.7104157412267,6.79358643158735,-2.69041854199858));
#29575=CARTESIAN_POINT('Ctrl Pts',(67.6442452064128,5.42284737824935,-4.9076700785551));
#29576=CARTESIAN_POINT('Ctrl Pts',(67.5780746715987,3.42892195617063,-6.03925647982234));
#29577=CARTESIAN_POINT('Ctrl Pts',(67.5119041367847,1.43499653409197,-7.17084288108956));
#29578=CARTESIAN_POINT('Ctrl Pts',(67.4457336019706,-1.18211525672738,-7.21676414706757));
#29579=CARTESIAN_POINT('Ctrl Pts',(67.3795630671565,-3.21780841116017,-6.15418342104918));
#29580=CARTESIAN_POINT('Ctrl Pts',(67.3133925323425,-5.25350156559306,-5.09160269503072));
#29581=CARTESIAN_POINT('Ctrl Pts',(67.2472219975285,-6.7077760836393,-2.92051997701569));
#29582=CARTESIAN_POINT('Ctrl Pts',(67.1810514627145,-6.91569128618054,-0.633623485305609));
#29583=CARTESIAN_POINT('Ctrl Pts',(67.1749981963451,-6.93471132443119,-0.424418683463479));
#29584=CARTESIAN_POINT('Ctrl Pts',(67.1689449299757,-6.94330114086077,-0.214244688119485));
#29585=CARTESIAN_POINT('Ctrl Pts',(67.1628916636063,-6.94182785481333,-0.00394764471083664));
#29586=CARTESIAN_POINT('Ctrl Pts',(66.9835483363939,-6.933,-4.50639525695351E-12));
#29587=CARTESIAN_POINT('Ctrl Pts',(67.040772531679,-6.9329999999987,-1.99420935702078));
#29588=CARTESIAN_POINT('Ctrl Pts',(67.0979967269641,-6.02307502628991,-3.97063309653436));
#29589=CARTESIAN_POINT('Ctrl Pts',(67.1552209222492,-4.50798484753642,-5.26731066241417));
#29590=CARTESIAN_POINT('Ctrl Pts',(67.2124451175343,-2.99289466878293,-6.56398822829398));
#29591=CARTESIAN_POINT('Ctrl Pts',(67.2696693128194,-0.899664345624143,
-7.15779044292469));
#29592=CARTESIAN_POINT('Ctrl Pts',(67.3268935081045,1.0706237168229,-6.84983604599237));
#29593=CARTESIAN_POINT('Ctrl Pts',(67.3841177033896,3.04091177926994,-6.54188164906005));
#29594=CARTESIAN_POINT('Ctrl Pts',(67.4413418986747,4.85311303640228,-5.33766370386085));
#29595=CARTESIAN_POINT('Ctrl Pts',(67.4985660939598,5.90026971493998,-3.64050907030351));
#29596=CARTESIAN_POINT('Ctrl Pts',(67.5557902892448,6.94742639347768,-1.94335443674616));
#29597=CARTESIAN_POINT('Ctrl Pts',(67.6130144845299,7.21086008527496,0.216464293128598));
#29598=CARTESIAN_POINT('Ctrl Pts',(67.670238679815,6.60233935005945,2.11556236179805));
#29599=CARTESIAN_POINT('Ctrl Pts',(67.7274628751001,5.99381861484394,4.0146604304675));
#29600=CARTESIAN_POINT('Ctrl Pts',(67.7846870703852,4.52419779646933,5.61916312790734));
#29601=CARTESIAN_POINT('Ctrl Pts',(67.8419112656703,2.6856947299999,6.39167683923795));
#29602=CARTESIAN_POINT('Ctrl Pts',(67.8991354609554,0.847191663530473,7.16419055056855));
#29603=CARTESIAN_POINT('Ctrl Pts',(67.9563596562405,-1.32739978994628,7.09093574623701));
#29604=CARTESIAN_POINT('Ctrl Pts',(68.0135838515256,-3.10974706736591,6.19644754492517));
#29605=CARTESIAN_POINT('Ctrl Pts',(68.0708080468107,-4.89209434478554,5.30195934361332));
#29606=CARTESIAN_POINT('Ctrl Pts',(68.1280322420958,-6.25040525058887,3.60219296582268));
#29607=CARTESIAN_POINT('Ctrl Pts',(68.1852564373809,-6.7297428071287,1.66644854402994));
#29608=CARTESIAN_POINT('Ctrl Pts',(68.2013537370519,-6.86458158035646,1.12191912096289));
#29609=CARTESIAN_POINT('Ctrl Pts',(68.2174510367229,-6.93300000000037,0.560975745773549));
#29610=CARTESIAN_POINT('Ctrl Pts',(68.2335483363939,-6.933,-4.55399606913431E-12));
#29611=CARTESIAN_POINT('Origin',(29.75,0.,0.));
#29612=CARTESIAN_POINT('',(69.6628916636063,-6.92775586673719,-0.00132508185730362));
#29613=CARTESIAN_POINT('',(69.4835483363939,-6.92774438460107,0.00106183211813038));
#29614=CARTESIAN_POINT('',(29.75,-6.933,-8.4904762584886E-16));
#29615=CARTESIAN_POINT('Ctrl Pts',(69.6628916636063,-6.933,8.80129302771593E-13));
#29616=CARTESIAN_POINT('Ctrl Pts',(69.6056674683212,-6.93299999999975,1.99420935701716));
#29617=CARTESIAN_POINT('Ctrl Pts',(69.5484432730361,-6.02307502629199,3.97063309653121));
#29618=CARTESIAN_POINT('Ctrl Pts',(69.491219077751,-4.50798484753918,5.26731066241181));
#29619=CARTESIAN_POINT('Ctrl Pts',(69.4339948824659,-2.99289466878637,6.56398822829242));
#29620=CARTESIAN_POINT('Ctrl Pts',(69.3767706871808,-0.899664345627887,
7.15779044292421));
#29621=CARTESIAN_POINT('Ctrl Pts',(69.3195464918957,1.07062371681932,6.84983604599292));
#29622=CARTESIAN_POINT('Ctrl Pts',(69.2623222966106,3.04091177926652,6.54188164906164));
#29623=CARTESIAN_POINT('Ctrl Pts',(69.2050981013255,4.85311303639948,5.33766370386339));
#29624=CARTESIAN_POINT('Ctrl Pts',(69.1478739060404,5.90026971493807,3.64050907030659));
#29625=CARTESIAN_POINT('Ctrl Pts',(69.0906497107553,6.94742639347666,1.9433544367498));
#29626=CARTESIAN_POINT('Ctrl Pts',(69.0334255154702,7.21086008527507,-0.216464293124826));
#29627=CARTESIAN_POINT('Ctrl Pts',(68.9762013201851,6.60233935006056,-2.1155623617946));
#29628=CARTESIAN_POINT('Ctrl Pts',(68.9189771249,5.99381861484604,-4.01466043046437));
#29629=CARTESIAN_POINT('Ctrl Pts',(68.8617529296149,4.52419779647226,-5.61916312790497));
#29630=CARTESIAN_POINT('Ctrl Pts',(68.8045287343298,2.68569473000324,-6.39167683923654));
#29631=CARTESIAN_POINT('Ctrl Pts',(68.7473045390447,0.84719166353422,-7.16419055056811));
#29632=CARTESIAN_POINT('Ctrl Pts',(68.6900803437596,-1.32739978994257,-7.09093574623771));
#29633=CARTESIAN_POINT('Ctrl Pts',(68.6328561484745,-3.10974706736267,-6.19644754492679));
#29634=CARTESIAN_POINT('Ctrl Pts',(68.5756319531894,-4.89209434478277,-5.30195934361588));
#29635=CARTESIAN_POINT('Ctrl Pts',(68.5184077579043,-6.25040525058698,-3.60219296582595));
#29636=CARTESIAN_POINT('Ctrl Pts',(68.4611835626193,-6.72974280712783,-1.66644854403346));
#29637=CARTESIAN_POINT('Ctrl Pts',(68.4450862629483,-6.86458158035586,-1.12191912096655));
#29638=CARTESIAN_POINT('Ctrl Pts',(68.4289889632773,-6.93300000000006,-0.560975745777307));
#29639=CARTESIAN_POINT('Ctrl Pts',(68.4128916636063,-6.933,7.30526750203353E-13));
#29640=CARTESIAN_POINT('Ctrl Pts',(68.2335483363939,-6.933,-4.55399606913431E-12));
#29641=CARTESIAN_POINT('Ctrl Pts',(68.290772531679,-6.93299999999869,-1.99420935702096));
#29642=CARTESIAN_POINT('Ctrl Pts',(68.3479967269641,-6.02307502628976,-3.97063309653466));
#29643=CARTESIAN_POINT('Ctrl Pts',(68.4052209222492,-4.50798484753609,-5.26731066241446));
#29644=CARTESIAN_POINT('Ctrl Pts',(68.4624451175343,-2.99289466878242,-6.56398822829426));
#29645=CARTESIAN_POINT('Ctrl Pts',(68.5196693128194,-0.89966434562341,-7.15779044292481));
#29646=CARTESIAN_POINT('Ctrl Pts',(68.5768935081045,1.07062371682373,-6.84983604599224));
#29647=CARTESIAN_POINT('Ctrl Pts',(68.6341177033896,3.04091177927086,-6.54188164905966));
#29648=CARTESIAN_POINT('Ctrl Pts',(68.6913418986747,4.85311303640315,-5.3376637038601));
#29649=CARTESIAN_POINT('Ctrl Pts',(68.7485660939598,5.90026971494062,-3.64050907030246));
#29650=CARTESIAN_POINT('Ctrl Pts',(68.8057902892449,6.94742639347809,-1.94335443674482));
#29651=CARTESIAN_POINT('Ctrl Pts',(68.86301448453,7.21086008527495,0.216464293130162));
#29652=CARTESIAN_POINT('Ctrl Pts',(68.9202386798151,6.60233935005896,2.1155623617996));
#29653=CARTESIAN_POINT('Ctrl Pts',(68.9774628751002,5.99381861484296,4.01466043046903));
#29654=CARTESIAN_POINT('Ctrl Pts',(69.0346870703853,4.52419779646781,5.6191631279086));
#29655=CARTESIAN_POINT('Ctrl Pts',(69.0919112656704,2.68569472999804,6.39167683923873));
#29656=CARTESIAN_POINT('Ctrl Pts',(69.1491354609555,0.847191663528267,7.16419055056885));
#29657=CARTESIAN_POINT('Ctrl Pts',(69.2063596562406,-1.32739978994863,7.09093574623661));
#29658=CARTESIAN_POINT('Ctrl Pts',(69.2635838515257,-3.10974706736806,6.19644754492409));
#29659=CARTESIAN_POINT('Ctrl Pts',(69.3208080468108,-4.8920943447875,5.30195934361156));
#29660=CARTESIAN_POINT('Ctrl Pts',(69.3780322420959,-6.25040525059029,3.60219296582028));
#29661=CARTESIAN_POINT('Ctrl Pts',(69.435256437381,-6.72974280712937,1.66644854402722));
#29662=CARTESIAN_POINT('Ctrl Pts',(69.451353737052,-6.86458158035667,1.12191912096107));
#29663=CARTESIAN_POINT('Ctrl Pts',(69.4674510367229,-6.93300000000036,0.560975745772714));
#29664=CARTESIAN_POINT('Ctrl Pts',(69.4835483363939,-6.933,-4.40453229444415E-12));
#29665=CARTESIAN_POINT('Origin',(29.75,0.,0.));
#29666=CARTESIAN_POINT('',(70.9128916636062,-6.93600788003209,-0.00402363236026881));
#29667=CARTESIAN_POINT('',(70.7335483363939,-6.93748346162273,-0.00501519726878595));
#29668=CARTESIAN_POINT('',(29.75,-6.933,-8.4904762584886E-16));
#29669=CARTESIAN_POINT('Ctrl Pts',(70.9128916636062,-6.93600788003209,-0.00402363236026881));
#29670=CARTESIAN_POINT('Ctrl Pts',(70.8930998240354,-6.93185358698644,0.684973550004836));
#29671=CARTESIAN_POINT('Ctrl Pts',(70.8733079844645,-6.82435975372044,1.37546389076954));
#29672=CARTESIAN_POINT('Ctrl Pts',(70.8535161448936,-6.62104360085322,2.03665129400251));
#29673=CARTESIAN_POINT('Ctrl Pts',(70.8204308774865,-6.28116770090578,3.14193319383502));
#29674=CARTESIAN_POINT('Ctrl Pts',(70.7873456100795,-5.67352073095605,4.16532938092614));
#29675=CARTESIAN_POINT('Ctrl Pts',(70.7542603426724,-4.85002858812791,4.96638979919627));
#29676=CARTESIAN_POINT('Ctrl Pts',(70.6880898078583,-3.20304430247158,6.5685106357366));
#29677=CARTESIAN_POINT('Ctrl Pts',(70.6219192730444,-0.692679325301471,
7.28128839699305));
#29678=CARTESIAN_POINT('Ctrl Pts',(70.5557487382303,1.54387781336133,6.77133000678115));
#29679=CARTESIAN_POINT('Ctrl Pts',(70.4895782034163,3.7804349520242,6.26137161656925));
#29680=CARTESIAN_POINT('Ctrl Pts',(70.4234076686023,5.74318425217982,4.52867707488891));
#29681=CARTESIAN_POINT('Ctrl Pts',(70.3572371337882,6.52768685308951,2.37106409472671));
#29682=CARTESIAN_POINT('Ctrl Pts',(70.2910665989742,7.31218945399919,0.213451114564565));
#29683=CARTESIAN_POINT('Ctrl Pts',(70.2248960641602,6.91844535566313,-2.36908030407929));
#29684=CARTESIAN_POINT('Ctrl Pts',(70.1587255293462,5.53062392128402,-4.1977203057812));
#29685=CARTESIAN_POINT('Ctrl Pts',(70.0925549945321,4.1428024869049,-6.02636030748311));
#29686=CARTESIAN_POINT('Ctrl Pts',(70.026384459718,1.76090371648268,-7.10110889224293));
#29687=CARTESIAN_POINT('Ctrl Pts',(69.960213924904,-0.528348580108324,-6.92532263247645));
#29688=CARTESIAN_POINT('Ctrl Pts',(69.89404339009,-2.81760087669933,-6.74953637270997));
#29689=CARTESIAN_POINT('Ctrl Pts',(69.8278728552759,-5.0142066994592,-5.32321526841718));
#29690=CARTESIAN_POINT('Ctrl Pts',(69.7617023204619,-6.10668716247187,-3.30725649205025));
#29691=CARTESIAN_POINT('Ctrl Pts',(69.7287654348434,-6.65047759958824,-2.30379771972032));
#29692=CARTESIAN_POINT('Ctrl Pts',(69.6958285492248,-6.92070705183615,-1.15424877668268));
#29693=CARTESIAN_POINT('Ctrl Pts',(69.6628916636063,-6.91934367692504,-0.00345066477998368));
#29694=CARTESIAN_POINT('Ctrl Pts',(69.4835483363939,-6.91910824403556,0.00280665757405688));
#29695=CARTESIAN_POINT('Ctrl Pts',(69.5151159781859,-6.91929278287084,-1.10048129744765));
#29696=CARTESIAN_POINT('Ctrl Pts',(69.5466836199778,-6.67002846877592,-2.20446988795717));
#29697=CARTESIAN_POINT('Ctrl Pts',(69.5782512617697,-6.16970630690116,-3.18137335378403));
#29698=CARTESIAN_POINT('Ctrl Pts',(69.6113365291767,-5.64533097901331,-4.20524180144227));
#29699=CARTESIAN_POINT('Ctrl Pts',(69.6444217965837,-4.84517815766031,-5.08951207500788));
#29700=CARTESIAN_POINT('Ctrl Pts',(69.6775070639907,-3.88765338934523,-5.73617004499287));
#29701=CARTESIAN_POINT('Ctrl Pts',(69.7105923313977,-2.93012862103014,-6.38282801497786));
#29702=CARTESIAN_POINT('Ctrl Pts',(69.7436775988048,-1.81523190575297,-6.79187368138223));
#29703=CARTESIAN_POINT('Ctrl Pts',(69.7767628662118,-0.671317570116662,
-6.90316829378146));
#29704=CARTESIAN_POINT('Ctrl Pts',(69.8098481336188,0.472596765519775,-7.0144629061807));
#29705=CARTESIAN_POINT('Ctrl Pts',(69.8429334010258,1.64552872151536,-6.82800646457471));
#29706=CARTESIAN_POINT('Ctrl Pts',(69.8760186684328,2.70970252414811,-6.37785070657828));
#29707=CARTESIAN_POINT('Ctrl Pts',(69.9091039358398,3.77387632678074,-5.9276949485819));
#29708=CARTESIAN_POINT('Ctrl Pts',(69.9421892032469,4.72929197605057,-5.21383987419512));
#29709=CARTESIAN_POINT('Ctrl Pts',(69.9752744706539,5.44108660062344,-4.31016536153499));
#29710=CARTESIAN_POINT('Ctrl Pts',(70.0414450054679,6.86467584976921,-2.50281633621466));
#29711=CARTESIAN_POINT('Ctrl Pts',(70.1076155402819,7.3137810001271,0.0638104421991439));
#29712=CARTESIAN_POINT('Ctrl Pts',(70.173786075096,6.57541224839079,2.23462018433102));
#29713=CARTESIAN_POINT('Ctrl Pts',(70.23995660991,5.83704349665449,4.40542992646289));
#29714=CARTESIAN_POINT('Ctrl Pts',(70.3061271447241,3.91120084282398,6.18042263231284));
#29715=CARTESIAN_POINT('Ctrl Pts',(70.3722976795381,1.68399291891217,6.73820552039241));
#29716=CARTESIAN_POINT('Ctrl Pts',(70.4384682143522,-0.543215004999702,
7.29598840847199));
#29717=CARTESIAN_POINT('Ctrl Pts',(70.5046387491662,-3.0717881989929,6.63656147878113));
#29718=CARTESIAN_POINT('Ctrl Pts',(70.5708092839802,-4.74702605841882,5.06699124973978));
#29719=CARTESIAN_POINT('Ctrl Pts',(70.6250556347848,-6.12037963427992,3.780263592237));
#29720=CARTESIAN_POINT('Ctrl Pts',(70.6793019855893,-6.92023575397323,1.88185979080618));
#29721=CARTESIAN_POINT('Ctrl Pts',(70.7335483363939,-6.93748346162273,-0.00501519726878595));
#29722=CARTESIAN_POINT('Origin',(29.75,0.,0.));
#29723=CARTESIAN_POINT('',(72.1628916636062,-6.94192775449039,0.00618195413371575));
#29724=CARTESIAN_POINT('',(71.9835483363939,-6.9401949188535,0.00210382873980236));
#29725=CARTESIAN_POINT('',(29.75,-6.933,-8.4904762584886E-16));
#29726=CARTESIAN_POINT('Ctrl Pts',(72.1628916636062,-6.94192775449039,0.00618195413371575));
#29727=CARTESIAN_POINT('Ctrl Pts',(72.1565416336599,-6.94340649393155,0.226523173955462));
#29728=CARTESIAN_POINT('Ctrl Pts',(72.1501916037136,-6.93383229160786,0.446685249002146));
#29729=CARTESIAN_POINT('Ctrl Pts',(72.1438415737672,-6.91278923537634,0.665688012065615));
#29730=CARTESIAN_POINT('Ctrl Pts',(72.0776710389532,-6.69350990965197,2.94780795167749));
#29731=CARTESIAN_POINT('Ctrl Pts',(72.0115005041392,-5.22886240848834,5.10404170763851));
#29732=CARTESIAN_POINT('Ctrl Pts',(71.9453299693251,-3.18799897027634,6.16629140109333));
#29733=CARTESIAN_POINT('Ctrl Pts',(71.9122447019181,-2.16756725117023,6.69741624782081));
#29734=CARTESIAN_POINT('Ctrl Pts',(71.8791594345111,-1.00308154780201,6.95504507892165));
#29735=CARTESIAN_POINT('Ctrl Pts',(71.8460741671041,0.151959897059239,6.92780658346952));
#29736=CARTESIAN_POINT('Ctrl Pts',(71.8129888996971,1.30700134192036,6.90056808801738));
#29737=CARTESIAN_POINT('Ctrl Pts',(71.7799036322901,2.45259852827447,6.58846226601233));
#29738=CARTESIAN_POINT('Ctrl Pts',(71.7468183648831,3.4497814268547,6.01683565816965));
#29739=CARTESIAN_POINT('Ctrl Pts',(71.713733097476,4.44696432543494,5.44520905032697));
#29740=CARTESIAN_POINT('Ctrl Pts',(71.680647830069,5.29573293624125,4.61406165664668));
#29741=CARTESIAN_POINT('Ctrl Pts',(71.6475625626619,5.90256931486079,3.63083473489497));
#29742=CARTESIAN_POINT('Ctrl Pts',(71.6144772952549,6.50940569348037,2.64760781314321));
#29743=CARTESIAN_POINT('Ctrl Pts',(71.5813920278479,6.87430983991314,1.51230136332004));
#29744=CARTESIAN_POINT('Ctrl Pts',(71.5483067604409,6.93129030217091,0.363370212588453));
#29745=CARTESIAN_POINT('Ctrl Pts',(71.4821362256269,7.04525122668644,-1.93449208887466));
#29746=CARTESIAN_POINT('Ctrl Pts',(71.4159656908128,5.92751741450193,-4.28685319397145));
#29747=CARTESIAN_POINT('Ctrl Pts',(71.3497951559988,4.06794409821576,-5.62922334413628));
#29748=CARTESIAN_POINT('Ctrl Pts',(71.2836246211847,2.20837078192963,-6.97159349430107));
#29749=CARTESIAN_POINT('Ctrl Pts',(71.2174540863708,-0.393042038458098,
-7.30397268953411));
#29750=CARTESIAN_POINT('Ctrl Pts',(71.1512835515567,-2.53030427501,-6.46891859890768));
#29751=CARTESIAN_POINT('Ctrl Pts',(71.0851130167427,-4.66756651156202,-5.63386450828119));
#29752=CARTESIAN_POINT('Ctrl Pts',(71.0189424819285,-6.34067816427811,-3.63137713179512));
#29753=CARTESIAN_POINT('Ctrl Pts',(70.9527719471145,-6.8022422752566,-1.38099118953441));
#29754=CARTESIAN_POINT('Ctrl Pts',(70.9394785192785,-6.89496888262458,-0.928896564473384));
#29755=CARTESIAN_POINT('Ctrl Pts',(70.9261850914423,-6.9387981610777,-0.466796902638633));
#29756=CARTESIAN_POINT('Ctrl Pts',(70.9128916636062,-6.93600788003209,-0.00402363236026881));
#29757=CARTESIAN_POINT('Ctrl Pts',(70.7335483363939,-6.93748346162273,-0.00501519726878595));
#29758=CARTESIAN_POINT('Ctrl Pts',(70.7454725204034,-6.94127477360416,-0.419779402178013));
#29759=CARTESIAN_POINT('Ctrl Pts',(70.7573967044129,-6.90725137386348,-0.833986548478055));
#29760=CARTESIAN_POINT('Ctrl Pts',(70.7693208884224,-6.83319224883801,-1.24101743892661));
#29761=CARTESIAN_POINT('Ctrl Pts',(70.8354914232364,-6.42221805497271,-3.49974237015994));
#29762=CARTESIAN_POINT('Ctrl Pts',(70.9016619580505,-4.7783671423835,-5.53747870423487));
#29763=CARTESIAN_POINT('Ctrl Pts',(70.9678324928645,-2.65923204405885,-6.41583616523792));
#29764=CARTESIAN_POINT('Ctrl Pts',(71.0340030276785,-0.540096945734205,
-7.29419362624096));
#29765=CARTESIAN_POINT('Ctrl Pts',(71.1001735624925,2.05432233832609,-7.01317221417207));
#29766=CARTESIAN_POINT('Ctrl Pts',(71.1663440973065,3.94699624409178,-5.71043129652606));
#29767=CARTESIAN_POINT('Ctrl Pts',(71.1994293647136,4.89333319697466,-5.05906083770303));
#29768=CARTESIAN_POINT('Ctrl Pts',(71.2325146321206,5.66423380528383,-4.15226050248588));
#29769=CARTESIAN_POINT('Ctrl Pts',(71.2655998995276,6.18492037000725,-3.11976391325222));
#29770=CARTESIAN_POINT('Ctrl Pts',(71.2986851669347,6.70560693473067,-2.08726732401856));
#29771=CARTESIAN_POINT('Ctrl Pts',(71.3317704343417,6.9760794558682,-0.929074480768539));
#29772=CARTESIAN_POINT('Ctrl Pts',(71.3648557017487,6.9375587400496,0.218895786211316));
#29773=CARTESIAN_POINT('Ctrl Pts',(71.4310262365627,6.86051730841241,2.51483632017089));
#29774=CARTESIAN_POINT('Ctrl Pts',(71.4971967713767,5.5475029289509,4.76988654904982));
#29775=CARTESIAN_POINT('Ctrl Pts',(71.5633673061908,3.58085398574065,5.95204437955841));
#29776=CARTESIAN_POINT('Ctrl Pts',(71.6295378410048,1.61420504253036,7.13420221006703));
#29777=CARTESIAN_POINT('Ctrl Pts',(71.6957083758188,-1.00607846442871,7.24346764220525));
#29778=CARTESIAN_POINT('Ctrl Pts',(71.7618789106329,-3.06469476610544,6.23249313156326));
#29779=CARTESIAN_POINT('Ctrl Pts',(71.8280494454469,-5.12331106778224,5.22151862092123));
#29780=CARTESIAN_POINT('Ctrl Pts',(71.894219980261,-6.62026016417667,3.09030416749892));
#29781=CARTESIAN_POINT('Ctrl Pts',(71.960390515075,-6.89385797829254,0.80594375703103));
#29782=CARTESIAN_POINT('Ctrl Pts',(71.968109788848,-6.92577515165044,0.539456513818102));
#29783=CARTESIAN_POINT('Ctrl Pts',(71.9758290626209,-6.94104383768068,0.270885119828461));
#29784=CARTESIAN_POINT('Ctrl Pts',(71.9835483363939,-6.9401949188535,0.00210382873980236));
#29785=CARTESIAN_POINT('Origin',(29.75,0.,0.));
#29786=CARTESIAN_POINT('',(73.4128916636062,-6.92763786104848,9.47019909190297E-6));
#29787=CARTESIAN_POINT('',(73.2335483363939,-6.92837444992812,0.00246305386789827));
#29788=CARTESIAN_POINT('',(29.75,-6.933,-8.4904762584886E-16));
#29789=CARTESIAN_POINT('Ctrl Pts',(73.4128916636062,-6.92029165047812,2.2444507172259E-5));
#29790=CARTESIAN_POINT('Ctrl Pts',(73.3868981758774,-6.92413299961627,0.90830462489887));
#29791=CARTESIAN_POINT('Ctrl Pts',(73.3609046881487,-6.75800402829825,1.81602407914437));
#29792=CARTESIAN_POINT('Ctrl Pts',(73.3349112004199,-6.41502137678869,2.65215700470205));
#29793=CARTESIAN_POINT('Ctrl Pts',(73.3018259330129,-5.97846307958873,3.71641131788004));
#29794=CARTESIAN_POINT('Ctrl Pts',(73.2687406656059,-5.25538521396701,4.66468873262861));
#29795=CARTESIAN_POINT('Ctrl Pts',(73.2356553981989,-4.35552620310463,5.38949129071545));
#29796=CARTESIAN_POINT('Ctrl Pts',(73.2025701307919,-3.4556671922422,6.11429384880233));
#29797=CARTESIAN_POINT('Ctrl Pts',(73.1694848633848,-2.37902703613907,6.61562155022746));
#29798=CARTESIAN_POINT('Ctrl Pts',(73.1363995959778,-1.24850598774616,6.82250488956186));
#29799=CARTESIAN_POINT('Ctrl Pts',(73.1033143285708,-0.117984939353238,
7.02938822889626));
#29800=CARTESIAN_POINT('Ctrl Pts',(73.0702290611638,1.06641700132947,6.94182720613994));
#29801=CARTESIAN_POINT('Ctrl Pts',(73.0371437937568,2.16463905450583,6.58267021332574));
#29802=CARTESIAN_POINT('Ctrl Pts',(73.0040585263498,3.26286110768207,6.22351322051157));
#29803=CARTESIAN_POINT('Ctrl Pts',(72.9709732589427,4.27490327335198,5.59276025763959));
#29804=CARTESIAN_POINT('Ctrl Pts',(72.9378879915357,5.06006237968395,4.75207816740074));
#29805=CARTESIAN_POINT('Ctrl Pts',(72.8717174567216,6.63038059234808,3.07071398692286));
#29806=CARTESIAN_POINT('Ctrl Pts',(72.8055469219076,7.29316656766025,0.549633296977299));
#29807=CARTESIAN_POINT('Ctrl Pts',(72.7393763870936,6.73971393441234,-1.67520577327393));
#29808=CARTESIAN_POINT('Ctrl Pts',(72.6732058522796,6.18626130116446,-3.90004484352504));
#29809=CARTESIAN_POINT('Ctrl Pts',(72.6070353174655,4.41657005935665,-5.82864229408185));
#29810=CARTESIAN_POINT('Ctrl Pts',(72.5408647826515,2.24392949191622,-6.57214175759916));
#29811=CARTESIAN_POINT('Ctrl Pts',(72.4746942478375,0.0712889244756562,
-7.31564122111651));
#29812=CARTESIAN_POINT('Ctrl Pts',(72.4085237130234,-2.50430096859759,-6.87404269759419));
#29813=CARTESIAN_POINT('Ctrl Pts',(72.3423531782093,-4.3051403399917,-5.44924037420161));
#29814=CARTESIAN_POINT('Ctrl Pts',(72.2825326733416,-5.93316285311149,-4.16116865827016));
#29815=CARTESIAN_POINT('Ctrl Pts',(72.2227121684739,-6.92799727846338,-2.06954416437256));
#29816=CARTESIAN_POINT('Ctrl Pts',(72.1628916636062,-6.94192775449039,0.00618195413371575));
#29817=CARTESIAN_POINT('Ctrl Pts',(71.9835483363939,-6.9401949188535,0.00210382873980236));
#29818=CARTESIAN_POINT('Ctrl Pts',(72.0089143300279,-6.93740532099759,-0.881127511310418));
#29819=CARTESIAN_POINT('Ctrl Pts',(72.0342803236619,-6.76057480142328,-1.76662535962301));
#29820=CARTESIAN_POINT('Ctrl Pts',(72.059646317296,-6.42854092195365,-2.58788465809884));
#29821=CARTESIAN_POINT('Ctrl Pts',(72.092731584703,-5.99546387206851,-3.65906617349956));
#29822=CARTESIAN_POINT('Ctrl Pts',(72.1258168521101,-5.2983486858099,-4.62096250980574));
#29823=CARTESIAN_POINT('Ctrl Pts',(72.1589021195171,-4.41133942826932,-5.35195176352421));
#29824=CARTESIAN_POINT('Ctrl Pts',(72.1919873869242,-3.52433017072873,-6.08294101724269));
#29825=CARTESIAN_POINT('Ctrl Pts',(72.2250726543312,-2.44742684190618,-6.58302318837345));
#29826=CARTESIAN_POINT('Ctrl Pts',(72.2581579217382,-1.31336822550145,-6.80387094031927));
#29827=CARTESIAN_POINT('Ctrl Pts',(72.2912431891452,-0.179309609096652,
-7.0247186922651));
#29828=CARTESIAN_POINT('Ctrl Pts',(72.3243284565522,1.01190429489034,-6.96633202502595));
#29829=CARTESIAN_POINT('Ctrl Pts',(72.3574137239592,2.10704588485406,-6.61413975637045));
#29830=CARTESIAN_POINT('Ctrl Pts',(72.4235842587733,4.29732906478144,-5.90975521905948));
#29831=CARTESIAN_POINT('Ctrl Pts',(72.4897547935873,6.10332298861579,-4.0301482760832));
#29832=CARTESIAN_POINT('Ctrl Pts',(72.5559253284013,6.70278317878333,-1.81727631370743));
#29833=CARTESIAN_POINT('Ctrl Pts',(72.6220958632153,7.30224336895088,0.395595648668328));
#29834=CARTESIAN_POINT('Ctrl Pts',(72.6882663980294,6.69516982545161,2.94173263044357));
#29835=CARTESIAN_POINT('Ctrl Pts',(72.7544369328434,5.15921646832352,4.64875676238626));
#29836=CARTESIAN_POINT('Ctrl Pts',(72.8206074676575,3.62326311119548,6.3557808943289));
#29837=CARTESIAN_POINT('Ctrl Pts',(72.8867780024715,1.15842994043866,7.22369217643902));
#29838=CARTESIAN_POINT('Ctrl Pts',(72.9529485372855,-1.10822237865247,6.8556626234175));
#29839=CARTESIAN_POINT('Ctrl Pts',(73.0191190720996,-3.37487469774379,6.48763307039594));
#29840=CARTESIAN_POINT('Ctrl Pts',(73.0852896069136,-5.44334616516939,4.88366268224249));
#29841=CARTESIAN_POINT('Ctrl Pts',(73.1514601417277,-6.36261189066002,2.78338431219154));
#29842=CARTESIAN_POINT('Ctrl Pts',(73.1788228732831,-6.74274515307623,1.91488062859826));
#29843=CARTESIAN_POINT('Ctrl Pts',(73.2061856048385,-6.9263671749664,0.961509550380373));
#29844=CARTESIAN_POINT('Ctrl Pts',(73.2335483363939,-6.92150572898554,0.00612057123355675));
#29845=CARTESIAN_POINT('Origin',(29.75,0.,0.));
#29846=CARTESIAN_POINT('',(74.6628916636063,-6.93302851199415,-6.57016384422878E-5));
#29847=CARTESIAN_POINT('',(74.4835483363939,-6.93138337985325,-0.00328068813936701));
#29848=CARTESIAN_POINT('',(29.75,-6.933,-8.4904762584886E-16));
#29849=CARTESIAN_POINT('Ctrl Pts',(74.6628916636062,-6.933,1.47798440153224E-12));
#29850=CARTESIAN_POINT('Ctrl Pts',(74.6056674683211,-6.93299999999958,1.99420935701776));
#29851=CARTESIAN_POINT('Ctrl Pts',(74.548443273036,-6.02307502629165,3.97063309653173));
#29852=CARTESIAN_POINT('Ctrl Pts',(74.491219077751,-4.50798484753872,5.2673106624122));
#29853=CARTESIAN_POINT('Ctrl Pts',(74.4339948824659,-2.9928946687858,6.56398822829268));
#29854=CARTESIAN_POINT('Ctrl Pts',(74.3767706871808,-0.89966434562727,7.15779044292429));
#29855=CARTESIAN_POINT('Ctrl Pts',(74.3195464918957,1.07062371681991,6.84983604599283));
#29856=CARTESIAN_POINT('Ctrl Pts',(74.2623222966106,3.04091177926709,6.54188164906137));
#29857=CARTESIAN_POINT('Ctrl Pts',(74.2050981013255,4.85311303639994,5.33766370386297));
#29858=CARTESIAN_POINT('Ctrl Pts',(74.1478739060404,5.90026971493839,3.64050907030609));
#29859=CARTESIAN_POINT('Ctrl Pts',(74.0906497107553,6.94742639347683,1.9433544367492));
#29860=CARTESIAN_POINT('Ctrl Pts',(74.0334255154702,7.21086008527505,-0.216464293125449));
#29861=CARTESIAN_POINT('Ctrl Pts',(73.9762013201851,6.60233935006037,-2.11556236179517));
#29862=CARTESIAN_POINT('Ctrl Pts',(73.9189771249,5.99381861484569,-4.01466043046489));
#29863=CARTESIAN_POINT('Ctrl Pts',(73.8617529296149,4.52419779647178,-5.61916312790536));
#29864=CARTESIAN_POINT('Ctrl Pts',(73.8045287343298,2.68569473000269,-6.39167683923677));
#29865=CARTESIAN_POINT('Ctrl Pts',(73.7473045390447,0.847191663533602,-7.16419055056818));
#29866=CARTESIAN_POINT('Ctrl Pts',(73.6900803437596,-1.32739978994318,-7.09093574623759));
#29867=CARTESIAN_POINT('Ctrl Pts',(73.6328561484745,-3.1097470673632,-6.19644754492653));
#29868=CARTESIAN_POINT('Ctrl Pts',(73.5756319531894,-4.89209434478322,-5.30195934361546));
#29869=CARTESIAN_POINT('Ctrl Pts',(73.5184077579043,-6.25040525058729,-3.60219296582541));
#29870=CARTESIAN_POINT('Ctrl Pts',(73.4611835626192,-6.72974280712797,-1.66644854403288));
#29871=CARTESIAN_POINT('Ctrl Pts',(73.4450862629482,-6.86458158035597,-1.12191912096589));
#29872=CARTESIAN_POINT('Ctrl Pts',(73.4289889632772,-6.93300000000012,-0.560975745776578));
#29873=CARTESIAN_POINT('Ctrl Pts',(73.4128916636062,-6.933,1.52572399159112E-12));
#29874=CARTESIAN_POINT('Ctrl Pts',(73.2335483363939,-6.933,-4.15320555724463E-12));
#29875=CARTESIAN_POINT('Ctrl Pts',(73.290772531679,-6.93299999999881,-1.99420935702036));
#29876=CARTESIAN_POINT('Ctrl Pts',(73.3479967269641,-6.02307502629018,-3.97063309653393));
#29877=CARTESIAN_POINT('Ctrl Pts',(73.4052209222492,-4.50798484753684,-5.26731066241381));
#29878=CARTESIAN_POINT('Ctrl Pts',(73.4624451175343,-2.9928946687835,-6.5639882282937));
#29879=CARTESIAN_POINT('Ctrl Pts',(73.5196693128193,-0.89966434562485,-7.15779044292458));
#29880=CARTESIAN_POINT('Ctrl Pts',(73.5768935081044,1.07062371682216,-6.84983604599248));
#29881=CARTESIAN_POINT('Ctrl Pts',(73.6341177033895,3.04091177926917,-6.54188164906038));
#29882=CARTESIAN_POINT('Ctrl Pts',(73.6913418986746,4.85311303640158,-5.33766370386146));
#29883=CARTESIAN_POINT('Ctrl Pts',(73.7485660939597,5.90026971493948,-3.64050907030431));
#29884=CARTESIAN_POINT('Ctrl Pts',(73.8057902892448,6.94742639347738,-1.94335443674717));
#29885=CARTESIAN_POINT('Ctrl Pts',(73.8630144845299,7.21086008527498,0.216464293127474));
#29886=CARTESIAN_POINT('Ctrl Pts',(73.920238679815,6.6023393500598,2.11556236179696));
#29887=CARTESIAN_POINT('Ctrl Pts',(73.9774628751001,5.99381861484462,4.01466043046646));
#29888=CARTESIAN_POINT('Ctrl Pts',(74.0346870703852,4.52419779647035,5.61916312790649));
#29889=CARTESIAN_POINT('Ctrl Pts',(74.0919112656703,2.68569473000113,6.39167683923743));
#29890=CARTESIAN_POINT('Ctrl Pts',(74.1491354609554,0.847191663531917,7.16419055056836));
#29891=CARTESIAN_POINT('Ctrl Pts',(74.2063596562405,-1.32739978994477,7.09093574623728));
#29892=CARTESIAN_POINT('Ctrl Pts',(74.2635838515256,-3.10974706736454,6.19644754492586));
#29893=CARTESIAN_POINT('Ctrl Pts',(74.3208080468107,-4.89209434478431,5.30195934361443));
#29894=CARTESIAN_POINT('Ctrl Pts',(74.3780322420958,-6.25040525058798,3.60219296582418));
#29895=CARTESIAN_POINT('Ctrl Pts',(74.4352564373808,-6.72974280712828,1.66644854403162));
#29896=CARTESIAN_POINT('Ctrl Pts',(74.4513537370519,-6.86458158035629,1.12191912096416));
#29897=CARTESIAN_POINT('Ctrl Pts',(74.4674510367229,-6.93300000000034,0.560975745774362));
#29898=CARTESIAN_POINT('Ctrl Pts',(74.4835483363939,-6.933,-4.20066759154736E-12));
#29899=CARTESIAN_POINT('Origin',(29.75,0.,0.));
#29900=CARTESIAN_POINT('',(75.9128916636063,-6.93577247332454,-0.000335286187928552));
#29901=CARTESIAN_POINT('',(75.7335483363939,-6.94460482329128,0.000883125311795762));
#29902=CARTESIAN_POINT('',(29.75,-6.933,-8.4904762584886E-16));
#29903=CARTESIAN_POINT('Ctrl Pts',(75.9128916636063,-6.93577247332454,-0.000335286187928552));
#29904=CARTESIAN_POINT('Ctrl Pts',(75.8806965277196,-6.93514425451495,1.1180543323845));
#29905=CARTESIAN_POINT('Ctrl Pts',(75.8485013918329,-6.65226718410521,2.23682721397932));
#29906=CARTESIAN_POINT('Ctrl Pts',(75.8163062559463,-6.12942454003317,3.23224042168337));
#29907=CARTESIAN_POINT('Ctrl Pts',(75.7832209885393,-5.59212633598693,4.25517482622593));
#29908=CARTESIAN_POINT('Ctrl Pts',(75.7501357211323,-4.80140998319663,5.14783395957035));
#29909=CARTESIAN_POINT('Ctrl Pts',(75.7170504537253,-3.84154731235279,5.78177750999706));
#29910=CARTESIAN_POINT('Ctrl Pts',(75.6508799189113,-1.92182197066505,7.04966461085053));
#29911=CARTESIAN_POINT('Ctrl Pts',(75.5847093840972,0.674488643236908,7.28268938003312));
#29912=CARTESIAN_POINT('Ctrl Pts',(75.5185388492831,2.77585362956056,6.36590612130795));
#29913=CARTESIAN_POINT('Ctrl Pts',(75.4523683144691,4.87721861588421,5.44912286258278));
#29914=CARTESIAN_POINT('Ctrl Pts',(75.3861977796551,6.48363797462955,3.38253157594985));
#29915=CARTESIAN_POINT('Ctrl Pts',(75.320027244841,6.85434798412124,1.11632363563946));
#29916=CARTESIAN_POINT('Ctrl Pts',(75.253856710027,7.22505799361293,-1.14988430467093));
#29917=CARTESIAN_POINT('Ctrl Pts',(75.187686175213,6.36005865385096,-3.61570889865878));
#29918=CARTESIAN_POINT('Ctrl Pts',(75.1215156403989,4.65485526475585,-5.15369646059015));
#29919=CARTESIAN_POINT('Ctrl Pts',(75.0553451055849,2.94965187566074,-6.69168402252151));
#29920=CARTESIAN_POINT('Ctrl Pts',(74.9891745707708,0.404244437232484,-7.3018345523964));
#29921=CARTESIAN_POINT('Ctrl Pts',(74.9230040359568,-1.80934090928194,-6.70495410796962));
#29922=CARTESIAN_POINT('Ctrl Pts',(74.8568335011428,-4.02292625579636,-6.10807366354283));
#29923=CARTESIAN_POINT('Ctrl Pts',(74.7906629663288,-5.90468951039696,-4.30416224481439));
#29924=CARTESIAN_POINT('Ctrl Pts',(74.7244924315147,-6.61164537146094,-2.11484808314536));
#29925=CARTESIAN_POINT('Ctrl Pts',(74.7039588422119,-6.83102309520318,-1.43547503626127));
#29926=CARTESIAN_POINT('Ctrl Pts',(74.6834252529091,-6.93727359651782,-0.71898991290854));
#29927=CARTESIAN_POINT('Ctrl Pts',(74.6628916636062,-6.93384748847811,-0.00195291085134108));
#29928=CARTESIAN_POINT('Ctrl Pts',(74.4835483363939,-6.92866114138664,-0.00880506282216201));
#29929=CARTESIAN_POINT('Ctrl Pts',(74.5027126818701,-6.93434561264149,-0.677464884404123));
#29930=CARTESIAN_POINT('Ctrl Pts',(74.5218770273463,-6.84558152848312,-1.34433981842437));
#29931=CARTESIAN_POINT('Ctrl Pts',(74.5410413728224,-6.65631914950611,-1.98079271750886));
#29932=CARTESIAN_POINT('Ctrl Pts',(74.6072119076365,-6.00283516526842,-4.17833339369304));
#29933=CARTESIAN_POINT('Ctrl Pts',(74.6733824424504,-4.15123205783588,-6.01318909209914));
#29934=CARTESIAN_POINT('Ctrl Pts',(74.7395529772645,-1.94449844419176,-6.66373488795828));
#29935=CARTESIAN_POINT('Ctrl Pts',(74.7726382446716,-0.841131637369642,
-6.98900778588786));
#29936=CARTESIAN_POINT('Ctrl Pts',(74.8057235120786,0.351017796005385,-7.01820320818067));
#29937=CARTESIAN_POINT('Ctrl Pts',(74.8388087794856,1.47943176153331,-6.7696753978216));
#29938=CARTESIAN_POINT('Ctrl Pts',(74.8718940468926,2.60784572706124,-6.52114758746254));
#29939=CARTESIAN_POINT('Ctrl Pts',(74.9049793142996,3.67252422474206,-5.99489654445161));
#29940=CARTESIAN_POINT('Ctrl Pts',(74.9380645817066,4.54121424326715,-5.24239563710084));
#29941=CARTESIAN_POINT('Ctrl Pts',(74.9711498491136,5.40990426179223,-4.48989472975007));
#29942=CARTESIAN_POINT('Ctrl Pts',(75.0042351165207,6.08260580116156,-3.51114395805947));
#29943=CARTESIAN_POINT('Ctrl Pts',(75.0373203839277,6.4895115820401,-2.42970425104458));
#29944=CARTESIAN_POINT('Ctrl Pts',(75.0704056513348,6.89641736291859,-1.34826454402982));
#29945=CARTESIAN_POINT('Ctrl Pts',(75.1034909187418,7.03752738530635,-0.1641359016908));
#29946=CARTESIAN_POINT('Ctrl Pts',(75.1365761861488,6.87292506515188,0.974339766996876));
#29947=CARTESIAN_POINT('Ctrl Pts',(75.2027467209628,6.5437204248429,3.25129110437249));
#29948=CARTESIAN_POINT('Ctrl Pts',(75.2689172557769,4.99166641436471,5.34563054714267));
#29949=CARTESIAN_POINT('Ctrl Pts',(75.3350877905909,2.90977586653595,6.3058170384578));
#29950=CARTESIAN_POINT('Ctrl Pts',(75.4012583254049,0.827885318707192,7.26600352977293));
#29951=CARTESIAN_POINT('Ctrl Pts',(75.467428860219,-1.78384176647215,7.09203706963299));
#29952=CARTESIAN_POINT('Ctrl Pts',(75.533599395033,-3.72313617215261,5.86229663078674));
#29953=CARTESIAN_POINT('Ctrl Pts',(75.599769929847,-5.66243057783302,4.63255619194052));
#29954=CARTESIAN_POINT('Ctrl Pts',(75.6659404646611,-6.9292923040146,2.34704177438805));
#29955=CARTESIAN_POINT('Ctrl Pts',(75.7321109994751,-6.94447174479279,0.0507634976017025));
#29956=CARTESIAN_POINT('Ctrl Pts',(75.7325901117814,-6.94458165257726,0.03413713687956));
#29957=CARTESIAN_POINT('Ctrl Pts',(75.7330692240876,-6.94462593987182,0.0175102118531011));
#29958=CARTESIAN_POINT('Ctrl Pts',(75.7335483363939,-6.94460482329128,0.000883125311795762));
#29959=CARTESIAN_POINT('Origin',(29.75,0.,0.));
#29960=CARTESIAN_POINT('',(77.1628916636062,-6.933,1.77691195091256E-12));
#29961=CARTESIAN_POINT('',(76.9835483363939,-6.9297498061854,0.00533558548810259));
#29962=CARTESIAN_POINT('',(29.75,-6.933,-8.4904762584886E-16));
#29963=CARTESIAN_POINT('Ctrl Pts',(77.1628916636062,-6.93482283397445,0.00227082123790745));
#29964=CARTESIAN_POINT('Ctrl Pts',(77.1441383373442,-6.93813353830398,0.656949323559923));
#29965=CARTESIAN_POINT('Ctrl Pts',(77.1253850110821,-6.84966132346527,1.31098698841223));
#29966=CARTESIAN_POINT('Ctrl Pts',(77.10663168482,-6.6660308597263,1.93661289511069));
#29967=CARTESIAN_POINT('Ctrl Pts',(77.040461150006,-6.01809641737947,4.14411466099759));
#29968=CARTESIAN_POINT('Ctrl Pts',(76.974290615192,-4.18543272105473,5.99788733423284));
#29969=CARTESIAN_POINT('Ctrl Pts',(76.908120080378,-1.98866675453222,6.65397089400068));
#29970=CARTESIAN_POINT('Ctrl Pts',(76.8419495455639,0.208099211990228,7.31005445376851));
#29971=CARTESIAN_POINT('Ctrl Pts',(76.7757790107498,2.76896744871042,6.76844890006899));
#29972=CARTESIAN_POINT('Ctrl Pts',(76.7096084759358,4.51483985655232,5.27678745211015));
#29973=CARTESIAN_POINT('Ctrl Pts',(76.6434379411217,6.26071226439422,3.7851260041513));
#29974=CARTESIAN_POINT('Ctrl Pts',(76.5772674063078,7.19158884335782,1.34340866193312));
#29975=CARTESIAN_POINT('Ctrl Pts',(76.5110968714937,6.88184311853839,-0.931933493819985));
#29976=CARTESIAN_POINT('Ctrl Pts',(76.4449263366797,6.57209739371898,-3.20727564957302));
#29977=CARTESIAN_POINT('Ctrl Pts',(76.3787558018656,5.0217293651166,-5.31624261886099));
#29978=CARTESIAN_POINT('Ctrl Pts',(76.3125852670516,2.94573031687968,-6.28910144766352));
#29979=CARTESIAN_POINT('Ctrl Pts',(76.2464147322375,0.869731268642629,-7.2619602764661));
#29980=CARTESIAN_POINT('Ctrl Pts',(76.1802441974236,-1.73189879922904,-7.09871096478309));
#29981=CARTESIAN_POINT('Ctrl Pts',(76.1140736626095,-3.68496568754885,-5.88281096159864));
#29982=CARTESIAN_POINT('Ctrl Pts',(76.0809883952025,-4.66149913170876,-5.27486096000641));
#29983=CARTESIAN_POINT('Ctrl Pts',(76.0479031277954,-5.4758917809807,-4.40374828553883));
#29984=CARTESIAN_POINT('Ctrl Pts',(76.0148178603884,-6.04045450968852,-3.39560490218326));
#29985=CARTESIAN_POINT('Ctrl Pts',(75.9817325929814,-6.60501723839632,-2.38746151882774));
#29986=CARTESIAN_POINT('Ctrl Pts',(75.9486473255744,-6.91975004654002,-1.24228742658426));
#29987=CARTESIAN_POINT('Ctrl Pts',(75.9155620581674,-6.93517642296081,-0.0930955425921683));
#29988=CARTESIAN_POINT('Ctrl Pts',(75.914671926647,-6.93559145674997,-0.062177493591001));
#29989=CARTESIAN_POINT('Ctrl Pts',(75.9137817951266,-6.93578984232606,-0.0312565363750059));
#29990=CARTESIAN_POINT('Ctrl Pts',(75.9128916636063,-6.93577247332454,-0.000335286187928552));
#29991=CARTESIAN_POINT('Ctrl Pts',(75.7335483363939,-6.94460482329128,0.000883125311795762));
#29992=CARTESIAN_POINT('Ctrl Pts',(75.7992397589017,-6.94170951420419,-2.27886830832412));
#29993=CARTESIAN_POINT('Ctrl Pts',(75.8649311814095,-5.70926429895426,-4.56165611502022));
#29994=CARTESIAN_POINT('Ctrl Pts',(75.9306226039173,-3.8056136169074,-5.80925374870641));
#29995=CARTESIAN_POINT('Ctrl Pts',(75.9967931387313,-1.88807889286908,-7.06595058220794));
#29996=CARTESIAN_POINT('Ctrl Pts',(76.0629636735453,0.710487710582319,-7.27230211319087));
#29997=CARTESIAN_POINT('Ctrl Pts',(76.1291342083593,2.81589166875497,-6.34485547810106));
#29998=CARTESIAN_POINT('Ctrl Pts',(76.1622194757663,3.86859364784136,-5.88113216055613));
#29999=CARTESIAN_POINT('Ctrl Pts',(76.1953047431734,4.79800496560802,-5.133959301493));
#30000=CARTESIAN_POINT('Ctrl Pts',(76.2283900105804,5.49947858928678,-4.21579868844575));
#30001=CARTESIAN_POINT('Ctrl Pts',(76.2614752779874,6.20095221296551,-3.29763807539856));
#30002=CARTESIAN_POINT('Ctrl Pts',(76.2945605453944,6.67448814255641,-2.20848970836712));
#30003=CARTESIAN_POINT('Ctrl Pts',(76.3276458128014,6.85229462999235,-1.0730317336501));
#30004=CARTESIAN_POINT('Ctrl Pts',(76.3607310802085,7.03010111742829,0.0624262410669793));
#30005=CARTESIAN_POINT('Ctrl Pts',(76.3938163476155,6.91217816270932,1.2441938234698));
#30006=CARTESIAN_POINT('Ctrl Pts',(76.4269016150226,6.52495911412754,2.3328377342437));
#30007=CARTESIAN_POINT('Ctrl Pts',(76.4599868824296,6.13774006554577,3.4214816450176));
#30008=CARTESIAN_POINT('Ctrl Pts',(76.4930721498366,5.48122492310122,4.41700188416254));
#30009=CARTESIAN_POINT('Ctrl Pts',(76.5261574172436,4.62067251741759,5.18033033841466));
#30010=CARTESIAN_POINT('Ctrl Pts',(76.5923279520576,2.89956770605038,6.70698724691885));
#30011=CARTESIAN_POINT('Ctrl Pts',(76.6584984868717,0.362313841727035,7.30487701585175));
#30012=CARTESIAN_POINT('Ctrl Pts',(76.7246690216857,-1.84759209267133,6.69451473804381));
#30013=CARTESIAN_POINT('Ctrl Pts',(76.7908395564998,-4.05749802706964,6.08415246023589));
#30014=CARTESIAN_POINT('Ctrl Pts',(76.8570100913138,-5.94005603154293,4.26553813568725));
#30015=CARTESIAN_POINT('Ctrl Pts',(76.9231806261278,-6.62755912924991,2.07454205389382));
#30016=CARTESIAN_POINT('Ctrl Pts',(76.9433031962165,-6.83662996884164,1.40825648821338));
#30017=CARTESIAN_POINT('Ctrl Pts',(76.9634257663052,-6.93518472965,0.707533867475353));
#30018=CARTESIAN_POINT('Ctrl Pts',(76.9835483363939,-6.9297498061854,0.00533558548810259));
#30019=CARTESIAN_POINT('Origin',(29.75,0.,0.));
#30020=CARTESIAN_POINT('',(78.4128916636062,-6.92804963575093,0.000312599262795181));
#30021=CARTESIAN_POINT('',(78.2335483363939,-6.92245089085948,-0.0021973978771043));
#30022=CARTESIAN_POINT('',(29.75,-6.933,-8.4904762584886E-16));
#30023=CARTESIAN_POINT('Ctrl Pts',(78.4128916636062,-6.933,1.9265145034808E-12));
#30024=CARTESIAN_POINT('Ctrl Pts',(78.3556674683211,-6.93299999999945,1.99420935701807));
#30025=CARTESIAN_POINT('Ctrl Pts',(78.298443273036,-6.02307502629152,3.97063309653186));
#30026=CARTESIAN_POINT('Ctrl Pts',(78.241219077751,-4.50798484753868,5.26731066241224));
#30027=CARTESIAN_POINT('Ctrl Pts',(78.1839948824659,-2.99289466878585,6.56398822829261));
#30028=CARTESIAN_POINT('Ctrl Pts',(78.1267706871808,-0.899664345627491,
7.15779044292423));
#30029=CARTESIAN_POINT('Ctrl Pts',(78.0695464918957,1.07062371681957,6.84983604599289));
#30030=CARTESIAN_POINT('Ctrl Pts',(78.0123222966106,3.04091177926664,6.54188164906155));
#30031=CARTESIAN_POINT('Ctrl Pts',(77.9550981013255,4.85311303639945,5.33766370386337));
#30032=CARTESIAN_POINT('Ctrl Pts',(77.8978739060404,5.900269714938,3.64050907030671));
#30033=CARTESIAN_POINT('Ctrl Pts',(77.8406497107553,6.94742639347656,1.94335443675005));
#30034=CARTESIAN_POINT('Ctrl Pts',(77.7834255154702,7.21086008527505,-0.2164642931244));
#30035=CARTESIAN_POINT('Ctrl Pts',(77.7262013201851,6.60233935006072,-2.11556236179409));
#30036=CARTESIAN_POINT('Ctrl Pts',(77.6689771249,5.99381861484639,-4.01466043046379));
#30037=CARTESIAN_POINT('Ctrl Pts',(77.611752929615,4.52419779647289,-5.61916312790442));
#30038=CARTESIAN_POINT('Ctrl Pts',(77.5545287343298,2.68569473000409,-6.39167683923618));
#30039=CARTESIAN_POINT('Ctrl Pts',(77.4973045390448,0.847191663535296,-7.16419055056795));
#30040=CARTESIAN_POINT('Ctrl Pts',(77.4400803437597,-1.32739978994134,-7.0909357462379));
#30041=CARTESIAN_POINT('Ctrl Pts',(77.3828561484746,-3.10974706736149,-6.19644754492739));
#30042=CARTESIAN_POINT('Ctrl Pts',(77.3256319531895,-4.89209434478164,-5.30195934361687));
#30043=CARTESIAN_POINT('Ctrl Pts',(77.2684077579044,-6.25040525058613,-3.60219296582736));
#30044=CARTESIAN_POINT('Ctrl Pts',(77.2111835626193,-6.72974280712742,-1.66644854403513));
#30045=CARTESIAN_POINT('Ctrl Pts',(77.1950862629483,-6.8645815803558,-1.12191912096735));
#30046=CARTESIAN_POINT('Ctrl Pts',(77.1789889632773,-6.93300000000014,-0.56097574577718));
#30047=CARTESIAN_POINT('Ctrl Pts',(77.1628916636062,-6.933,1.77691195091256E-12));
#30048=CARTESIAN_POINT('Ctrl Pts',(76.9835483363939,-6.9297498061854,0.00533558548810259));
#30049=CARTESIAN_POINT('Ctrl Pts',(77.0295963011192,-6.91731266903644,-1.60155665425157));
#30050=CARTESIAN_POINT('Ctrl Pts',(77.0756442658446,-6.36031740813025,-3.21617642318602));
#30051=CARTESIAN_POINT('Ctrl Pts',(77.1216922305699,-5.33697258446145,-4.4435333213297));
#30052=CARTESIAN_POINT('Ctrl Pts',(77.1878627653839,-3.86643475102544,-6.20723477572147));
#30053=CARTESIAN_POINT('Ctrl Pts',(77.254033300198,-1.43291089321261,-7.1712598454668));
#30054=CARTESIAN_POINT('Ctrl Pts',(77.320203835012,0.842842081745409,-6.89345641489297));
#30055=CARTESIAN_POINT('Ctrl Pts',(77.3863743698261,3.11859505670343,-6.61565298431915));
#30056=CARTESIAN_POINT('Ctrl Pts',(77.4525449046401,5.23657714880673,-5.09602105342644));
#30057=CARTESIAN_POINT('Ctrl Pts',(77.5187154394541,6.24607061556865,-3.02870249342226));
#30058=CARTESIAN_POINT('Ctrl Pts',(77.5518007068611,6.75081734894962,-1.99504321342014));
#30059=CARTESIAN_POINT('Ctrl Pts',(77.5848859742681,6.97844192599519,-0.824462276140171));
#30060=CARTESIAN_POINT('Ctrl Pts',(77.6179712416751,6.92160306263817,0.329597297566678));
#30061=CARTESIAN_POINT('Ctrl Pts',(77.6510565090822,6.86476419928114,1.48365687127346));
#30062=CARTESIAN_POINT('Ctrl Pts',(77.6841417764892,6.52346189552155,2.62119508140712));
#30063=CARTESIAN_POINT('Ctrl Pts',(77.7172270438963,5.92639008272138,3.60322624674164));
#30064=CARTESIAN_POINT('Ctrl Pts',(77.7503123113033,5.32931826992122,4.58525741207615));
#30065=CARTESIAN_POINT('Ctrl Pts',(77.7833975787103,4.47647694808047,5.41178153261152));
#30066=CARTESIAN_POINT('Ctrl Pts',(77.8164828461173,3.47805314064643,5.99336046689384));
#30067=CARTESIAN_POINT('Ctrl Pts',(77.8495681135243,2.47962933321233,6.5749394011762));
#30068=CARTESIAN_POINT('Ctrl Pts',(77.8826533809313,1.33562304018492,6.91157314920548));
#30069=CARTESIAN_POINT('Ctrl Pts',(77.9157386483383,0.18564060271005,6.93916237704205));
#30070=CARTESIAN_POINT('Ctrl Pts',(77.9819091831524,-2.11432427223969,6.99434083271517));
#30071=CARTESIAN_POINT('Ctrl Pts',(78.0480797179665,-4.4381937249793,5.81334120761742));
#30072=CARTESIAN_POINT('Ctrl Pts',(78.1142502527805,-5.73216807578779,3.92076182261932));
#30073=CARTESIAN_POINT('Ctrl Pts',(78.1540162806516,-6.50979848550715,2.7833920736263));
#30074=CARTESIAN_POINT('Ctrl Pts',(78.1937823085228,-6.91547584179783,1.38903084661121));
#30075=CARTESIAN_POINT('Ctrl Pts',(78.2335483363939,-6.92245089085948,-0.0021973978771043));
#30076=CARTESIAN_POINT('Origin',(29.75,0.,0.));
#30077=CARTESIAN_POINT('',(79.6628916636062,-6.94043042295203,-0.00713010923047652));
#30078=CARTESIAN_POINT('',(79.4835483363939,-6.93525986827018,-0.000860828807844148));
#30079=CARTESIAN_POINT('',(29.75,-6.933,-8.4904762584886E-16));
#30080=CARTESIAN_POINT('Ctrl Pts',(79.6628916636062,-6.94043042295203,-0.00713010923047652));
#30081=CARTESIAN_POINT('Ctrl Pts',(79.6048514217793,-6.92467100667924,2.0081896470561));
#30082=CARTESIAN_POINT('Ctrl Pts',(79.5468111799523,-5.99531508320213,4.04002741126765));
#30083=CARTESIAN_POINT('Ctrl Pts',(79.4887709381254,-4.44984465230886,5.33171148088348));
#30084=CARTESIAN_POINT('Ctrl Pts',(79.4226004033113,-2.687884299759,6.80433500909159));
#30085=CARTESIAN_POINT('Ctrl Pts',(79.3564298684973,-0.125108764999251,
7.3149193243508));
#30086=CARTESIAN_POINT('Ctrl Pts',(79.2902593336833,2.06669920281348,6.63000898567692));
#30087=CARTESIAN_POINT('Ctrl Pts',(79.2240887988692,4.25850717062608,5.94509864700308));
#30088=CARTESIAN_POINT('Ctrl Pts',(79.1579182640551,6.07934757149164,4.0646936543963));
#30089=CARTESIAN_POINT('Ctrl Pts',(79.0917477292411,6.69232407312594,1.85551141711626));
#30090=CARTESIAN_POINT('Ctrl Pts',(79.0255771944271,7.30530057476027,-0.353670820163851));
#30091=CARTESIAN_POINT('Ctrl Pts',(78.9594066596131,6.71041317716317,-2.89163030211736));
#30092=CARTESIAN_POINT('Ctrl Pts',(78.893236124799,5.18579366300061,-4.614540173529));
#30093=CARTESIAN_POINT('Ctrl Pts',(78.860150857392,4.42348390591939,-5.47599510923475));
#30094=CARTESIAN_POINT('Ctrl Pts',(78.827065589985,3.42874111969687,-6.13368764230509));
#30095=CARTESIAN_POINT('Ctrl Pts',(78.793980322578,2.34055610925253,-6.52219444931898));
#30096=CARTESIAN_POINT('Ctrl Pts',(78.7608950551709,1.252371098808,-6.91070125633294));
#30097=CARTESIAN_POINT('Ctrl Pts',(78.7278097877639,0.0707438641416697,
-7.03002233729033));
#30098=CARTESIAN_POINT('Ctrl Pts',(78.6947245203569,-1.06492368765609,-6.85355939182368));
#30099=CARTESIAN_POINT('Ctrl Pts',(78.6616392529499,-2.20059123945372,-6.67709644635705));
#30100=CARTESIAN_POINT('Ctrl Pts',(78.6285539855429,-3.29029910838259,-6.20484947446653));
#30101=CARTESIAN_POINT('Ctrl Pts',(78.5954687181359,-4.2092890275671,-5.50446266384738));
#30102=CARTESIAN_POINT('Ctrl Pts',(78.5623834507288,-5.12827894675161,-4.80407585322824));
#30103=CARTESIAN_POINT('Ctrl Pts',(78.5292981833218,-5.87655091619167,-3.87554920388036));
#30104=CARTESIAN_POINT('Ctrl Pts',(78.4962129159148,-6.34151941390539,-2.82339661602677));
#30105=CARTESIAN_POINT('Ctrl Pts',(78.4684391651453,-6.73184175926583,-1.94015685293011));
#30106=CARTESIAN_POINT('Ctrl Pts',(78.4406654143758,-6.92252221752414,-0.969798794008508));
#30107=CARTESIAN_POINT('Ctrl Pts',(78.4128916636062,-6.91962899029542,0.00084433539633888));
#30108=CARTESIAN_POINT('Ctrl Pts',(78.2335483363939,-6.92245089085948,-0.0021973978771043));
#30109=CARTESIAN_POINT('Ctrl Pts',(78.2599528433368,-6.92708229965828,-0.925968209479977));
#30110=CARTESIAN_POINT('Ctrl Pts',(78.2863573502796,-6.75592926100566,-1.84835771580232));
#30111=CARTESIAN_POINT('Ctrl Pts',(78.3127618572225,-6.40116091921723,-2.69321436787948));
#30112=CARTESIAN_POINT('Ctrl Pts',(78.3789323920366,-5.51210016296075,-4.81045202848222));
#30113=CARTESIAN_POINT('Ctrl Pts',(78.4451029268507,-3.46989940157015,-6.44076820478922));
#30114=CARTESIAN_POINT('Ctrl Pts',(78.5112734616647,-1.20831798698859,-6.83873031983177));
#30115=CARTESIAN_POINT('Ctrl Pts',(78.5774439964787,1.05326342759283,-7.2366924348743));
#30116=CARTESIAN_POINT('Ctrl Pts',(78.6436145312927,3.53422549536492,-6.40230048865278));
#30117=CARTESIAN_POINT('Ctrl Pts',(78.7097850661068,5.09314398382109,-4.72122955159532));
#30118=CARTESIAN_POINT('Ctrl Pts',(78.7759556009208,6.65206247227726,-3.04015861453786));
#30119=CARTESIAN_POINT('Ctrl Pts',(78.8421261357349,7.28893738141711,-0.512408686644281));
#30120=CARTESIAN_POINT('Ctrl Pts',(78.9082966705489,6.72564139547028,1.71819229071338));
#30121=CARTESIAN_POINT('Ctrl Pts',(78.941381937956,6.44399340249686,2.83349277939225));
#30122=CARTESIAN_POINT('Ctrl Pts',(78.974467205363,5.86230268575175,3.87450603043722));
#30123=CARTESIAN_POINT('Ctrl Pts',(79.00755247277,5.07400169053412,4.71929339835356));
#30124=CARTESIAN_POINT('Ctrl Pts',(79.0406377401769,4.28570069531653,5.56408076626987));
#30125=CARTESIAN_POINT('Ctrl Pts',(79.073723007584,3.29078942162624,6.2126422510577));
#30126=CARTESIAN_POINT('Ctrl Pts',(79.106808274991,2.2008926306588,6.57734068040401));
#30127=CARTESIAN_POINT('Ctrl Pts',(79.139893542398,1.11099583969131,6.94203910975033));
#30128=CARTESIAN_POINT('Ctrl Pts',(79.1729788098051,-0.0738864685531249,
7.02287448365523));
#30129=CARTESIAN_POINT('Ctrl Pts',(79.2060640772121,-1.21186531751188,6.82265386689802));
#30130=CARTESIAN_POINT('Ctrl Pts',(79.2391493446191,-2.34984416647063,6.6224332501408));
#30131=CARTESIAN_POINT('Ctrl Pts',(79.2722346120261,-3.44091955614338,6.14115664272139));
#30132=CARTESIAN_POINT('Ctrl Pts',(79.3053198794331,-4.33708687488498,5.41997365012329));
#30133=CARTESIAN_POINT('Ctrl Pts',(79.3647293650867,-5.94628769563128,4.12498303918833));
#30134=CARTESIAN_POINT('Ctrl Pts',(79.4241388507403,-6.92703652059706,2.05645008161881));
#30135=CARTESIAN_POINT('Ctrl Pts',(79.4835483363939,-6.94186525225857,-0.00337695104174475));
#30136=CARTESIAN_POINT('Origin',(29.75,0.,0.));
#30137=CARTESIAN_POINT('',(80.9128916636062,-6.9365780831978,0.00570569907908797));
#30138=CARTESIAN_POINT('',(80.7335483363939,-6.933,-3.25614535334751E-12));
#30139=CARTESIAN_POINT('',(29.75,-6.933,-8.4904762584886E-16));
#30140=CARTESIAN_POINT('Ctrl Pts',(80.9128916636062,-6.9365780831978,0.00570569907908797));
#30141=CARTESIAN_POINT('Ctrl Pts',(80.9013784988108,-6.94039333737286,0.406469770832339));
#30142=CARTESIAN_POINT('Ctrl Pts',(80.8898653340155,-6.90893189083218,0.806646451518075));
#30143=CARTESIAN_POINT('Ctrl Pts',(80.8783521692201,-6.84015515512757,1.20022589492488));
#30144=CARTESIAN_POINT('Ctrl Pts',(80.8121816344061,-6.44486910952388,3.46227657559952));
#30145=CARTESIAN_POINT('Ctrl Pts',(80.7460110995921,-4.81697030490652,5.50640481680099));
#30146=CARTESIAN_POINT('Ctrl Pts',(80.6798405647781,-2.7007860187726,6.39796996131343));
#30147=CARTESIAN_POINT('Ctrl Pts',(80.613670029964,-0.584601732638681,7.28953510582587));
#30148=CARTESIAN_POINT('Ctrl Pts',(80.5474994951499,2.01986803501185,7.02853715364932));
#30149=CARTESIAN_POINT('Ctrl Pts',(80.4813289603359,3.91397706158762,5.73680291452963));
#30150=CARTESIAN_POINT('Ctrl Pts',(80.4151584255218,5.80808608816334,4.44506867540999));
#30151=CARTESIAN_POINT('Ctrl Pts',(80.3489878907078,6.99183437366439,2.12259814934748));
#30152=CARTESIAN_POINT('Ctrl Pts',(80.2828173558938,6.93937716091364,-0.177430400215159));
#30153=CARTESIAN_POINT('Ctrl Pts',(80.2497320884868,6.91314855453826,-1.32744467499651));
#30154=CARTESIAN_POINT('Ctrl Pts',(80.2166468210798,6.57786857359988,-2.47184845565289));
#30155=CARTESIAN_POINT('Ctrl Pts',(80.1835615536727,5.99747133187885,-3.47095965960107));
#30156=CARTESIAN_POINT('Ctrl Pts',(80.1504762862657,5.41707409015789,-4.47007086354912));
#30157=CARTESIAN_POINT('Ctrl Pts',(80.1173910188587,4.5915595876543,-5.32388949078905));
#30158=CARTESIAN_POINT('Ctrl Pts',(80.0843057514517,3.61023553540428,-5.92212277622558));
#30159=CARTESIAN_POINT('Ctrl Pts',(80.0512204840447,2.62891148315414,-6.52035606166219));
#30160=CARTESIAN_POINT('Ctrl Pts',(80.0181352166377,1.49177788115749,-6.86300400529537));
#30161=CARTESIAN_POINT('Ctrl Pts',(79.9850499492307,0.337786364125504,-6.92120825488567));
#30162=CARTESIAN_POINT('Ctrl Pts',(79.9519646818237,-0.816205152906479,
-6.97941250447597));
#30163=CARTESIAN_POINT('Ctrl Pts',(79.9188794144166,-1.98705458497383,-6.75317306002338));
#30164=CARTESIAN_POINT('Ctrl Pts',(79.8857941470096,-3.02131033278072,-6.24964965428966));
#30165=CARTESIAN_POINT('Ctrl Pts',(79.8196236121956,-5.08982182839451,-5.2426028428222));
#30166=CARTESIAN_POINT('Ctrl Pts',(79.7534530773815,-6.61195858696656,-3.12642018623015));
#30167=CARTESIAN_POINT('Ctrl Pts',(79.6872825425675,-6.89245438108255,-0.850997487355676));
#30168=CARTESIAN_POINT('Ctrl Pts',(79.6791522495804,-6.92691855753537,-0.571419072834691));
#30169=CARTESIAN_POINT('Ctrl Pts',(79.6710219565933,-6.94263800630402,-0.289436653199143));
#30170=CARTESIAN_POINT('Ctrl Pts',(79.6628916636062,-6.94043042295203,-0.00713010923047652));
#30171=CARTESIAN_POINT('Ctrl Pts',(79.4835483363939,-6.933,-3.60267371490863E-12));
#30172=CARTESIAN_POINT('Ctrl Pts',(79.540772531679,-6.93299999999897,-1.99420935701981));
#30173=CARTESIAN_POINT('Ctrl Pts',(79.5979967269641,-6.02307502629049,-3.97063309653345));
#30174=CARTESIAN_POINT('Ctrl Pts',(79.6552209222492,-4.50798484753726,-5.26731066241346));
#30175=CARTESIAN_POINT('Ctrl Pts',(79.7124451175342,-2.99289466878403,-6.56398822829346));
#30176=CARTESIAN_POINT('Ctrl Pts',(79.7696693128193,-0.899664345625418,
-7.15779044292451));
#30177=CARTESIAN_POINT('Ctrl Pts',(79.8268935081044,1.07062371682162,-6.84983604599257));
#30178=CARTESIAN_POINT('Ctrl Pts',(79.8841177033895,3.04091177926865,-6.54188164906062));
#30179=CARTESIAN_POINT('Ctrl Pts',(79.9413418986746,4.85311303640116,-5.33766370386184));
#30180=CARTESIAN_POINT('Ctrl Pts',(79.9985660939597,5.90026971493919,-3.64050907030478));
#30181=CARTESIAN_POINT('Ctrl Pts',(80.0557902892448,6.94742639347723,-1.94335443674772));
#30182=CARTESIAN_POINT('Ctrl Pts',(80.1130144845299,7.21086008527499,0.216464293126901));
#30183=CARTESIAN_POINT('Ctrl Pts',(80.170238679815,6.60233935005997,2.11556236179644));
#30184=CARTESIAN_POINT('Ctrl Pts',(80.2274628751001,5.99381861484494,4.01466043046598));
#30185=CARTESIAN_POINT('Ctrl Pts',(80.2846870703852,4.5241977964708,5.61916312790613));
#30186=CARTESIAN_POINT('Ctrl Pts',(80.3419112656703,2.68569473000164,6.39167683923721));
#30187=CARTESIAN_POINT('Ctrl Pts',(80.3991354609554,0.847191663532486,7.1641905505683));
#30188=CARTESIAN_POINT('Ctrl Pts',(80.4563596562405,-1.3273997899442,7.09093574623738));
#30189=CARTESIAN_POINT('Ctrl Pts',(80.5135838515256,-3.10974706736404,6.1964475449261));
#30190=CARTESIAN_POINT('Ctrl Pts',(80.5708080468107,-4.89209434478389,5.30195934361482));
#30191=CARTESIAN_POINT('Ctrl Pts',(80.6280322420957,-6.2504052505877,3.60219296582467));
#30192=CARTESIAN_POINT('Ctrl Pts',(80.6852564373808,-6.72974280712815,1.66644854403216));
#30193=CARTESIAN_POINT('Ctrl Pts',(80.7013537370518,-6.86458158035618,1.12191912096477));
#30194=CARTESIAN_POINT('Ctrl Pts',(80.7174510367228,-6.93300000000028,0.560975745775044));
#30195=CARTESIAN_POINT('Ctrl Pts',(80.7335483363939,-6.933,-3.45320994021847E-12));
#30196=CARTESIAN_POINT('Origin',(29.75,0.,0.));
#30197=CARTESIAN_POINT('',(82.1628916636062,-6.92353455550492,0.00101414875028183));
#30198=CARTESIAN_POINT('',(81.9835483363939,-6.92935402623401,0.00166396505006337));
#30199=CARTESIAN_POINT('',(29.75,-6.933,-8.4904762584886E-16));
#30200=CARTESIAN_POINT('Ctrl Pts',(82.1628916636062,-6.92353455550492,0.00101414875028183));
#30201=CARTESIAN_POINT('Ctrl Pts',(82.1317350410284,-6.92503138592253,1.0907153399273));
#30202=CARTESIAN_POINT('Ctrl Pts',(82.1005784184506,-6.68254061521535,2.17979048906057));
#30203=CARTESIAN_POINT('Ctrl Pts',(82.0694217958728,-6.19243531495591,3.14356638472189));
#30204=CARTESIAN_POINT('Ctrl Pts',(82.0032512610588,-5.15154810863604,5.19043671855075));
#30205=CARTESIAN_POINT('Ctrl Pts',(81.9370807262447,-2.9937856514116,6.67213975217042));
#30206=CARTESIAN_POINT('Ctrl Pts',(81.8709101914307,-0.713310410863843,
6.90806140509355));
#30207=CARTESIAN_POINT('Ctrl Pts',(81.8047396566167,1.56716482968418,7.14398305801671));
#30208=CARTESIAN_POINT('Ctrl Pts',(81.7385691218026,3.97035285355562,6.13412333024305));
#30209=CARTESIAN_POINT('Ctrl Pts',(81.6723985869886,5.41483843060364,4.34349648310992));
#30210=CARTESIAN_POINT('Ctrl Pts',(81.6393133195815,6.13708121912753,3.4481830595435));
#30211=CARTESIAN_POINT('Ctrl Pts',(81.6062280521745,6.61964839594568,2.35767785613726));
#30212=CARTESIAN_POINT('Ctrl Pts',(81.5731427847675,6.82121527266455,1.21993669477338));
#30213=CARTESIAN_POINT('Ctrl Pts',(81.5400575173605,7.02278214938344,0.0821955334093011));
#30214=CARTESIAN_POINT('Ctrl Pts',(81.5069722499535,6.94334872600299,-1.1027815859123));
#30215=CARTESIAN_POINT('Ctrl Pts',(81.4738869825466,6.579940063713,-2.19310910711941));
#30216=CARTESIAN_POINT('Ctrl Pts',(81.4408017151395,6.21653140142307,-3.28343662832634));
#30217=CARTESIAN_POINT('Ctrl Pts',(81.4077164477325,5.56914750022368,-4.27911455141867));
#30218=CARTESIAN_POINT('Ctrl Pts',(81.3746311803254,4.72529340221047,-5.06841450537669));
#30219=CARTESIAN_POINT('Ctrl Pts',(81.3415459129184,3.88143930419715,-5.85771445933481));
#30220=CARTESIAN_POINT('Ctrl Pts',(81.3084606455114,2.84111500936993,-6.4406364441586));
#30221=CARTESIAN_POINT('Ctrl Pts',(81.2753753781044,1.72614853324333,-6.72360380819039));
#30222=CARTESIAN_POINT('Ctrl Pts',(81.2092048432904,-0.503784419009892,
-7.28953853625396));
#30223=CARTESIAN_POINT('Ctrl Pts',(81.1430343084763,-3.03228609646078,-6.65565478114955));
#30224=CARTESIAN_POINT('Ctrl Pts',(81.0768637736623,-4.71520029189113,-5.09872634352341));
#30225=CARTESIAN_POINT('Ctrl Pts',(81.0222064036436,-6.1053003439436,-3.81269149512603));
#30226=CARTESIAN_POINT('Ctrl Pts',(80.9675490336249,-6.91846562125811,-1.89687370018916));
#30227=CARTESIAN_POINT('Ctrl Pts',(80.9128916636062,-6.9365780831978,0.00570569907908797));
#30228=CARTESIAN_POINT('Ctrl Pts',(80.7335483363939,-6.93120482123466,0.00349441528416698));
#30229=CARTESIAN_POINT('Ctrl Pts',(80.786836462586,-6.91342583053146,-1.85300233924437));
#30230=CARTESIAN_POINT('Ctrl Pts',(80.840124588778,-6.15087697410277,-3.71626439473826));
#30231=CARTESIAN_POINT('Ctrl Pts',(80.89341271497,-4.82190773278374,-4.99793256610273));
#30232=CARTESIAN_POINT('Ctrl Pts',(80.959583249784,-3.17166007474918,-6.58944411686849));
#30233=CARTESIAN_POINT('Ctrl Pts',(81.0257537845982,-0.648024325144719,
-7.28417090126887));
#30234=CARTESIAN_POINT('Ctrl Pts',(81.0919243194122,1.58784222942491,-6.76069684274643));
#30235=CARTESIAN_POINT('Ctrl Pts',(81.1580948542262,3.82370878399466,-6.23722278422395));
#30236=CARTESIAN_POINT('Ctrl Pts',(81.2242653890402,5.77180614352961,-4.49554788277849));
#30237=CARTESIAN_POINT('Ctrl Pts',(81.2904359238542,6.54140203412602,-2.33202147781674));
#30238=CARTESIAN_POINT('Ctrl Pts',(81.3566064586682,7.3109979247224,-0.168495072855053));
#30239=CARTESIAN_POINT('Ctrl Pts',(81.4227769934823,6.9020923463804,2.41688283562278));
#30240=CARTESIAN_POINT('Ctrl Pts',(81.4889475282964,5.50458035700961,4.23434991610444));
#30241=CARTESIAN_POINT('Ctrl Pts',(81.5551180631104,4.10706836763878,6.05181699658616));
#30242=CARTESIAN_POINT('Ctrl Pts',(81.6212885979244,1.72094996723906,7.10137324907152));
#30243=CARTESIAN_POINT('Ctrl Pts',(81.6874591327385,-0.572357798069008,
6.91800863538923));
#30244=CARTESIAN_POINT('Ctrl Pts',(81.7205444001455,-1.71901168072304,6.82632632854809));
#30245=CARTESIAN_POINT('Ctrl Pts',(81.7536296675526,-2.84246290460419,6.42641380516503));
#30246=CARTESIAN_POINT('Ctrl Pts',(81.7867149349595,-3.80689731953615,5.79005666067225));
#30247=CARTESIAN_POINT('Ctrl Pts',(81.8198002023665,-4.771331734468,5.15369951617955));
#30248=CARTESIAN_POINT('Ctrl Pts',(81.8528854697735,-5.57674934045072,4.28089775057717));
#30249=CARTESIAN_POINT('Ctrl Pts',(81.8859707371805,-6.11812269421474,3.26709557502076));
#30250=CARTESIAN_POINT('Ctrl Pts',(81.918496603585,-6.65034258419854,2.27043462266962));
#30251=CARTESIAN_POINT('Ctrl Pts',(81.9510224699895,-6.92737158357288,1.13750098159251));
#30252=CARTESIAN_POINT('Ctrl Pts',(81.9835483363939,-6.92935402623401,0.00166396505006337));
#30253=CARTESIAN_POINT('Origin',(29.75,0.,0.));
#30254=CARTESIAN_POINT('',(83.4128916636062,-6.93231962597778,-0.00593826529341535));
#30255=CARTESIAN_POINT('',(83.2335483363939,-6.933,-2.56308863022525E-12));
#30256=CARTESIAN_POINT('',(29.75,-6.933,-8.4904762584886E-16));
#30257=CARTESIAN_POINT('Ctrl Pts',(83.4128916636062,-6.93231962597778,-0.00593826529341535));
#30258=CARTESIAN_POINT('Ctrl Pts',(83.362091583246,-6.9151268553501,1.76512680626223));
#30259=CARTESIAN_POINT('Ctrl Pts',(83.3112915028857,-6.22396082486215,3.54762724591841));
#30260=CARTESIAN_POINT('Ctrl Pts',(83.2604914225255,-5.00363410987313,4.81599105203737));
#30261=CARTESIAN_POINT('Ctrl Pts',(83.1943208877115,-3.41407616417583,6.46812055251247));
#30262=CARTESIAN_POINT('Ctrl Pts',(83.1281503528975,-0.926700730346132,
7.24792360395334));
#30263=CARTESIAN_POINT('Ctrl Pts',(83.0619798180834,1.3323608810027,6.81258037832244));
#30264=CARTESIAN_POINT('Ctrl Pts',(83.0288945506764,2.46189168667719,6.59490876550698));
#30265=CARTESIAN_POINT('Ctrl Pts',(82.9958092832693,3.53434403673139,6.07345058342356));
#30266=CARTESIAN_POINT('Ctrl Pts',(82.9627240158623,4.42265598791498,5.33454190609151));
#30267=CARTESIAN_POINT('Ctrl Pts',(82.9296387484553,5.31096793909847,4.59563322875955));
#30268=CARTESIAN_POINT('Ctrl Pts',(82.8965534810483,6.01513949141133,3.63927405617907));
#30269=CARTESIAN_POINT('Ctrl Pts',(82.8634682136413,6.44131840033896,2.57191680721605));
#30270=CARTESIAN_POINT('Ctrl Pts',(82.8303829462343,6.86749730926663,1.5045595582529));
#30271=CARTESIAN_POINT('Ctrl Pts',(82.7972976788272,7.01568357480899,0.326204232906858));
#30272=CARTESIAN_POINT('Ctrl Pts',(82.7642124114202,6.88059876318932,-0.82133062483032));
#30273=CARTESIAN_POINT('Ctrl Pts',(82.7311271440132,6.74551395156967,-1.96886548256737));
#30274=CARTESIAN_POINT('Ctrl Pts',(82.6980418766062,6.32715806278815,-3.08557987269584));
#30275=CARTESIAN_POINT('Ctrl Pts',(82.6649566091992,5.65818466826036,-4.0213658361549));
#30276=CARTESIAN_POINT('Ctrl Pts',(82.5987860743851,4.32023787920462,-5.89293776307323));
#30277=CARTESIAN_POINT('Ctrl Pts',(82.5326155395711,1.97982106716371,-7.04079598331348));
#30278=CARTESIAN_POINT('Ctrl Pts',(82.466445004757,-0.310512453395021,-6.93784592903852));
#30279=CARTESIAN_POINT('Ctrl Pts',(82.400274469943,-2.60084597395362,-6.83489587476358));
#30280=CARTESIAN_POINT('Ctrl Pts',(82.334103935129,-4.84109620302989,-5.48113754597357));
#30281=CARTESIAN_POINT('Ctrl Pts',(82.267933400315,-5.99921533986046,-3.4982395645595));
#30282=CARTESIAN_POINT('Ctrl Pts',(82.2329194880787,-6.61203012109301,-2.4489958779279));
#30283=CARTESIAN_POINT('Ctrl Pts',(82.1979055758425,-6.9218524126878,-1.22359553981082));
#30284=CARTESIAN_POINT('Ctrl Pts',(82.1628916636062,-6.92353455550492,0.00101414875028183));
#30285=CARTESIAN_POINT('Ctrl Pts',(81.9835483363939,-6.92935402623401,0.00166396505006337));
#30286=CARTESIAN_POINT('Ctrl Pts',(81.9841077373965,-6.92938812157212,-0.0178708986160241));
#30287=CARTESIAN_POINT('Ctrl Pts',(81.9846671383991,-6.92934085990654,-0.0374066210819144));
#30288=CARTESIAN_POINT('Ctrl Pts',(81.9852265394017,-6.92921214022652,-0.056942523864537));
#30289=CARTESIAN_POINT('Ctrl Pts',(82.0183118068087,-6.92159913092891,-1.21237586168268));
#30290=CARTESIAN_POINT('Ctrl Pts',(82.0513970742157,-6.62904401078835,-2.36843995180839));
#30291=CARTESIAN_POINT('Ctrl Pts',(82.0844823416227,-6.06743435498427,-3.37234002975485));
#30292=CARTESIAN_POINT('Ctrl Pts',(82.1506528764367,-4.94421504337618,-5.38014018564764));
#30293=CARTESIAN_POINT('Ctrl Pts',(82.2168234112508,-2.74477758911402,-6.77928429282362));
#30294=CARTESIAN_POINT('Ctrl Pts',(82.2829939460648,-0.457073205771369,
-6.92973363148655));
#30295=CARTESIAN_POINT('Ctrl Pts',(82.3491644808789,1.83063117757141,-7.08018297014949));
#30296=CARTESIAN_POINT('Ctrl Pts',(82.4153350156929,4.20660248999483,-5.98193754029923));
#30297=CARTESIAN_POINT('Ctrl Pts',(82.4815055505069,5.57648760428372,-4.1389673524125));
#30298=CARTESIAN_POINT('Ctrl Pts',(82.5476760853209,6.94637271857261,-2.29599716452578));
#30299=CARTESIAN_POINT('Ctrl Pts',(82.613846620135,7.31017163472707,0.291697781397146));
#30300=CARTESIAN_POINT('Ctrl Pts',(82.680017154949,6.50154387995514,2.44094078627165));
#30301=CARTESIAN_POINT('Ctrl Pts',(82.7461876897631,5.6929161251832,4.59018379114616));
#30302=CARTESIAN_POINT('Ctrl Pts',(82.8123582245771,3.7118616994847,6.30097485497203));
#30303=CARTESIAN_POINT('Ctrl Pts',(82.8785287593911,1.47135462991242,6.78713781146553));
#30304=CARTESIAN_POINT('Ctrl Pts',(82.9446992942052,-0.769152439659738,
7.27330076795901));
#30305=CARTESIAN_POINT('Ctrl Pts',(83.0108698290192,-3.26911215310578,6.5348356171203));
#30306=CARTESIAN_POINT('Ctrl Pts',(83.0770403638333,-4.902394538607,4.91456658477292));
#30307=CARTESIAN_POINT('Ctrl Pts',(83.1101256312403,-5.71903573135766,4.10443206859918));
#30308=CARTESIAN_POINT('Ctrl Pts',(83.1432108986473,-6.31900759212212,3.07384658204822));
#30309=CARTESIAN_POINT('Ctrl Pts',(83.1762961660543,-6.64490887109431,1.96530135860606));
#30310=CARTESIAN_POINT('Ctrl Pts',(83.1953802228341,-6.83289340318271,1.32587657394482));
#30311=CARTESIAN_POINT('Ctrl Pts',(83.214464279614,-6.92969060024565,0.660513432091375));
#30312=CARTESIAN_POINT('Ctrl Pts',(83.2335483363938,-6.93172781140961,-0.00378750055469096));
#30313=CARTESIAN_POINT('Origin',(29.75,0.,0.));
#30314=CARTESIAN_POINT('',(84.6628916636062,-6.94340481590983,0.0048587949936791));
#30315=CARTESIAN_POINT('',(84.4835483363939,-6.93470434732279,0.000299062045973509));
#30316=CARTESIAN_POINT('',(29.75,-6.933,-8.4904762584886E-16));
#30317=CARTESIAN_POINT('Ctrl Pts',(84.6628916636062,-6.94340481590983,0.0048587949936791));
#30318=CARTESIAN_POINT('Ctrl Pts',(84.6586186602776,-6.94414319679649,0.153029414161253));
#30319=CARTESIAN_POINT('Ctrl Pts',(84.6543456569489,-6.93981013338403,0.301132648058085));
#30320=CARTESIAN_POINT('Ctrl Pts',(84.6500726536203,-6.93026956754333,0.44887396891849));
#30321=CARTESIAN_POINT('Ctrl Pts',(84.5839021188062,-6.78252703247977,2.73675475523645));
#30322=CARTESIAN_POINT('Ctrl Pts',(84.5177315839921,-5.38598616984263,4.93784606793614));
#30323=CARTESIAN_POINT('Ctrl Pts',(84.4515610491781,-3.37951635660294,6.06344012288267));
#30324=CARTESIAN_POINT('Ctrl Pts',(84.4184757817711,-2.3762814499831,6.62623715035594));
#30325=CARTESIAN_POINT('Ctrl Pts',(84.3853905143641,-1.22056430571257,6.92015986339094));
#30326=CARTESIAN_POINT('Ctrl Pts',(84.3523052469571,-0.0651407839431917,
6.92913991874561));
#30327=CARTESIAN_POINT('Ctrl Pts',(84.3192199795501,1.09028273782619,6.93811997410028));
#30328=CARTESIAN_POINT('Ctrl Pts',(84.2861347121431,2.2454126370945,6.66215737177462));
#30329=CARTESIAN_POINT('Ctrl Pts',(84.2530494447361,3.2598546291538,6.12198387735301));
#30330=CARTESIAN_POINT('Ctrl Pts',(84.219964177329,4.2742966212131,5.5818103829314));
#30331=CARTESIAN_POINT('Ctrl Pts',(84.186878909922,5.14805070606347,4.7774259964138));
#30332=CARTESIAN_POINT('Ctrl Pts',(84.1537936425149,5.78554847609396,3.8137451627047));
#30333=CARTESIAN_POINT('Ctrl Pts',(84.1207083751079,6.42304624612438,2.85006432899571));
#30334=CARTESIAN_POINT('Ctrl Pts',(84.0876231077009,6.82428770133504,1.72708704809516));
#30335=CARTESIAN_POINT('Ctrl Pts',(84.0545378402939,6.91732660797555,0.580542441965909));
#30336=CARTESIAN_POINT('Ctrl Pts',(83.9883673054799,7.1034044212566,-1.71254677029273));
#30337=CARTESIAN_POINT('Ctrl Pts',(83.9221967706659,6.05667204025721,-4.09990528346618));
#30338=CARTESIAN_POINT('Ctrl Pts',(83.8560262358518,4.2408596986948,-5.49956663154253));
#30339=CARTESIAN_POINT('Ctrl Pts',(83.7898557010378,2.42504735713218,-6.89922797961903));
#30340=CARTESIAN_POINT('Ctrl Pts',(83.7236851662237,-0.159844944993682,
-7.31119216259787));
#30341=CARTESIAN_POINT('Ctrl Pts',(83.6575146314097,-2.32428038332007,-6.54415658773383));
#30342=CARTESIAN_POINT('Ctrl Pts',(83.5913440965957,-4.48871582164609,-5.77712101286992));
#30343=CARTESIAN_POINT('Ctrl Pts',(83.5251735617817,-6.2326943961729,-3.8310856801635));
#30344=CARTESIAN_POINT('Ctrl Pts',(83.4590030269676,-6.75881345465409,-1.59584003905574));
#30345=CARTESIAN_POINT('Ctrl Pts',(83.4436325725138,-6.88102327279128,-1.07662493196513));
#30346=CARTESIAN_POINT('Ctrl Pts',(83.42826211806,-6.9375215999903,-0.541805036054968));
#30347=CARTESIAN_POINT('Ctrl Pts',(83.4128916636062,-6.93231962597778,-0.00593826529341535));
#30348=CARTESIAN_POINT('Ctrl Pts',(83.2335483363939,-6.933,-2.56308863022525E-12));
#30349=CARTESIAN_POINT('Ctrl Pts',(83.290772531679,-6.93299999999926,-1.99420935701877));
#30350=CARTESIAN_POINT('Ctrl Pts',(83.347996726964,-6.02307502629109,-3.97063309653254));
#30351=CARTESIAN_POINT('Ctrl Pts',(83.4052209222491,-4.50798484753805,-5.26731066241278));
#30352=CARTESIAN_POINT('Ctrl Pts',(83.4624451175342,-2.99289466878501,-6.56398822829301));
#30353=CARTESIAN_POINT('Ctrl Pts',(83.5196693128193,-0.899664345626491,
-7.15779044292437));
#30354=CARTESIAN_POINT('Ctrl Pts',(83.5768935081044,1.07062371682059,-6.84983604599273));
#30355=CARTESIAN_POINT('Ctrl Pts',(83.6341177033895,3.04091177926767,-6.54188164906108));
#30356=CARTESIAN_POINT('Ctrl Pts',(83.6913418986746,4.85311303640036,-5.33766370386257));
#30357=CARTESIAN_POINT('Ctrl Pts',(83.7485660939597,5.90026971493865,-3.64050907030567));
#30358=CARTESIAN_POINT('Ctrl Pts',(83.8057902892448,6.94742639347693,-1.94335443674876));
#30359=CARTESIAN_POINT('Ctrl Pts',(83.8630144845299,7.21086008527503,0.216464293125819));
#30360=CARTESIAN_POINT('Ctrl Pts',(83.920238679815,6.60233935006029,2.11556236179545));
#30361=CARTESIAN_POINT('Ctrl Pts',(83.9774628751001,5.99381861484554,4.01466043046508));
#30362=CARTESIAN_POINT('Ctrl Pts',(84.0346870703851,4.52419779647164,5.61916312790545));
#30363=CARTESIAN_POINT('Ctrl Pts',(84.0919112656702,2.6856947300026,6.39167683923681));
#30364=CARTESIAN_POINT('Ctrl Pts',(84.1491354609553,0.84719166353356,7.16419055056817));
#30365=CARTESIAN_POINT('Ctrl Pts',(84.2063596562404,-1.32739978994314,7.09093574623758));
#30366=CARTESIAN_POINT('Ctrl Pts',(84.2635838515255,-3.10974706736312,6.19644754492657));
#30367=CARTESIAN_POINT('Ctrl Pts',(84.3208080468106,-4.89209434478309,5.30195934361556));
#30368=CARTESIAN_POINT('Ctrl Pts',(84.3780322420957,-6.25040525058716,3.60219296582561));
#30369=CARTESIAN_POINT('Ctrl Pts',(84.4352564373808,-6.7297428071279,1.66644854403317));
#30370=CARTESIAN_POINT('Ctrl Pts',(84.4513537370518,-6.86458158035605,1.12191912096567));
#30371=CARTESIAN_POINT('Ctrl Pts',(84.4674510367228,-6.93300000000023,0.560975745775821));
#30372=CARTESIAN_POINT('Ctrl Pts',(84.4835483363939,-6.933,-2.8078928071551E-12));
#30373=CARTESIAN_POINT('Origin',(29.75,0.,0.));
#30374=CARTESIAN_POINT('',(85.9128916636062,-6.92777016594518,0.000431384726357015));
#30375=CARTESIAN_POINT('',(85.7335483363939,-6.92921246598513,0.00257278641648163));
#30376=CARTESIAN_POINT('',(29.75,-6.933,-8.4904762584886E-16));
#30377=CARTESIAN_POINT('Ctrl Pts',(85.9128916636062,-6.92137817579339,0.000958630302984043));
#30378=CARTESIAN_POINT('Ctrl Pts',(85.8889752024951,-6.92604506083378,0.836427548270157));
#30379=CARTESIAN_POINT('Ctrl Pts',(85.8650587413841,-6.78625928845202,1.67113888616492));
#30380=CARTESIAN_POINT('Ctrl Pts',(85.841142280273,-6.49492932481831,2.44996530464116));
#30381=CARTESIAN_POINT('Ctrl Pts',(85.8080570128659,-6.0919127704156,3.52736886360613));
#30382=CARTESIAN_POINT('Ctrl Pts',(85.7749717454589,-5.39888502526939,4.497825056979));
#30383=CARTESIAN_POINT('Ctrl Pts',(85.7418864780518,-4.52216542065837,5.25045171804183));
#30384=CARTESIAN_POINT('Ctrl Pts',(85.7088012106448,-3.64544581604724,6.00307837910473));
#30385=CARTESIAN_POINT('Ctrl Pts',(85.6757159432379,-2.58503435197131,6.53787550785749));
#30386=CARTESIAN_POINT('Ctrl Pts',(85.6426306758309,-1.4615458932431,6.78006064867637));
#30387=CARTESIAN_POINT('Ctrl Pts',(85.6095454084239,-0.338057434515012,
7.02224578949523));
#30388=CARTESIAN_POINT('Ctrl Pts',(85.5764601410168,0.84850801886527,6.97181894238025));
#30389=CARTESIAN_POINT('Ctrl Pts',(85.5433748736098,1.9574380566315,6.64722946720943));
#30390=CARTESIAN_POINT('Ctrl Pts',(85.5102896062027,3.06636809439786,6.32263999203856));
#30391=CARTESIAN_POINT('Ctrl Pts',(85.4772043387958,4.09766271655007,5.72388788881181));
#30392=CARTESIAN_POINT('Ctrl Pts',(85.4441190713888,4.90876287502491,4.90820577860255));
#30393=CARTESIAN_POINT('Ctrl Pts',(85.3779485365747,6.5309631919745,3.27684155818413));
#30394=CARTESIAN_POINT('Ctrl Pts',(85.3117780017607,7.27238565421453,0.777757309835552));
#30395=CARTESIAN_POINT('Ctrl Pts',(85.2456074669466,6.78887389477455,-1.46332339543877));
#30396=CARTESIAN_POINT('Ctrl Pts',(85.1794369321326,6.30536213533455,-3.70440410071322));
#30397=CARTESIAN_POINT('Ctrl Pts',(85.1132663973185,4.59691615421462,-5.68748126291356));
#30398=CARTESIAN_POINT('Ctrl Pts',(85.0470958625045,2.44863138187429,-6.49865132937342));
#30399=CARTESIAN_POINT('Ctrl Pts',(84.9809253276904,0.300346609533963,-7.30982139583328));
#30400=CARTESIAN_POINT('Ctrl Pts',(84.9147547928764,-2.28777695402661,-6.94908436655257));
#30401=CARTESIAN_POINT('Ctrl Pts',(84.8485842580624,-4.13236663206187,-5.581380721944));
#30402=CARTESIAN_POINT('Ctrl Pts',(84.786686726577,-5.8578407875103,-4.30199738851975));
#30403=CARTESIAN_POINT('Ctrl Pts',(84.7247891950916,-6.93270883683727,-2.14149936570948));
#30404=CARTESIAN_POINT('Ctrl Pts',(84.6628916636062,-6.94340481590983,0.0048587949936791));
#30405=CARTESIAN_POINT('Ctrl Pts',(84.4835483363939,-6.94155004985185,0.00150027839546349));
#30406=CARTESIAN_POINT('Ctrl Pts',(84.5109913566456,-6.93928989654419,-0.953521174230491));
#30407=CARTESIAN_POINT('Ctrl Pts',(84.5384343768973,-6.73091917705912,-1.91105609676861));
#30408=CARTESIAN_POINT('Ctrl Pts',(84.5658773971491,-6.34390333657409,-2.78785110640628));
#30409=CARTESIAN_POINT('Ctrl Pts',(84.5989626645561,-5.87731757248042,-3.84491396205739));
#30410=CARTESIAN_POINT('Ctrl Pts',(84.6320479319631,-5.15107683485604,-4.78462393491109));
#30411=CARTESIAN_POINT('Ctrl Pts',(84.6651331993701,-4.24177091760061,-5.48750565196823));
#30412=CARTESIAN_POINT('Ctrl Pts',(84.6982184667772,-3.33246500034529,-6.19038736902529));
#30413=CARTESIAN_POINT('Ctrl Pts',(84.7313037341842,-2.24009390345898,-6.65644083028586));
#30414=CARTESIAN_POINT('Ctrl Pts',(84.7643890015912,-1.09957551318182,-6.84164870671519));
#30415=CARTESIAN_POINT('Ctrl Pts',(84.7974742689982,0.0409428770954647,
-7.02685658314454));
#30416=CARTESIAN_POINT('Ctrl Pts',(84.8305595364052,1.2296085607636,-6.93121887474259));
#30417=CARTESIAN_POINT('Ctrl Pts',(84.8636448038122,2.31311716204457,-6.54491603635869));
#30418=CARTESIAN_POINT('Ctrl Pts',(84.9298153386262,4.48013436460651,-5.7723103595909));
#30419=CARTESIAN_POINT('Ctrl Pts',(84.9959858734404,6.22652323761978,-3.83704416289533));
#30420=CARTESIAN_POINT('Ctrl Pts',(85.0621564082544,6.7564304231043,-1.6064781531476));
#30421=CARTESIAN_POINT('Ctrl Pts',(85.1283269430685,7.28633760858878,0.624087856599996));
#30422=CARTESIAN_POINT('Ctrl Pts',(85.1944974778824,6.59976310654463,3.14995367939972));
#30423=CARTESIAN_POINT('Ctrl Pts',(85.2606680126964,5.01109087012319,4.80803837717989));
#30424=CARTESIAN_POINT('Ctrl Pts',(85.3268385475104,3.42241863370165,6.46612307496015));
#30425=CARTESIAN_POINT('Ctrl Pts',(85.3930090823246,0.931648662902707,7.25642664772076));
#30426=CARTESIAN_POINT('Ctrl Pts',(85.4591796171386,-1.32235953455869,6.81759708448866));
#30427=CARTESIAN_POINT('Ctrl Pts',(85.5253501519526,-3.57636773201997,6.37876752125658));
#30428=CARTESIAN_POINT('Ctrl Pts',(85.5915206867667,-5.59361415614373,4.71080482203193));
#30429=CARTESIAN_POINT('Ctrl Pts',(85.6576912215807,-6.44666043474205,2.58276854517033));
#30430=CARTESIAN_POINT('Ctrl Pts',(85.6829769265184,-6.77263447378339,1.76958337831761));
#30431=CARTESIAN_POINT('Ctrl Pts',(85.7082626314561,-6.92860868119207,0.889216953124101));
#30432=CARTESIAN_POINT('Ctrl Pts',(85.7335483363939,-6.9229639019227,0.00681729503297956));
#30433=CARTESIAN_POINT('Origin',(29.75,0.,0.));
#30434=CARTESIAN_POINT('',(87.1628916636062,-6.93297740291849,-0.000166944099082397));
#30435=CARTESIAN_POINT('',(86.9835483363939,-6.93072156200529,-0.00296430948166657));
#30436=CARTESIAN_POINT('',(29.75,-6.933,-8.4904762584886E-16));
#30437=CARTESIAN_POINT('Ctrl Pts',(87.1628916636062,-6.933,2.97289970419001E-12));
#30438=CARTESIAN_POINT('Ctrl Pts',(87.1056674683211,-6.93299999999915,1.99420935701932));
#30439=CARTESIAN_POINT('Ctrl Pts',(87.048443273036,-6.02307502629073,3.97063309653316));
#30440=CARTESIAN_POINT('Ctrl Pts',(86.9912190777509,-4.50798484753744,5.2673106624133));
#30441=CARTESIAN_POINT('Ctrl Pts',(86.9339948824658,-2.99289466878415,6.56398822829345));
#30442=CARTESIAN_POINT('Ctrl Pts',(86.8767706871807,-0.899664345625384,
7.15779044292455));
#30443=CARTESIAN_POINT('Ctrl Pts',(86.8195464918956,1.07062371682177,6.84983604599254));
#30444=CARTESIAN_POINT('Ctrl Pts',(86.7623222966105,3.04091177926893,6.54188164906054));
#30445=CARTESIAN_POINT('Ctrl Pts',(86.7050981013254,4.85311303640152,5.33766370386157));
#30446=CARTESIAN_POINT('Ctrl Pts',(86.6478739060403,5.90026971493948,3.64050907030431));
#30447=CARTESIAN_POINT('Ctrl Pts',(86.5906497107552,6.94742639347745,1.94335443674705));
#30448=CARTESIAN_POINT('Ctrl Pts',(86.5334255154701,7.210860085275,-0.21646429312776));
#30449=CARTESIAN_POINT('Ctrl Pts',(86.476201320185,6.60233935005968,-2.11556236179734));
#30450=CARTESIAN_POINT('Ctrl Pts',(86.4189771248999,5.99381861484435,-4.01466043046692));
#30451=CARTESIAN_POINT('Ctrl Pts',(86.3617529296148,4.52419779646983,-5.61916312790696));
#30452=CARTESIAN_POINT('Ctrl Pts',(86.3045287343297,2.6856947300004,-6.39167683923773));
#30453=CARTESIAN_POINT('Ctrl Pts',(86.2473045390446,0.847191663530979,-7.16419055056851));
#30454=CARTESIAN_POINT('Ctrl Pts',(86.1900803437595,-1.32739978994586,-7.09093574623711));
#30455=CARTESIAN_POINT('Ctrl Pts',(86.1328561484744,-3.10974706736559,-6.19644754492533));
#30456=CARTESIAN_POINT('Ctrl Pts',(86.0756319531893,-4.89209434478533,-5.30195934361354));
#30457=CARTESIAN_POINT('Ctrl Pts',(86.0184077579042,-6.25040525058877,-3.60219296582288));
#30458=CARTESIAN_POINT('Ctrl Pts',(85.9611835626191,-6.72974280712866,-1.66644854403009));
#30459=CARTESIAN_POINT('Ctrl Pts',(85.9450862629482,-6.86458158035627,-1.12191912096368));
#30460=CARTESIAN_POINT('Ctrl Pts',(85.9289889632772,-6.9330000000002,-0.560975745775017));
#30461=CARTESIAN_POINT('Ctrl Pts',(85.9128916636062,-6.933,2.429445533636E-12));
#30462=CARTESIAN_POINT('Ctrl Pts',(85.7335483363939,-6.933,-3.05241942832879E-12));
#30463=CARTESIAN_POINT('Ctrl Pts',(85.790772531679,-6.93299999999912,-1.99420935701939));
#30464=CARTESIAN_POINT('Ctrl Pts',(85.8479967269641,-6.02307502629068,-3.97063309653323));
#30465=CARTESIAN_POINT('Ctrl Pts',(85.9052209222492,-4.50798484753738,-5.26731066241335));
#30466=CARTESIAN_POINT('Ctrl Pts',(85.9624451175343,-2.99289466878407,-6.56398822829348));
#30467=CARTESIAN_POINT('Ctrl Pts',(86.0196693128193,-0.899664345625303,
-7.15779044292456));
#30468=CARTESIAN_POINT('Ctrl Pts',(86.0768935081044,1.07062371682185,-6.84983604599253));
#30469=CARTESIAN_POINT('Ctrl Pts',(86.1341177033895,3.04091177926901,-6.5418816490605));
#30470=CARTESIAN_POINT('Ctrl Pts',(86.1913418986746,4.85311303640158,-5.33766370386151));
#30471=CARTESIAN_POINT('Ctrl Pts',(86.2485660939597,5.90026971493953,-3.64050907030424));
#30472=CARTESIAN_POINT('Ctrl Pts',(86.3057902892448,6.94742639347747,-1.94335443674697));
#30473=CARTESIAN_POINT('Ctrl Pts',(86.3630144845299,7.210860085275,0.216464293127843));
#30474=CARTESIAN_POINT('Ctrl Pts',(86.420238679815,6.60233935005965,2.11556236179742));
#30475=CARTESIAN_POINT('Ctrl Pts',(86.4774628751001,5.99381861484431,4.01466043046699));
#30476=CARTESIAN_POINT('Ctrl Pts',(86.5346870703852,4.52419779646977,5.61916312790701));
#30477=CARTESIAN_POINT('Ctrl Pts',(86.5919112656703,2.68569473000033,6.39167683923776));
#30478=CARTESIAN_POINT('Ctrl Pts',(86.6491354609554,0.847191663530897,7.16419055056852));
#30479=CARTESIAN_POINT('Ctrl Pts',(86.7063596562405,-1.32739978994594,7.09093574623709));
#30480=CARTESIAN_POINT('Ctrl Pts',(86.7635838515256,-3.10974706736567,6.19644754492529));
#30481=CARTESIAN_POINT('Ctrl Pts',(86.8208080468107,-4.89209434478539,5.30195934361348));
#30482=CARTESIAN_POINT('Ctrl Pts',(86.8780322420958,-6.25040525058881,3.60219296582281));
#30483=CARTESIAN_POINT('Ctrl Pts',(86.9352564373809,-6.72974280712868,1.66644854403002));
#30484=CARTESIAN_POINT('Ctrl Pts',(86.9513537370519,-6.86458158035632,1.12191912096348));
#30485=CARTESIAN_POINT('Ctrl Pts',(86.9674510367229,-6.93300000000024,0.560975745774675));
#30486=CARTESIAN_POINT('Ctrl Pts',(86.9835483363939,-6.933,-2.90281687576055E-12));
#30487=CARTESIAN_POINT('Origin',(29.75,0.,0.));
#30488=CARTESIAN_POINT('',(88.4128916636062,-6.935505181738,-0.00110020350931883));
#30489=CARTESIAN_POINT('',(88.2335483363938,-6.94458427852422,-0.00039025483562369));
#30490=CARTESIAN_POINT('',(29.75,-6.933,-8.4904762584886E-16));
#30491=CARTESIAN_POINT('Ctrl Pts',(88.4128916636062,-6.935505181738,-0.00110020350931883));
#30492=CARTESIAN_POINT('Ctrl Pts',(88.3827735543372,-6.93378070856149,1.04526965719805));
#30493=CARTESIAN_POINT('Ctrl Pts',(88.3526554450683,-6.68734941614985,2.09265228946978));
#30494=CARTESIAN_POINT('Ctrl Pts',(88.3225373357993,-6.2276382020042,3.03870790965906));
#30495=CARTESIAN_POINT('Ctrl Pts',(88.2894520683923,-5.72263742940609,4.07796647985569));
#30496=CARTESIAN_POINT('Ctrl Pts',(88.2563668009853,-4.96026313710671,4.99494964068218));
#30497=CARTESIAN_POINT('Ctrl Pts',(88.2232815335783,-4.02072362537253,5.65864104328076));
#30498=CARTESIAN_POINT('Ctrl Pts',(88.1571109987643,-2.14164460190385,6.98602384847814));
#30499=CARTESIAN_POINT('Ctrl Pts',(88.0909404639502,0.446095299304411,7.30023962076365));
#30500=CARTESIAN_POINT('Ctrl Pts',(88.0247699291362,2.57513936872885,6.44971172614812));
#30501=CARTESIAN_POINT('Ctrl Pts',(87.9585993943221,4.70418343815292,5.59918383153274));
#30502=CARTESIAN_POINT('Ctrl Pts',(87.8924288595081,6.37453167579348,3.5839122700167));
#30503=CARTESIAN_POINT('Ctrl Pts',(87.8262583246941,6.81602776252033,1.33042485154879));
#30504=CARTESIAN_POINT('Ctrl Pts',(87.76008778988,7.25752384924726,-0.923062566919503));
#30505=CARTESIAN_POINT('Ctrl Pts',(87.6939172550659,6.47016778506027,-3.41476584233957));
#30506=CARTESIAN_POINT('Ctrl Pts',(87.6277467202519,4.81396388596147,-5.00539873034359));
#30507=CARTESIAN_POINT('Ctrl Pts',(87.5615761854379,3.15775998686276,-6.59603161834753));
#30508=CARTESIAN_POINT('Ctrl Pts',(87.4954056506239,0.632708252852293,-7.28559411893525));
#30509=CARTESIAN_POINT('Ctrl Pts',(87.4292351158099,-1.59848315555634,-6.75832639935306));
#30510=CARTESIAN_POINT('Ctrl Pts',(87.3630645809958,-3.82967456396472,-6.23105867977093));
#30511=CARTESIAN_POINT('Ctrl Pts',(87.2968940461817,-5.76700564677146,-4.48696074001916));
#30512=CARTESIAN_POINT('Ctrl Pts',(87.2307235113677,-6.54217468998849,-2.32085916289729));
#30513=CARTESIAN_POINT('Ctrl Pts',(87.2081128954472,-6.80705164101982,-1.58069753442065));
#30514=CARTESIAN_POINT('Ctrl Pts',(87.1855022795267,-6.93623411182673,-0.79126260129709));
#30515=CARTESIAN_POINT('Ctrl Pts',(87.1628916636062,-6.93279839181025,-0.00148945332221512));
#30516=CARTESIAN_POINT('Ctrl Pts',(86.9835483363939,-6.92663006290457,-0.00828746050336714));
#30517=CARTESIAN_POINT('Ctrl Pts',(87.0047897084878,-6.93231836757728,-0.750014360114233));
#30518=CARTESIAN_POINT('Ctrl Pts',(87.0260310805816,-6.82278736112151,-1.48975226235973));
#30519=CARTESIAN_POINT('Ctrl Pts',(87.0472724526755,-6.59102457491306,-2.18826853280899));
#30520=CARTESIAN_POINT('Ctrl Pts',(87.1134429874895,-5.86904355383633,-4.36426709766948));
#30521=CARTESIAN_POINT('Ctrl Pts',(87.1796135223035,-3.96088883031357,-6.1402386343094));
#30522=CARTESIAN_POINT('Ctrl Pts',(87.2457840571176,-1.73486522229777,-6.72135995084269));
#30523=CARTESIAN_POINT('Ctrl Pts',(87.2788693245246,-0.62185341828987,-7.01192060910934));
#30524=CARTESIAN_POINT('Ctrl Pts',(87.3119545919317,0.570625606841345,-7.00376871234934));
#30525=CARTESIAN_POINT('Ctrl Pts',(87.3450398593387,1.69070331343781,-6.72002571730325));
#30526=CARTESIAN_POINT('Ctrl Pts',(87.3781251267457,2.81078102003415,-6.43628272225719));
#30527=CARTESIAN_POINT('Ctrl Pts',(87.4112103941527,3.85845740809585,-5.87694862892509));
#30528=CARTESIAN_POINT('Ctrl Pts',(87.4442956615597,4.70315627451569,-5.0976131527676));
#30529=CARTESIAN_POINT('Ctrl Pts',(87.4773809289667,5.54785514093573,-4.31827767660994));
#30530=CARTESIAN_POINT('Ctrl Pts',(87.5104661963738,6.18957648571371,-3.3189408176271));
#30531=CARTESIAN_POINT('Ctrl Pts',(87.5435514637808,6.5624166537896,-2.22528896940409));
#30532=CARTESIAN_POINT('Ctrl Pts',(87.5766367311878,6.93525682186541,-1.13163712118134));
#30533=CARTESIAN_POINT('Ctrl Pts',(87.6097219985948,7.03921581323902,0.0563297162812662));
#30534=CARTESIAN_POINT('Ctrl Pts',(87.6428072660018,6.83904205674447,1.18909237421267));
#30535=CARTESIAN_POINT('Ctrl Pts',(87.7089778008158,6.43869454375532,3.45461769007573));
#30536=CARTESIAN_POINT('Ctrl Pts',(87.7751483356299,4.8218160392931,5.49932628781417));
#30537=CARTESIAN_POINT('Ctrl Pts',(87.8413188704439,2.71087765477093,6.39384598341667));
#30538=CARTESIAN_POINT('Ctrl Pts',(87.907489405258,0.599939270248752,7.28836567901917));
#30539=CARTESIAN_POINT('Ctrl Pts',(87.9736599400721,-2.00505899433351,7.0326964724858));
#30540=CARTESIAN_POINT('Ctrl Pts',(88.0398304748861,-3.90489207377941,5.74282880096571));
#30541=CARTESIAN_POINT('Ctrl Pts',(88.1044030953886,-5.75884717331272,4.48410940439889));
#30542=CARTESIAN_POINT('Ctrl Pts',(88.1689757158912,-6.94128313269814,2.24053698532216));
#30543=CARTESIAN_POINT('Ctrl Pts',(88.2335483363938,-6.94458427852422,-0.00039025483562369));
#30544=CARTESIAN_POINT('Origin',(29.75,0.,0.));
#30545=CARTESIAN_POINT('',(89.6628916636062,-6.93366901110661,0.000560428832954156));
#30546=CARTESIAN_POINT('',(89.4835483363938,-6.93167766374453,0.00562466873832855));
#30547=CARTESIAN_POINT('',(29.75,-6.933,-8.4904762584886E-16));
#30548=CARTESIAN_POINT('Ctrl Pts',(89.6628916636062,-6.93602175126458,0.00253131295903153));
#30549=CARTESIAN_POINT('Ctrl Pts',(89.6462153639618,-6.93907490126647,0.584461471238139));
#30550=CARTESIAN_POINT('Ctrl Pts',(89.6295390643174,-6.86919820701986,1.1657362249708));
#30551=CARTESIAN_POINT('Ctrl Pts',(89.612862764673,-6.72340785284693,1.72691162848786));
#30552=CARTESIAN_POINT('Ctrl Pts',(89.5466922298589,-6.14492066371759,3.95362123236213));
#30553=CARTESIAN_POINT('Ctrl Pts',(89.480521695045,-4.37120800409507,5.86387586171152));
#30554=CARTESIAN_POINT('Ctrl Pts',(89.4143511602309,-2.19606517438035,6.58843091097293));
#30555=CARTESIAN_POINT('Ctrl Pts',(89.3481806254169,-0.020922344665516,
7.31298596023438));
#30556=CARTESIAN_POINT('Ctrl Pts',(89.2820100906029,2.55565065514142,6.85184142940768));
#30557=CARTESIAN_POINT('Ctrl Pts',(89.2158395557888,4.34737921445182,5.41558479859921));
#30558=CARTESIAN_POINT('Ctrl Pts',(89.1496690209748,6.13910777376212,3.97932816779082));
#30559=CARTESIAN_POINT('Ctrl Pts',(89.0834984861608,7.14599189257585,1.56795943700085));
#30560=CARTESIAN_POINT('Ctrl Pts',(89.0173279513468,6.90765202347533,-0.715966666573044));
#30561=CARTESIAN_POINT('Ctrl Pts',(88.9511574165327,6.66931215437481,-2.99989277014694));
#30562=CARTESIAN_POINT('Ctrl Pts',(88.8849868817187,5.18574829735977,-5.15637624650502));
#30563=CARTESIAN_POINT('Ctrl Pts',(88.8188163469046,3.14123319515043,-6.19376929926154));
#30564=CARTESIAN_POINT('Ctrl Pts',(88.7526458120905,1.0967180929411,-7.23116235201807));
#30565=CARTESIAN_POINT('Ctrl Pts',(88.6864752772765,-1.50874825446258,-7.14946498117337));
#30566=CARTESIAN_POINT('Ctrl Pts',(88.6203047424625,-3.49893401082527,-5.99532298681402));
#30567=CARTESIAN_POINT('Ctrl Pts',(88.5872194750555,-4.49402688900667,-5.41825198963431));
#30568=CARTESIAN_POINT('Ctrl Pts',(88.5541342076485,-5.33529961942776,-4.57306983657593));
#30569=CARTESIAN_POINT('Ctrl Pts',(88.5210489402415,-5.93115617306285,-3.58310058273908));
#30570=CARTESIAN_POINT('Ctrl Pts',(88.4879636728344,-6.52701272669794,-2.59313132890222));
#30571=CARTESIAN_POINT('Ctrl Pts',(88.4548784054274,-6.87745310354699,-1.45837497428694));
#30572=CARTESIAN_POINT('Ctrl Pts',(88.4217931380204,-6.9288596655231,-0.3102298071958));
#30573=CARTESIAN_POINT('Ctrl Pts',(88.4188259798823,-6.93346991687278,-0.207261672336488));
#30574=CARTESIAN_POINT('Ctrl Pts',(88.4158588217443,-6.93567507237004,-0.104185852741362));
#30575=CARTESIAN_POINT('Ctrl Pts',(88.4128916636062,-6.935505181738,-0.00110020350931883));
#30576=CARTESIAN_POINT('Ctrl Pts',(88.2335483363938,-6.94458427852422,-0.00039025483562369));
#30577=CARTESIAN_POINT('Ctrl Pts',(88.2351462507052,-6.94466596869133,-0.0558442488051521));
#30578=CARTESIAN_POINT('Ctrl Pts',(88.2367441650167,-6.94402559831809,-0.111296622960476));
#30579=CARTESIAN_POINT('Ctrl Pts',(88.2383420793281,-6.94265547521014,-0.166732413169323));
#30580=CARTESIAN_POINT('Ctrl Pts',(88.3045126141421,-6.88591790288544,-2.46235981927781));
#30581=CARTESIAN_POINT('Ctrl Pts',(88.3706831489563,-5.57777486392631,-4.72954849498799));
#30582=CARTESIAN_POINT('Ctrl Pts',(88.4368536837703,-3.62182626347297,-5.92558002528084));
#30583=CARTESIAN_POINT('Ctrl Pts',(88.5030242185843,-1.66587766301974,-7.12161155557361));
#30584=CARTESIAN_POINT('Ctrl Pts',(88.5691947533982,0.937876498927613,-7.24648594044916));
#30585=CARTESIAN_POINT('Ctrl Pts',(88.6353652882123,3.01320420398057,-6.25356197326325));
#30586=CARTESIAN_POINT('Ctrl Pts',(88.6684505556194,4.05086805650711,-5.75709998967027));
#30587=CARTESIAN_POINT('Ctrl Pts',(88.7015358230265,4.95642529481004,-4.98118841806188));
#30588=CARTESIAN_POINT('Ctrl Pts',(88.7346210904335,5.62880203099263,-4.04151098367676));
#30589=CARTESIAN_POINT('Ctrl Pts',(88.7677063578405,6.30117876717522,-3.10183354929164));
#30590=CARTESIAN_POINT('Ctrl Pts',(88.8007916252474,6.74037500123749,-1.99839025212978));
#30591=CARTESIAN_POINT('Ctrl Pts',(88.8338768926544,6.88253661774944,-0.857921035482686));
#30592=CARTESIAN_POINT('Ctrl Pts',(88.8669621600615,7.02469823426139,0.282548181164276));
#30593=CARTESIAN_POINT('Ctrl Pts',(88.9000474274686,6.86982523322309,1.46004331729646));
#30594=CARTESIAN_POINT('Ctrl Pts',(88.9331326948756,6.44870444968859,2.53602725849965));
#30595=CARTESIAN_POINT('Ctrl Pts',(88.9662179622827,6.02758366615408,3.61201119970284));
#30596=CARTESIAN_POINT('Ctrl Pts',(88.9993032296895,5.34021510012337,4.58648394597703));
#30597=CARTESIAN_POINT('Ctrl Pts',(89.0323884970965,4.45618059126846,5.32248921711756));
#30598=CARTESIAN_POINT('Ctrl Pts',(89.0985590319105,2.68811157355832,6.79449975939887));
#30599=CARTESIAN_POINT('Ctrl Pts',(89.1647295667247,0.133378784551066,7.31264040114517));
#30600=CARTESIAN_POINT('Ctrl Pts',(89.2309001015388,-2.05632936253286,6.63337272219608));
#30601=CARTESIAN_POINT('Ctrl Pts',(89.2970706363528,-4.24603750961654,5.95410504324707));
#30602=CARTESIAN_POINT('Ctrl Pts',(89.3632411711668,-6.07072101477698,4.07742904360294));
#30603=CARTESIAN_POINT('Ctrl Pts',(89.4294117059808,-6.68927433964374,1.86597790824286));
#30604=CARTESIAN_POINT('Ctrl Pts',(89.4474572494518,-6.85796167071017,1.26288715630475));
#30605=CARTESIAN_POINT('Ctrl Pts',(89.4655027929228,-6.93694644387414,0.634898440211108));
#30606=CARTESIAN_POINT('Ctrl Pts',(89.4835483363938,-6.93167766374453,0.00562466873832855));
#30607=CARTESIAN_POINT('Origin',(29.75,0.,0.));
#30608=CARTESIAN_POINT('',(90.9128916636062,-6.92718184132294,0.00080019213586006));
#30609=CARTESIAN_POINT('',(90.7335483363939,-6.92146317547543,-0.000963293967941629));
#30610=CARTESIAN_POINT('',(29.75,-6.933,-8.4904762584886E-16));
#30611=CARTESIAN_POINT('Ctrl Pts',(90.9128916636062,-6.933,3.81528142412435E-12));
#30612=CARTESIAN_POINT('Ctrl Pts',(90.8556674683211,-6.9329999999989,1.99420935702016));
#30613=CARTESIAN_POINT('Ctrl Pts',(90.798443273036,-6.02307502629025,3.97063309653389));
#30614=CARTESIAN_POINT('Ctrl Pts',(90.7412190777509,-4.5079848475368,5.26731066241385));
#30615=CARTESIAN_POINT('Ctrl Pts',(90.6839948824658,-2.99289466878335,6.56398822829381));
#30616=CARTESIAN_POINT('Ctrl Pts',(90.6267706871807,-0.899664345624515,
7.15779044292466));
#30617=CARTESIAN_POINT('Ctrl Pts',(90.5695464918956,1.07062371682261,6.84983604599241));
#30618=CARTESIAN_POINT('Ctrl Pts',(90.5123222966105,3.04091177926973,6.54188164906017));
#30619=CARTESIAN_POINT('Ctrl Pts',(90.4550981013254,4.85311303640217,5.33766370386098));
#30620=CARTESIAN_POINT('Ctrl Pts',(90.3978739060403,5.90026971493993,3.64050907030359));
#30621=CARTESIAN_POINT('Ctrl Pts',(90.3406497107552,6.94742639347769,1.94335443674621));
#30622=CARTESIAN_POINT('Ctrl Pts',(90.2834255154701,7.21086008527498,-0.216464293128636));
#30623=CARTESIAN_POINT('Ctrl Pts',(90.226201320185,6.60233935005942,-2.11556236179814));
#30624=CARTESIAN_POINT('Ctrl Pts',(90.1689771248999,5.99381861484387,-4.01466043046765));
#30625=CARTESIAN_POINT('Ctrl Pts',(90.1117529296148,4.52419779646915,-5.61916312790751));
#30626=CARTESIAN_POINT('Ctrl Pts',(90.0545287343297,2.68569472999963,-6.39167683923806));
#30627=CARTESIAN_POINT('Ctrl Pts',(89.9973045390446,0.847191663530109,-7.16419055056861));
#30628=CARTESIAN_POINT('Ctrl Pts',(89.9400803437595,-1.32739978994672,-7.09093574623695));
#30629=CARTESIAN_POINT('Ctrl Pts',(89.8828561484744,-3.10974706736635,-6.19644754492495));
#30630=CARTESIAN_POINT('Ctrl Pts',(89.8256319531893,-4.89209434478598,-5.30195934361295));
#30631=CARTESIAN_POINT('Ctrl Pts',(89.7684077579042,-6.25040525058921,-3.60219296582212));
#30632=CARTESIAN_POINT('Ctrl Pts',(89.7111835626191,-6.72974280712887,-1.66644854402927));
#30633=CARTESIAN_POINT('Ctrl Pts',(89.6950862629482,-6.86458158035644,-1.12191912096272));
#30634=CARTESIAN_POINT('Ctrl Pts',(89.6789889632772,-6.9330000000003,-0.560975745773912));
#30635=CARTESIAN_POINT('Ctrl Pts',(89.6628916636062,-6.933,3.66595642731227E-12));
#30636=CARTESIAN_POINT('Ctrl Pts',(89.4835483363938,-6.93167766374453,0.00562466873832855));
#30637=CARTESIAN_POINT('Ctrl Pts',(89.5316733277368,-6.91762654921127,-1.67256223946896));
#30638=CARTESIAN_POINT('Ctrl Pts',(89.5797983190799,-6.30435085090587,-3.35988866458186));
#30639=CARTESIAN_POINT('Ctrl Pts',(89.6279233104229,-5.19520266043836,-4.60848500724921));
#30640=CARTESIAN_POINT('Ctrl Pts',(89.694093845237,-3.6701545117932,-6.3252705163049));
#30641=CARTESIAN_POINT('Ctrl Pts',(89.7602643800511,-1.20763506992989,-7.21261526334011));
#30642=CARTESIAN_POINT('Ctrl Pts',(89.8264349148651,1.05830213661075,-6.86368127949098));
#30643=CARTESIAN_POINT('Ctrl Pts',(89.8926054496791,3.32423934315126,-6.51474729564187));
#30644=CARTESIAN_POINT('Ctrl Pts',(89.9587759844931,5.39359431436911,-4.92953458090855));
#30645=CARTESIAN_POINT('Ctrl Pts',(90.0249465193072,6.33785313441409,-2.83161695413198));
#30646=CARTESIAN_POINT('Ctrl Pts',(90.0580317867142,6.80998254443662,-1.78265814074363));
#30647=CARTESIAN_POINT('Ctrl Pts',(90.0911170541212,7.00083791666589,-0.605523099344461));
#30648=CARTESIAN_POINT('Ctrl Pts',(90.1242023215282,6.90788674366042,0.546190508931948));
#30649=CARTESIAN_POINT('Ctrl Pts',(90.1572875889352,6.81493557065494,1.69790411720836));
#30650=CARTESIAN_POINT('Ctrl Pts',(90.1903728563423,6.43817785241471,2.824196292362));
#30651=CARTESIAN_POINT('Ctrl Pts',(90.2234581237493,5.81064588145672,3.7870480902803));
#30652=CARTESIAN_POINT('Ctrl Pts',(90.2565433911563,5.18311391049873,4.7498998881986));
#30653=CARTESIAN_POINT('Ctrl Pts',(90.2896286585634,4.30480768682298,5.54931130888157));
#30654=CARTESIAN_POINT('Ctrl Pts',(90.3227139259704,3.28866101015077,6.09933866051073));
#30655=CARTESIAN_POINT('Ctrl Pts',(90.3557991933774,2.27251433347868,6.64936601213983));
#30656=CARTESIAN_POINT('Ctrl Pts',(90.3888844607844,1.11852720381016,6.95000929471518));
#30657=CARTESIAN_POINT('Ctrl Pts',(90.4219697281914,-0.0317551929082471,
6.94157248295037));
#30658=CARTESIAN_POINT('Ctrl Pts',(90.4881402630053,-2.33231998634532,6.92469885942073));
#30659=CARTESIAN_POINT('Ctrl Pts',(90.5543107978194,-4.61806584798195,5.67150485853014));
#30660=CARTESIAN_POINT('Ctrl Pts',(90.6204813326335,-5.8521381065398,3.73933198589997));
#30661=CARTESIAN_POINT('Ctrl Pts',(90.658170333887,-6.55503330045561,2.63881699047063));
#30662=CARTESIAN_POINT('Ctrl Pts',(90.6958593351404,-6.91675055518297,1.31803155035726));
#30663=CARTESIAN_POINT('Ctrl Pts',(90.7335483363939,-6.92146317547543,-0.000963293967941629));
#30664=CARTESIAN_POINT('Origin',(29.75,0.,0.));
#30665=CARTESIAN_POINT('',(92.1628916636062,-6.93839386646797,-0.00802539788412049));
#30666=CARTESIAN_POINT('',(91.9835483363938,-6.93565096779518,-0.0017588741014353));
#30667=CARTESIAN_POINT('',(29.75,-6.933,-8.4904762584886E-16));
#30668=CARTESIAN_POINT('Ctrl Pts',(92.1628916636062,-6.93839386646797,-0.00802539788412049));
#30669=CARTESIAN_POINT('Ctrl Pts',(92.1069284483969,-6.92141512853983,1.93686533832047));
#30670=CARTESIAN_POINT('Ctrl Pts',(92.0509652331876,-6.06505943965661,3.89823190017224));
#30671=CARTESIAN_POINT('Ctrl Pts',(91.9950020179784,-4.61462848763626,5.18974649343901));
#30672=CARTESIAN_POINT('Ctrl Pts',(91.9288314831643,-2.89964854148488,6.71682479008534));
#30673=CARTESIAN_POINT('Ctrl Pts',(91.8626609483504,-0.354119244346323,
7.30741380281861));
#30674=CARTESIAN_POINT('Ctrl Pts',(91.7964904135363,1.85806218476672,6.69147739012891));
#30675=CARTESIAN_POINT('Ctrl Pts',(91.7303198787223,4.07024361387963,6.07554097743925));
#30676=CARTESIAN_POINT('Ctrl Pts',(91.6641493439082,5.94907717496707,4.25307913932677));
#30677=CARTESIAN_POINT('Ctrl Pts',(91.5979788090942,6.63093513249416,2.06417620067773));
#30678=CARTESIAN_POINT('Ctrl Pts',(91.5318082742801,7.3127930900213,-0.124726737971427));
#30679=CARTESIAN_POINT('Ctrl Pts',(91.4656377394661,6.79767544398795,-2.68007077715719));
#30680=CARTESIAN_POINT('Ctrl Pts',(91.3994672046521,5.3277578235197,-4.44988016717922));
#30681=CARTESIAN_POINT('Ctrl Pts',(91.366381937245,4.59279901328558,-5.33478486219024));
#30682=CARTESIAN_POINT('Ctrl Pts',(91.333296669838,3.61914020944273,-6.02330589491032));
#30683=CARTESIAN_POINT('Ctrl Pts',(91.300211402431,2.54365527055743,-6.44569943449522));
#30684=CARTESIAN_POINT('Ctrl Pts',(91.267126135024,1.46817033167227,-6.86809297408008));
#30685=CARTESIAN_POINT('Ctrl Pts',(91.2340408676171,0.290859257744679,-7.02435902052981));
#30686=CARTESIAN_POINT('Ctrl Pts',(91.20095560021,-0.849777359231778,-6.88354685010008));
#30687=CARTESIAN_POINT('Ctrl Pts',(91.167870332803,-1.99041397620836,-6.74273467967033));
#30688=CARTESIAN_POINT('Ctrl Pts',(91.1347850653959,-3.09437613623381,-6.30484429236105));
#30689=CARTESIAN_POINT('Ctrl Pts',(91.1016997979888,-4.03484843570422,-5.63357980649799));
#30690=CARTESIAN_POINT('Ctrl Pts',(91.0686145305818,-4.97532073517462,-4.96231532063492));
#30691=CARTESIAN_POINT('Ctrl Pts',(91.0355292631749,-5.75230317408999,-4.05767673621806));
#30692=CARTESIAN_POINT('Ctrl Pts',(91.0024439957679,-6.24999252257306,-3.02060099915746));
#30693=CARTESIAN_POINT('Ctrl Pts',(90.9725932183807,-6.6990266430109,-2.08491211443893));
#30694=CARTESIAN_POINT('Ctrl Pts',(90.9427424409935,-6.9207069805332,-1.04141502148469));
#30695=CARTESIAN_POINT('Ctrl Pts',(90.9128916636062,-6.91918773061192,0.00189965071867138));
#30696=CARTESIAN_POINT('Ctrl Pts',(90.7335483363939,-6.92146317547543,-0.000963293967941629));
#30697=CARTESIAN_POINT('Ctrl Pts',(90.7620298699545,-6.92502449704284,-0.997726133934744));
#30698=CARTESIAN_POINT('Ctrl Pts',(90.7905114035151,-6.72470736279399,-1.99346639920903));
#30699=CARTESIAN_POINT('Ctrl Pts',(90.8189929370756,-6.31368152489429,-2.8923503154485));
#30700=CARTESIAN_POINT('Ctrl Pts',(90.8851634718897,-5.35875402921189,-4.98070799979733));
#30701=CARTESIAN_POINT('Ctrl Pts',(90.9513340067037,-3.26650038236796,-6.54627162412541));
#30702=CARTESIAN_POINT('Ctrl Pts',(91.0175045415177,-0.993565712653891,
-6.87321554439442));
#30703=CARTESIAN_POINT('Ctrl Pts',(91.0836750763317,1.27936895706031,-7.20015946466345));
#30704=CARTESIAN_POINT('Ctrl Pts',(91.1498456111458,3.73298464964467,-6.2884836808732));
#30705=CARTESIAN_POINT('Ctrl Pts',(91.2160161459598,5.23849463787312,-4.55941860852503));
#30706=CARTESIAN_POINT('Ctrl Pts',(91.2821866807739,6.74400462610157,-2.83035353617686));
#30707=CARTESIAN_POINT('Ctrl Pts',(91.348357215588,7.30140890997411,-0.283899175270764));
#30708=CARTESIAN_POINT('Ctrl Pts',(91.414527750402,6.66853635908363,1.92796777875305));
#30709=CARTESIAN_POINT('Ctrl Pts',(91.447613017809,6.35210008363843,3.03390125576483));
#30710=CARTESIAN_POINT('Ctrl Pts',(91.480698285216,5.73809459950255,4.05618788105605));
#30711=CARTESIAN_POINT('Ctrl Pts',(91.513783552623,4.92372512177406,4.87587471747353));
#30712=CARTESIAN_POINT('Ctrl Pts',(91.54686882003,4.10935564404549,5.69556155389111));
#30713=CARTESIAN_POINT('Ctrl Pts',(91.579954087437,3.09462217272427,6.31264860143489));
#30714=CARTESIAN_POINT('Ctrl Pts',(91.613039354844,1.99383914151695,6.64303727789786));
#30715=CARTESIAN_POINT('Ctrl Pts',(91.6461246222511,0.893056110309632,6.97342595436083));
#30716=CARTESIAN_POINT('Ctrl Pts',(91.6792098896581,-0.293776480783792,
7.01711625974298));
#30717=CARTESIAN_POINT('Ctrl Pts',(91.7122951570651,-1.4249271508334,6.78135723510452));
#30718=CARTESIAN_POINT('Ctrl Pts',(91.7453804244721,-2.55607782088288,6.54559821046609));
#30719=CARTESIAN_POINT('Ctrl Pts',(91.7784656918791,-3.63154656988856,6.03038985580711));
#30720=CARTESIAN_POINT('Ctrl Pts',(91.8115509592862,-4.50469000490483,5.28149646293935));
#30721=CARTESIAN_POINT('Ctrl Pts',(91.868883418322,-6.0177338502121,3.98376175701588));
#30722=CARTESIAN_POINT('Ctrl Pts',(91.9262158773579,-6.92322764173258,1.98430883930039));
#30723=CARTESIAN_POINT('Ctrl Pts',(91.9835483363938,-6.94004001014585,-0.0046709324541017));
#30724=CARTESIAN_POINT('Origin',(29.75,0.,0.));
#30725=CARTESIAN_POINT('',(93.4128916636062,-6.93875336632197,0.00522259790129709));
#30726=CARTESIAN_POINT('',(93.2335483363939,-6.93307491442268,0.000658892883751194));
#30727=CARTESIAN_POINT('',(29.75,-6.933,-8.4904762584886E-16));
#30728=CARTESIAN_POINT('Ctrl Pts',(93.4128916636062,-6.93875336632197,0.00522259790129709));
#30729=CARTESIAN_POINT('Ctrl Pts',(93.4034555254285,-6.94167326281239,0.333422550527998));
#30730=CARTESIAN_POINT('Ctrl Pts',(93.3940193872508,-6.92062603608355,0.661249996353714));
#30731=CARTESIAN_POINT('Ctrl Pts',(93.3845832490732,-6.8743862713196,0.985432969693625));
#30732=CARTESIAN_POINT('Ctrl Pts',(93.3184127142592,-6.55013180339034,3.25875287235075));
#30733=CARTESIAN_POINT('Ctrl Pts',(93.2522421794451,-4.98704472552019,5.35285735196643));
#30734=CARTESIAN_POINT('Ctrl Pts',(93.1860716446311,-2.89981832568375,6.31025502044848));
#30735=CARTESIAN_POINT('Ctrl Pts',(93.1199011098171,-0.812591925847067,
7.26765268893064));
#30736=CARTESIAN_POINT('Ctrl Pts',(93.053730575003,1.79877379595603,7.08834354627892));
#30737=CARTESIAN_POINT('Ctrl Pts',(92.9875600401889,3.73240540926872,5.85655820253256));
#30738=CARTESIAN_POINT('Ctrl Pts',(92.9213895053749,5.66603702258108,4.6247728587864));
#30739=CARTESIAN_POINT('Ctrl Pts',(92.8552189705608,6.92193452740331,2.34051131394602));
#30740=CARTESIAN_POINT('Ctrl Pts',(92.7890484357468,6.9415300532182,0.0399680947605974));
#30741=CARTESIAN_POINT('Ctrl Pts',(92.7559631683398,6.95132781612565,-1.11030351483225));
#30742=CARTESIAN_POINT('Ctrl Pts',(92.7228779009328,6.6520500842812,-2.26464554301135));
#30743=CARTESIAN_POINT('Ctrl Pts',(92.6897926335258,6.103225371949,-3.28144227352618));
#30744=CARTESIAN_POINT('Ctrl Pts',(92.6567073661188,5.55440065961681,-4.29823900404101));
#30745=CARTESIAN_POINT('Ctrl Pts',(92.6236220987117,4.75602896679687,-5.17749043689156));
#30746=CARTESIAN_POINT('Ctrl Pts',(92.5905368313047,3.79392030748638,-5.80616116709036));
#30747=CARTESIAN_POINT('Ctrl Pts',(92.5574515638977,2.83181164817599,-6.43483189728908));
#30748=CARTESIAN_POINT('Ctrl Pts',(92.5243662964907,1.70596602237508,-6.81292192483611));
#30749=CARTESIAN_POINT('Ctrl Pts',(92.4912810290837,0.554363195424337,-6.90723568316918));
#30750=CARTESIAN_POINT('Ctrl Pts',(92.4581957616767,-0.597239631526407,
-7.00154944150225));
#30751=CARTESIAN_POINT('Ctrl Pts',(92.4251104942697,-1.77459965962699,-6.81208693062137));
#30752=CARTESIAN_POINT('Ctrl Pts',(92.3920252268626,-2.8241163389132,-6.34119892706528));
#30753=CARTESIAN_POINT('Ctrl Pts',(92.3258546920486,-4.92314969748599,-5.39942291995293));
#30754=CARTESIAN_POINT('Ctrl Pts',(92.2596841572346,-6.51080966080111,-3.33194494213933));
#30755=CARTESIAN_POINT('Ctrl Pts',(92.1935136224205,-6.86242434487645,-1.06642216295277));
#30756=CARTESIAN_POINT('Ctrl Pts',(92.1833063028158,-6.91666364441026,-0.716947655242347));
#30757=CARTESIAN_POINT('Ctrl Pts',(92.173098983211,-6.94149067575369,-0.362760580031751));
#30758=CARTESIAN_POINT('Ctrl Pts',(92.1628916636062,-6.93839386646797,-0.00802539788412049));
#30759=CARTESIAN_POINT('Ctrl Pts',(91.9835483363938,-6.933,-2.3049617769999E-12));
#30760=CARTESIAN_POINT('Ctrl Pts',(92.0407725316789,-6.93299999999934,-1.99420935701865));
#30761=CARTESIAN_POINT('Ctrl Pts',(92.097996726964,-6.02307502629111,-3.97063309653258));
#30762=CARTESIAN_POINT('Ctrl Pts',(92.1552209222491,-4.50798484753795,-5.26731066241287));
#30763=CARTESIAN_POINT('Ctrl Pts',(92.2124451175342,-2.99289466878478,-6.56398822829316));
#30764=CARTESIAN_POINT('Ctrl Pts',(92.2696693128193,-0.899664345626074,
-7.15779044292446));
#30765=CARTESIAN_POINT('Ctrl Pts',(92.3268935081044,1.07062371682111,-6.84983604599264));
#30766=CARTESIAN_POINT('Ctrl Pts',(92.3841177033895,3.0409117792683,-6.54188164906083));
#30767=CARTESIAN_POINT('Ctrl Pts',(92.4413418986746,4.853113036401,-5.33766370386204));
#30768=CARTESIAN_POINT('Ctrl Pts',(92.4985660939597,5.90026971493913,-3.64050907030488));
#30769=CARTESIAN_POINT('Ctrl Pts',(92.5557902892448,6.94742639347726,-1.94335443674772));
#30770=CARTESIAN_POINT('Ctrl Pts',(92.6130144845299,7.21086008527502,0.216464293127065));
#30771=CARTESIAN_POINT('Ctrl Pts',(92.670238679815,6.60233935005988,2.11556236179671));
#30772=CARTESIAN_POINT('Ctrl Pts',(92.7274628751001,5.99381861484474,4.01466043046635));
#30773=CARTESIAN_POINT('Ctrl Pts',(92.7846870703852,4.52419779647037,5.61916312790652));
#30774=CARTESIAN_POINT('Ctrl Pts',(92.8419112656703,2.68569473000102,6.39167683923747));
#30775=CARTESIAN_POINT('Ctrl Pts',(92.8991354609554,0.847191663531669,7.16419055056843));
#30776=CARTESIAN_POINT('Ctrl Pts',(92.9563596562405,-1.32739978994518,7.09093574623724));
#30777=CARTESIAN_POINT('Ctrl Pts',(93.0135838515256,-3.109747067365,6.19644754492562));
#30778=CARTESIAN_POINT('Ctrl Pts',(93.0708080468107,-4.89209434478482,5.30195934361401));
#30779=CARTESIAN_POINT('Ctrl Pts',(93.1280322420958,-6.25040525058842,3.60219296582348));
#30780=CARTESIAN_POINT('Ctrl Pts',(93.1852564373809,-6.7297428071285,1.66644854403074));
#30781=CARTESIAN_POINT('Ctrl Pts',(93.2013537370519,-6.86458158035613,1.12191912096447));
#30782=CARTESIAN_POINT('Ctrl Pts',(93.2174510367228,-6.93300000000011,0.560975745775948));
#30783=CARTESIAN_POINT('Ctrl Pts',(93.2335483363938,-6.933,-1.36723965482588E-12));
#30784=CARTESIAN_POINT('Origin',(29.75,0.,0.));
#30785=CARTESIAN_POINT('',(94.6628916636061,-6.92404070110412,0.00207036192589771));
#30786=CARTESIAN_POINT('',(94.4835483363939,-6.92908201353558,0.00220150041010815));
#30787=CARTESIAN_POINT('',(29.75,-6.933,-8.4904762584886E-16));
#30788=CARTESIAN_POINT('Ctrl Pts',(94.6628916636061,-6.92404070110412,0.00207036192589771));
#30789=CARTESIAN_POINT('Ctrl Pts',(94.6338120676461,-6.92690635206978,1.01894162261975));
#30790=CARTESIAN_POINT('Ctrl Pts',(94.604732471686,-6.71688041784802,2.03469379117756));
#30791=CARTESIAN_POINT('Ctrl Pts',(94.5756528757259,-6.28784118309068,2.94810413677931));
#30792=CARTESIAN_POINT('Ctrl Pts',(94.5094823409118,-5.31156367018941,5.02656668337304));
#30793=CARTESIAN_POINT('Ctrl Pts',(94.4433118060977,-3.20126007432825,6.57511485341535));
#30794=CARTESIAN_POINT('Ctrl Pts',(94.3771412712837,-0.929291360962711,
6.88233548188621));
#30795=CARTESIAN_POINT('Ctrl Pts',(94.3109707364697,1.3426773524027,7.18955611035705));
#30796=CARTESIAN_POINT('Ctrl Pts',(94.2448002016557,3.77631118327259,6.2554491972566));
#30797=CARTESIAN_POINT('Ctrl Pts',(94.1786296668417,5.27616304063658,4.51093565648535));
#30798=CARTESIAN_POINT('Ctrl Pts',(94.1455443994346,6.02608896931861,3.63867888609968));
#30799=CARTESIAN_POINT('Ctrl Pts',(94.1124591320276,6.54256940462418,2.56382045879623));
#30800=CARTESIAN_POINT('Ctrl Pts',(94.0793738646205,6.77966658558774,1.43294951884275));
#30801=CARTESIAN_POINT('Ctrl Pts',(94.0462885972135,7.0167637665513,0.302078578889283));
#30802=CARTESIAN_POINT('Ctrl Pts',(94.0132033298066,6.97447769317291,-0.884804873713921));
#30803=CARTESIAN_POINT('Ctrl Pts',(93.9801180623996,6.64539163981147,-1.98597803394435));
#30804=CARTESIAN_POINT('Ctrl Pts',(93.9470327949925,6.31630558644999,-3.0871511941749));
#30805=CARTESIAN_POINT('Ctrl Pts',(93.9139475275855,5.70041955310533,-4.10261406203237));
#30806=CARTESIAN_POINT('Ctrl Pts',(93.8808622601784,4.88169681195711,-4.91795278255235));
#30807=CARTESIAN_POINT('Ctrl Pts',(93.8477769927714,4.06297407080907,-5.73329150307215));
#30808=CARTESIAN_POINT('Ctrl Pts',(93.8146917253644,3.0414146218575,-6.34850607625464));
#30809=CARTESIAN_POINT('Ctrl Pts',(93.7816064579574,1.93585631061123,-6.66625061582574));
#30810=CARTESIAN_POINT('Ctrl Pts',(93.7154359231434,-0.275260311881576,
-7.30173969496801));
#30811=CARTESIAN_POINT('Ctrl Pts',(93.6492653883293,-2.82237238355351,-6.74734863966452));
#30812=CARTESIAN_POINT('Ctrl Pts',(93.5830948535153,-4.55321749039531,-5.24388544916344));
#30813=CARTESIAN_POINT('Ctrl Pts',(93.5263604568789,-6.03723833265783,-3.95482110628342));
#30814=CARTESIAN_POINT('Ctrl Pts',(93.4696260602425,-6.9211976075459,-1.96806625584167));
#30815=CARTESIAN_POINT('Ctrl Pts',(93.4128916636062,-6.93875336632197,0.00522259790129709));
#30816=CARTESIAN_POINT('Ctrl Pts',(93.2335483363938,-6.93338545573979,0.00339018893299717));
#30817=CARTESIAN_POINT('Ctrl Pts',(93.2889134892035,-6.91513820903545,-1.92436519451582));
#30818=CARTESIAN_POINT('Ctrl Pts',(93.3442786420133,-6.08482141908014,-3.85875145648536));
#30819=CARTESIAN_POINT('Ctrl Pts',(93.3996437948231,-4.66302902386902,-5.14648272525469));
#30820=CARTESIAN_POINT('Ctrl Pts',(93.4658143296372,-2.96375143840046,-6.68553504294682));
#30821=CARTESIAN_POINT('Ctrl Pts',(93.5319848644511,-0.419597565822329,
-7.30089166661355));
#30822=CARTESIAN_POINT('Ctrl Pts',(93.5981553992651,1.79877943452019,-6.7076566169575));
#30823=CARTESIAN_POINT('Ctrl Pts',(93.6643259340792,4.01715643486283,-6.11442156730142));
#30824=CARTESIAN_POINT('Ctrl Pts',(93.7304964688933,5.9097565629698,-4.31259484432236));
#30825=CARTESIAN_POINT('Ctrl Pts',(93.7966670037073,6.6112226499871,-2.12602911959458));
#30826=CARTESIAN_POINT('Ctrl Pts',(93.8628375385213,7.3126887370044,0.0605366051331999));
#30827=CARTESIAN_POINT('Ctrl Pts',(93.9290080733354,6.82302078293202,2.63184133160969));
#30828=CARTESIAN_POINT('Ctrl Pts',(93.9951786081494,5.36927895395365,4.40465295266497));
#30829=CARTESIAN_POINT('Ctrl Pts',(94.0613491429634,3.91553712497536,6.17746457372014));
#30830=CARTESIAN_POINT('Ctrl Pts',(94.1275196777775,1.4977214210912,7.1517830893542));
#30831=CARTESIAN_POINT('Ctrl Pts',(94.1936902125915,-0.788719383856762,
6.89669186362991));
#30832=CARTESIAN_POINT('Ctrl Pts',(94.2267754799985,-1.93193978633081,6.76914625076775));
#30833=CARTESIAN_POINT('Ctrl Pts',(94.2598607474055,-3.0423164640708,6.33424820256598));
#30834=CARTESIAN_POINT('Ctrl Pts',(94.2929460148126,-3.98634989426118,5.66800122228379));
#30835=CARTESIAN_POINT('Ctrl Pts',(94.3260312822196,-4.93038332445145,5.00175424200167));
#30836=CARTESIAN_POINT('Ctrl Pts',(94.3591165496266,-5.70807350709216,4.1041583296392));
#30837=CARTESIAN_POINT('Ctrl Pts',(94.3922018170336,-6.21743341290116,3.07389989328311));
#30838=CARTESIAN_POINT('Ctrl Pts',(94.4226506568204,-6.68620454220678,2.12573847504145));
#30839=CARTESIAN_POINT('Ctrl Pts',(94.4530994966071,-6.92770579363022,1.06521479942219));
#30840=CARTESIAN_POINT('Ctrl Pts',(94.4835483363939,-6.92908201353558,0.00220150041010815));
#30841=CARTESIAN_POINT('Origin',(29.75,0.,0.));
#30842=CARTESIAN_POINT('',(95.9128916636062,-6.93006097531607,-0.0057025460704313));
#30843=CARTESIAN_POINT('',(95.7335483363938,-6.93097598691781,-0.00393591295944164));
#30844=CARTESIAN_POINT('',(29.75,-6.933,-8.4904762584886E-16));
#30845=CARTESIAN_POINT('Ctrl Pts',(95.9128916636062,-6.93006097531607,-0.0057025460704313));
#30846=CARTESIAN_POINT('Ctrl Pts',(95.8641686098637,-6.91417425872587,1.69433574802711));
#30847=CARTESIAN_POINT('Ctrl Pts',(95.8154455561211,-6.2837585161334,3.40437531631781));
#30848=CARTESIAN_POINT('Ctrl Pts',(95.7667225023785,-5.15199618764788,4.65693669714884));
#30849=CARTESIAN_POINT('Ctrl Pts',(95.7005519675645,-3.61495544808387,6.35803402357966));
#30850=CARTESIAN_POINT('Ctrl Pts',(95.6343814327504,-1.1532200453151,7.21534852515465));
#30851=CARTESIAN_POINT('Ctrl Pts',(95.5682108979364,1.11836667277205,6.85096291871172));
#30852=CARTESIAN_POINT('Ctrl Pts',(95.5351256305294,2.25416003181581,6.66877011549023));
#30853=CARTESIAN_POINT('Ctrl Pts',(95.5020403631224,3.3424162196891,6.18115228526414));
#30854=CARTESIAN_POINT('Ctrl Pts',(95.4689550957154,4.25343193671011,5.47042412387387));
#30855=CARTESIAN_POINT('Ctrl Pts',(95.4358698283084,5.16444765373091,4.75969596248375));
#30856=CARTESIAN_POINT('Ctrl Pts',(95.4027845609013,5.89822289989943,3.82585746992961));
#30857=CARTESIAN_POINT('Ctrl Pts',(95.3696992934943,6.35761782886665,2.77236980575509));
#30858=CARTESIAN_POINT('Ctrl Pts',(95.3366140260872,6.81701275783391,1.71888214158046));
#30859=CARTESIAN_POINT('Ctrl Pts',(95.3035287586802,7.00202736959979,0.545745305785123));
#30860=CARTESIAN_POINT('Ctrl Pts',(95.2704434912732,6.90294467185206,-0.605457011385599));
#30861=CARTESIAN_POINT('Ctrl Pts',(95.2373582238662,6.80386197410433,-1.75665932855619));
#30862=CARTESIAN_POINT('Ctrl Pts',(95.2042729564592,6.42068196684316,-2.88592712710245));
#30863=CARTESIAN_POINT('Ctrl Pts',(95.1711876890522,5.78134147007617,-3.84220349990833));
#30864=CARTESIAN_POINT('Ctrl Pts',(95.1050171542381,4.50266047654211,-5.75475624552021));
#30865=CARTESIAN_POINT('Ctrl Pts',(95.0388466194241,2.19933752498479,-6.97534328817024));
#30866=CARTESIAN_POINT('Ctrl Pts',(94.9726760846101,-0.0930966390109256,
-6.94416713037601));
#30867=CARTESIAN_POINT('Ctrl Pts',(94.9065055497961,-2.38553080300677,-6.91299097258179));
#30868=CARTESIAN_POINT('Ctrl Pts',(94.840335014982,-4.66707617944086,-5.63005161434315));
#30869=CARTESIAN_POINT('Ctrl Pts',(94.7741644801679,-5.88672315268717,-3.68439347365119));
#30870=CARTESIAN_POINT('Ctrl Pts',(94.737073541314,-6.57037867149475,-2.59378286683231));
#30871=CARTESIAN_POINT('Ctrl Pts',(94.6999826024601,-6.92038557175193,-1.2949459310265));
#30872=CARTESIAN_POINT('Ctrl Pts',(94.6628916636061,-6.92404070110412,0.00207036192589771));
#30873=CARTESIAN_POINT('Ctrl Pts',(94.4835483363939,-6.92908201353558,0.00220150041010815));
#30874=CARTESIAN_POINT('Ctrl Pts',(94.4861847640141,-6.92920117420624,-0.0898400237292746));
#30875=CARTESIAN_POINT('Ctrl Pts',(94.4888211916344,-6.92752010633732,-0.18190021269113));
#30876=CARTESIAN_POINT('Ctrl Pts',(94.4914576192547,-6.92403046519316,-0.273907744256341));
#30877=CARTESIAN_POINT('Ctrl Pts',(94.5245428866617,-6.88023798269881,-1.42853598508922));
#30878=CARTESIAN_POINT('Ctrl Pts',(94.5576281540687,-6.55162338873298,-2.57487150640527));
#30879=CARTESIAN_POINT('Ctrl Pts',(94.5907134214757,-5.95885134174323,-3.5606920135467));
#30880=CARTESIAN_POINT('Ctrl Pts',(94.6568839562896,-4.7733072477636,-5.53233302782977));
#30881=CARTESIAN_POINT('Ctrl Pts',(94.7230544911038,-2.53113334168807,-6.86191398541422));
#30882=CARTESIAN_POINT('Ctrl Pts',(94.7892250259179,-0.239839551955025,
-6.94064846452462));
#30883=CARTESIAN_POINT('Ctrl Pts',(94.8553955607319,2.05145423777802,-7.01938294363501));
#30884=CARTESIAN_POINT('Ctrl Pts',(94.9215660955459,4.39186791116858,-5.84727094427134));
#30885=CARTESIAN_POINT('Ctrl Pts',(94.9877366303599,5.70336724912391,-3.96230573866875));
#30886=CARTESIAN_POINT('Ctrl Pts',(95.053907165174,7.01486658707917,-2.07734053306627));
#30887=CARTESIAN_POINT('Ctrl Pts',(95.120077699988,7.29745158959932,0.520477878775046));
#30888=CARTESIAN_POINT('Ctrl Pts',(95.186248234802,6.42191537663093,2.64334402612632));
#30889=CARTESIAN_POINT('Ctrl Pts',(95.2524187696161,5.5463791636625,4.76621017347772));
#30890=CARTESIAN_POINT('Ctrl Pts',(95.3185893044301,3.5127217352054,6.41412405633902));
#30891=CARTESIAN_POINT('Ctrl Pts',(95.3847598392442,1.2580890031021,6.82988551727358));
#30892=CARTESIAN_POINT('Ctrl Pts',(95.4509303740582,-0.996543729001065,
7.24564697820812));
#30893=CARTESIAN_POINT('Ctrl Pts',(95.5171009088724,-3.4721517647504,6.42925601721605));
#30894=CARTESIAN_POINT('Ctrl Pts',(95.5832714436863,-5.05389323211731,4.75863427116323));
#30895=CARTESIAN_POINT('Ctrl Pts',(95.6163567110933,-5.84476396580081,3.92332339813677));
#30896=CARTESIAN_POINT('Ctrl Pts',(95.6494419785002,-6.41216805738867,2.8744548288451));
#30897=CARTESIAN_POINT('Ctrl Pts',(95.6825272459073,-6.70319462303771,1.75624747144725));
#30898=CARTESIAN_POINT('Ctrl Pts',(95.6995342760694,-6.85279285717295,1.1814482406943));
#30899=CARTESIAN_POINT('Ctrl Pts',(95.7165413062316,-6.92936292591762,0.588327388208185));
#30900=CARTESIAN_POINT('Ctrl Pts',(95.7335483363938,-6.93097598691781,-0.00393591295944164));
#30901=CARTESIAN_POINT('Origin',(29.75,0.,0.));
#30902=CARTESIAN_POINT('',(97.1628916636062,-6.94438291503296,0.0033794907004818));
#30903=CARTESIAN_POINT('',(96.9835483363938,-6.94194141381233,0.000872210908587178));
#30904=CARTESIAN_POINT('',(29.75,-6.933,-8.4904762584886E-16));
#30905=CARTESIAN_POINT('Ctrl Pts',(97.1628916636062,-6.94438291503296,0.0033794907004818));
#30906=CARTESIAN_POINT('Ctrl Pts',(97.1606956868953,-6.94459561280772,0.0794883938480412));
#30907=CARTESIAN_POINT('Ctrl Pts',(97.1584997101843,-6.94345033553247,0.155584207710589));
#30908=CARTESIAN_POINT('Ctrl Pts',(97.1563037334734,-6.94092737286312,0.231627553260109));
#30909=CARTESIAN_POINT('Ctrl Pts',(97.0901331986593,-6.86490389396477,2.52301289399314));
#30910=CARTESIAN_POINT('Ctrl Pts',(97.0239626638451,-5.53797669587943,4.76675832492743));
#30911=CARTESIAN_POINT('Ctrl Pts',(96.9577921290311,-3.5677397385306,5.95463433692111));
#30912=CARTESIAN_POINT('Ctrl Pts',(96.9247068616242,-2.5826212598563,6.54857234291788));
#30913=CARTESIAN_POINT('Ctrl Pts',(96.8916215942172,-1.43667534136616,6.87854299417956));
#30914=CARTESIAN_POINT('Ctrl Pts',(96.8585363268102,-0.282099721775767,
6.92370154485739));
#30915=CARTESIAN_POINT('Ctrl Pts',(96.8254510594032,0.872475897814623,6.96886009553523));
#30916=CARTESIAN_POINT('Ctrl Pts',(96.7923657919961,2.03568121850526,6.72920654562922));
#30917=CARTESIAN_POINT('Ctrl Pts',(96.7592805245891,3.06654158312319,6.22106594698705));
#30918=CARTESIAN_POINT('Ctrl Pts',(96.726195257182,4.09740194774136,5.71292534834477));
#30919=CARTESIAN_POINT('Ctrl Pts',(96.6931099897751,4.99591735628674,4.9362977009662));
#30920=CARTESIAN_POINT('Ctrl Pts',(96.660024722368,5.66328080375355,3.99305320188991));
#30921=CARTESIAN_POINT('Ctrl Pts',(96.626939454961,6.33064425122035,3.04980870281361));
#30922=CARTESIAN_POINT('Ctrl Pts',(96.593854187554,6.76685573760857,1.93994735203959));
#30923=CARTESIAN_POINT('Ctrl Pts',(96.560768920147,6.89575386284522,0.796878655370808));
#30924=CARTESIAN_POINT('Ctrl Pts',(96.4945983853329,7.15355011331848,-1.4892587379665));
#30925=CARTESIAN_POINT('Ctrl Pts',(96.4284278505189,6.18209291918581,-3.90822551488283));
#30926=CARTESIAN_POINT('Ctrl Pts',(96.3622573157048,4.41100253414985,-5.36406382908644));
#30927=CARTESIAN_POINT('Ctrl Pts',(96.2960867808908,2.63991214911409,-6.81990214328987));
#30928=CARTESIAN_POINT('Ctrl Pts',(96.2299162460767,0.0691885731752734,
-7.31261199478086));
#30929=CARTESIAN_POINT('Ctrl Pts',(96.1637457112627,-2.1182055609885,-6.61373343479036));
#30930=CARTESIAN_POINT('Ctrl Pts',(96.0975751764487,-4.30559969515253,-5.91485487479979));
#30931=CARTESIAN_POINT('Ctrl Pts',(96.0314046416347,-6.10966438754142,-4.02438790332748));
#30932=CARTESIAN_POINT('Ctrl Pts',(95.9652341068207,-6.70552369555624,-1.80671434194794));
#30933=CARTESIAN_POINT('Ctrl Pts',(95.9477866257492,-6.86263658616644,-1.22197042845769));
#30934=CARTESIAN_POINT('Ctrl Pts',(95.9303391446777,-6.93574992881354,-0.614477729042277));
#30935=CARTESIAN_POINT('Ctrl Pts',(95.9128916636062,-6.93006097531607,-0.0057025460704313));
#30936=CARTESIAN_POINT('Ctrl Pts',(95.7335483363938,-6.93097598691781,-0.00393591295944164));
#30937=CARTESIAN_POINT('Ctrl Pts',(95.7496265736387,-6.93250095495774,-0.56385435708546));
#30938=CARTESIAN_POINT('Ctrl Pts',(95.7657048108836,-6.86703250395054,-1.12300635793202));
#30939=CARTESIAN_POINT('Ctrl Pts',(95.7817830481285,-6.73294086289519,-1.66518651644247));
#30940=CARTESIAN_POINT('Ctrl Pts',(95.8148683155355,-6.45701149739346,-2.78086700143006));
#30941=CARTESIAN_POINT('Ctrl Pts',(95.8479535829424,-5.89050372667986,-3.82468182590149));
#30942=CARTESIAN_POINT('Ctrl Pts',(95.8810388503494,-5.11180054835783,-4.67832432491541));
#30943=CARTESIAN_POINT('Ctrl Pts',(95.9141241177564,-4.33309737003554,-5.53196682392962));
#30944=CARTESIAN_POINT('Ctrl Pts',(95.9472093851635,-3.34219878410467,-6.19543699748618));
#30945=CARTESIAN_POINT('Ctrl Pts',(95.9802946525705,-2.25314033729704,-6.56580501909516));
#30946=CARTESIAN_POINT('Ctrl Pts',(96.0464651873846,-0.0750234436820296,
-7.30654106231305));
#30947=CARTESIAN_POINT('Ctrl Pts',(96.1126357221986,2.49573289343994,-6.8748684977409));
#30948=CARTESIAN_POINT('Ctrl Pts',(96.1788062570126,4.2966487576269,-5.4560914189897));
#30949=CARTESIAN_POINT('Ctrl Pts',(96.2449767918266,6.09756462181375,-4.03731434023859));
#30950=CARTESIAN_POINT('Ctrl Pts',(96.3111473266407,7.12864001306566,-1.63143274730855));
#30951=CARTESIAN_POINT('Ctrl Pts',(96.3773178614547,6.913716874689,0.654815792194409));
#30952=CARTESIAN_POINT('Ctrl Pts',(96.4434883962688,6.69879373631232,2.9410643316975));
#30953=CARTESIAN_POINT('Ctrl Pts',(96.5096589310827,5.23787206830692,5.10767981777348));
#30954=CARTESIAN_POINT('Ctrl Pts',(96.5758294658968,3.19893187329868,6.16401651644934));
#30955=CARTESIAN_POINT('Ctrl Pts',(96.6420000007108,1.15999167829055,7.22035321512515));
#30956=CARTESIAN_POINT('Ctrl Pts',(96.708170535525,-1.45696704372035,7.16641112640097));
#30957=CARTESIAN_POINT('Ctrl Pts',(96.774341070339,-3.44741502385695,6.0287190821994));
#30958=CARTESIAN_POINT('Ctrl Pts',(96.840511605153,-5.43786300399367,4.89102703799777));
#30959=CARTESIAN_POINT('Ctrl Pts',(96.9066821399668,-6.80180024225602,2.66958503831864));
#30960=CARTESIAN_POINT('Ctrl Pts',(96.972852674781,-6.93163671608136,0.372624965083196));
#30961=CARTESIAN_POINT('Ctrl Pts',(96.9764178953186,-6.93863221134688,0.248866418320443));
#30962=CARTESIAN_POINT('Ctrl Pts',(96.9799831158562,-6.94204514118107,0.124888644370122));
#30963=CARTESIAN_POINT('Ctrl Pts',(96.9835483363938,-6.94194141381233,0.000872210908587178));
#30964=CARTESIAN_POINT('Origin',(29.75,0.,0.));
#30965=CARTESIAN_POINT('',(98.4128916636062,-6.92920931711453,0.000661134518076692));
#30966=CARTESIAN_POINT('',(98.2335483363938,-6.92927911623139,0.00329186758170552));
#30967=CARTESIAN_POINT('',(29.75,-6.933,-8.4904762584886E-16));
#30968=CARTESIAN_POINT('Ctrl Pts',(98.4128916636061,-6.92277218803937,0.001783836750055));
#30969=CARTESIAN_POINT('Ctrl Pts',(98.3910522291127,-6.92795854075618,0.764408199582078));
#30970=CARTESIAN_POINT('Ctrl Pts',(98.3692127946193,-6.81209375619514,1.52619914819609));
#30971=CARTESIAN_POINT('Ctrl Pts',(98.3473733601259,-6.56846622737201,2.24537042560992));
#30972=CARTESIAN_POINT('Ctrl Pts',(98.314288092719,-6.19938698490055,3.33486631122398));
#30973=CARTESIAN_POINT('Ctrl Pts',(98.281202825312,-5.53708965775431,4.3265491885863));
#30974=CARTESIAN_POINT('Ctrl Pts',(98.248117557905,-4.68436907918055,5.10626180931842));
#30975=CARTESIAN_POINT('Ctrl Pts',(98.215032290498,-3.83164850060668,5.88597443005063));
#30976=CARTESIAN_POINT('Ctrl Pts',(98.1819470230908,-2.7885046706052,6.45371679415264));
#30977=CARTESIAN_POINT('Ctrl Pts',(98.1488617556838,-1.67315143243921,6.73096598430807));
#30978=CARTESIAN_POINT('Ctrl Pts',(98.1157764882768,-0.557798194273473,
7.00821517446343));
#30979=CARTESIAN_POINT('Ctrl Pts',(98.0826912208698,0.629764452056806,6.99497119067236));
#30980=CARTESIAN_POINT('Ctrl Pts',(98.0496059534628,1.7483153549858,6.70526783617236));
#30981=CARTESIAN_POINT('Ctrl Pts',(98.0165206860558,2.8668662579148,6.41556448167235));
#30982=CARTESIAN_POINT('Ctrl Pts',(97.9834354186488,3.91640541744259,5.8494017564634));
#30983=CARTESIAN_POINT('Ctrl Pts',(97.9503501512418,4.75265142482019,5.05951987470007));
#30984=CARTESIAN_POINT('Ctrl Pts',(97.8841796164277,6.42514343957568,3.47975611117313));
#30985=CARTESIAN_POINT('Ctrl Pts',(97.8180090816137,7.24446284573023,1.00511572142863));
#30986=CARTESIAN_POINT('Ctrl Pts',(97.7518385467997,6.83136924535634,-1.25000734093417));
#30987=CARTESIAN_POINT('Ctrl Pts',(97.6856680119856,6.41827564498251,-3.50513040329671));
#30988=CARTESIAN_POINT('Ctrl Pts',(97.6194974771716,4.7727690380803,-5.54073613827742));
#30989=CARTESIAN_POINT('Ctrl Pts',(97.5533269423575,2.65094026756886,-6.4187834083141));
#30990=CARTESIAN_POINT('Ctrl Pts',(97.4871564075435,0.529111497057312,-7.29683067835084));
#30991=CARTESIAN_POINT('Ctrl Pts',(97.4209858727295,-2.06903943706366,-7.01731948344348));
#30992=CARTESIAN_POINT('Ctrl Pts',(97.3548153379154,-3.95555502426836,-5.70805126072392));
#30993=CARTESIAN_POINT('Ctrl Pts',(97.2908407798123,-5.77946352652212,-4.44223323125975));
#30994=CARTESIAN_POINT('Ctrl Pts',(97.2268662217093,-6.93818647129019,-2.21387236916584));
#30995=CARTESIAN_POINT('Ctrl Pts',(97.1628916636062,-6.94438291503296,0.0033794907004818));
#30996=CARTESIAN_POINT('Ctrl Pts',(96.9835483363938,-6.94194141381233,0.000872210908587178));
#30997=CARTESIAN_POINT('Ctrl Pts',(97.0130683832633,-6.94108255059348,-1.02598458231818));
#30998=CARTESIAN_POINT('Ctrl Pts',(97.0425884301328,-6.69912695613847,-2.05549181351691));
#30999=CARTESIAN_POINT('Ctrl Pts',(97.0721084770023,-6.25348840864668,-2.98514757729132));
#31000=CARTESIAN_POINT('Ctrl Pts',(97.1051937444093,-5.75402881849591,-4.02708052804132));
#31001=CARTESIAN_POINT('Ctrl Pts',(97.1382790118161,-4.99871659239096,-4.94358687453451));
#31002=CARTESIAN_POINT('Ctrl Pts',(97.1713642792231,-4.06784541551554,-5.61764830451808));
#31003=CARTESIAN_POINT('Ctrl Pts',(97.2044495466301,-3.13697423864023,-6.29170973450157));
#31004=CARTESIAN_POINT('Ctrl Pts',(97.2375348140372,-2.03054411099448,-6.7233262479755));
#31005=CARTESIAN_POINT('Ctrl Pts',(97.2706200814443,-0.884785181006302,
-6.87272715293996));
#31006=CARTESIAN_POINT('Ctrl Pts',(97.3037053488513,0.260973748982006,-7.02212805790444));
#31007=CARTESIAN_POINT('Ctrl Pts',(97.3367906162583,1.44606148131276,-6.88931335435939));
#31008=CARTESIAN_POINT('Ctrl Pts',(97.3698758836653,2.51694132343833,-6.46926914749254));
#31009=CARTESIAN_POINT('Ctrl Pts',(97.4360464184792,4.65870100768948,-5.62918073375883));
#31010=CARTESIAN_POINT('Ctrl Pts',(97.5022169532934,6.34362913111992,-3.64017430673796));
#31011=CARTESIAN_POINT('Ctrl Pts',(97.5683874881074,6.80342467766202,-1.39410787752219));
#31012=CARTESIAN_POINT('Ctrl Pts',(97.6345580229215,7.26322022420409,0.851958551693452));
#31013=CARTESIAN_POINT('Ctrl Pts',(97.7007285577355,6.49788319385797,3.35508498310395));
#31014=CARTESIAN_POINT('Ctrl Pts',(97.7668990925495,4.85806604502377,4.96260607415636));
#31015=CARTESIAN_POINT('Ctrl Pts',(97.8330696273635,3.21824889618947,6.57012716520887));
#31016=CARTESIAN_POINT('Ctrl Pts',(97.8992401621775,0.703951628866997,7.28204291590319));
#31017=CARTESIAN_POINT('Ctrl Pts',(97.9654106969916,-1.53520881853428,6.77284272876324));
#31018=CARTESIAN_POINT('Ctrl Pts',(98.0315812318057,-3.77436926593531,6.26364254162335));
#31019=CARTESIAN_POINT('Ctrl Pts',(98.0977517666198,-5.73839289341521,4.53332641664947));
#31020=CARTESIAN_POINT('Ctrl Pts',(98.1639223014338,-6.52437983792119,2.37962010609202));
#31021=CARTESIAN_POINT('Ctrl Pts',(98.1871309797538,-6.80005719507182,1.62422834300578));
#31022=CARTESIAN_POINT('Ctrl Pts',(98.2103396580738,-6.93081387900884,0.81675162228316));
#31023=CARTESIAN_POINT('Ctrl Pts',(98.2335483363938,-6.92470486363958,0.00733871095478924));
#31024=CARTESIAN_POINT('Origin',(29.75,0.,0.));
#31025=CARTESIAN_POINT('',(99.6628916636061,-6.933,4.46781500684779E-12));
#31026=CARTESIAN_POINT('',(99.4835483363938,-6.92933028435402,-0.00338549438887613));
#31027=CARTESIAN_POINT('',(29.75,-6.933,-8.4904762584886E-16));
#31028=CARTESIAN_POINT('Ctrl Pts',(99.6628916636061,-6.933,5.25579579857549E-12));
#31029=CARTESIAN_POINT('Ctrl Pts',(99.605667468321,-6.93299999999849,1.99420935702147));
#31030=CARTESIAN_POINT('Ctrl Pts',(99.548443273036,-6.02307502628955,3.97063309653488));
#31031=CARTESIAN_POINT('Ctrl Pts',(99.4912190777509,-4.507984847536,5.26731066241453));
#31032=CARTESIAN_POINT('Ctrl Pts',(99.4339948824658,-2.99289466878246,6.56398822829418));
#31033=CARTESIAN_POINT('Ctrl Pts',(99.3767706871807,-0.899664345623711,
7.15779044292472));
#31034=CARTESIAN_POINT('Ctrl Pts',(99.3195464918956,1.07062371682325,6.84983604599231));
#31035=CARTESIAN_POINT('Ctrl Pts',(99.2623222966105,3.04091177927021,6.5418816490599));
#31036=CARTESIAN_POINT('Ctrl Pts',(99.2050981013254,4.85311303640243,5.33766370386068));
#31037=CARTESIAN_POINT('Ctrl Pts',(99.1478739060403,5.90026971494006,3.64050907030337));
#31038=CARTESIAN_POINT('Ctrl Pts',(99.0906497107552,6.94742639347769,1.94335443674606));
#31039=CARTESIAN_POINT('Ctrl Pts',(99.0334255154701,7.21086008527494,-0.216464293128621));
#31040=CARTESIAN_POINT('Ctrl Pts',(98.976201320185,6.60233935005946,-2.11556236179801));
#31041=CARTESIAN_POINT('Ctrl Pts',(98.9189771248999,5.99381861484398,-4.01466043046741));
#31042=CARTESIAN_POINT('Ctrl Pts',(98.8617529296148,4.52419779646946,-5.61916312790721));
#31043=CARTESIAN_POINT('Ctrl Pts',(98.8045287343297,2.68569473000012,-6.39167683923785));
#31044=CARTESIAN_POINT('Ctrl Pts',(98.7473045390446,0.847191663530777,-7.1641905505685));
#31045=CARTESIAN_POINT('Ctrl Pts',(98.6900803437595,-1.32739978994589,-7.09093574623707));
#31046=CARTESIAN_POINT('Ctrl Pts',(98.6328561484744,-3.10974706736552,-6.19644754492536));
#31047=CARTESIAN_POINT('Ctrl Pts',(98.5756319531893,-4.89209434478515,-5.30195934361366));
#31048=CARTESIAN_POINT('Ctrl Pts',(98.5184077579043,-6.25040525058856,-3.60219296582318));
#31049=CARTESIAN_POINT('Ctrl Pts',(98.4611835626192,-6.72974280712855,-1.66644854403055));
#31050=CARTESIAN_POINT('Ctrl Pts',(98.4450862629482,-6.86458158035639,-1.12191912096339));
#31051=CARTESIAN_POINT('Ctrl Pts',(98.4289889632772,-6.93300000000035,-0.560975745773916));
#31052=CARTESIAN_POINT('Ctrl Pts',(98.4128916636062,-6.933,4.31821245427955E-12));
#31053=CARTESIAN_POINT('Ctrl Pts',(98.2335483363938,-6.933,-7.69384556065233E-13));
#31054=CARTESIAN_POINT('Ctrl Pts',(98.2907725316789,-6.93299999999978,-1.99420935701711));
#31055=CARTESIAN_POINT('Ctrl Pts',(98.347996726964,-6.02307502629199,-3.97063309653124));
#31056=CARTESIAN_POINT('Ctrl Pts',(98.4052209222491,-4.50798484753911,-5.26731066241187));
#31057=CARTESIAN_POINT('Ctrl Pts',(98.4624451175342,-2.99289466878623,-6.5639882282925));
#31058=CARTESIAN_POINT('Ctrl Pts',(98.5196693128193,-0.89966434562766,-7.15779044292426));
#31059=CARTESIAN_POINT('Ctrl Pts',(98.5768935081044,1.0706237168196,-6.84983604599288));
#31060=CARTESIAN_POINT('Ctrl Pts',(98.6341177033895,3.04091177926685,-6.5418816490615));
#31061=CARTESIAN_POINT('Ctrl Pts',(98.6913418986746,4.85311303639982,-5.33766370386311));
#31062=CARTESIAN_POINT('Ctrl Pts',(98.7485660939597,5.90026971493833,-3.64050907030619));
#31063=CARTESIAN_POINT('Ctrl Pts',(98.8057902892448,6.94742639347683,-1.94335443674926));
#31064=CARTESIAN_POINT('Ctrl Pts',(98.8630144845299,7.21086008527507,0.216464293125468));
#31065=CARTESIAN_POINT('Ctrl Pts',(98.920238679815,6.60233935006035,2.11556236179524));
#31066=CARTESIAN_POINT('Ctrl Pts',(98.9774628751001,5.99381861484563,4.01466043046502));
#31067=CARTESIAN_POINT('Ctrl Pts',(99.0346870703851,4.52419779647162,5.61916312790552));
#31068=CARTESIAN_POINT('Ctrl Pts',(99.0919112656702,2.68569473000244,6.39167683923688));
#31069=CARTESIAN_POINT('Ctrl Pts',(99.1491354609553,0.847191663533256,7.16419055056824));
#31070=CARTESIAN_POINT('Ctrl Pts',(99.2063596562404,-1.32739978994361,7.09093574623753));
#31071=CARTESIAN_POINT('Ctrl Pts',(99.2635838515255,-3.10974706736363,6.19644754492631));
#31072=CARTESIAN_POINT('Ctrl Pts',(99.3208080468106,-4.89209434478364,5.30195934361509));
#31073=CARTESIAN_POINT('Ctrl Pts',(99.3780322420957,-6.25040525058763,3.60219296582487));
#31074=CARTESIAN_POINT('Ctrl Pts',(99.4352564373808,-6.72974280712813,1.66644854403223));
#31075=CARTESIAN_POINT('Ctrl Pts',(99.4513537370518,-6.86458158035598,1.12191912096561));
#31076=CARTESIAN_POINT('Ctrl Pts',(99.4674510367228,-6.93300000000008,0.560975745776695));
#31077=CARTESIAN_POINT('Ctrl Pts',(99.4835483363938,-6.933,-1.01391117723892E-12));
#31078=CARTESIAN_POINT('Origin',(29.75,0.,0.));
#31079=CARTESIAN_POINT('',(100.912891663606,-6.933,5.40539835114373E-12));
#31080=CARTESIAN_POINT('',(100.733548336394,-6.94397743835492,-0.00162794009456958));
#31081=CARTESIAN_POINT('',(29.75,-6.933,-8.4904762584886E-16));
#31082=CARTESIAN_POINT('Ctrl Pts',(100.912891663606,-6.93501187936537,-0.00181345658265553));
#31083=CARTESIAN_POINT('Ctrl Pts',(100.884850580955,-6.93263583601006,0.972625129661142));
#31084=CARTESIAN_POINT('Ctrl Pts',(100.856809498304,-6.71995816851569,1.94841025277312));
#31085=CARTESIAN_POINT('Ctrl Pts',(100.828768415652,-6.31974308779576,2.84219468712902));
#31086=CARTESIAN_POINT('Ctrl Pts',(100.795683148245,-5.84753510885921,3.89675799991803));
#31087=CARTESIAN_POINT('Ctrl Pts',(100.762597880838,-5.11425070045544,4.83716570681445));
#31088=CARTESIAN_POINT('Ctrl Pts',(100.729512613431,-4.1959559550899,5.52995393753654));
#31089=CARTESIAN_POINT('Ctrl Pts',(100.663342078617,-2.35936646435863,6.91553039898088));
#31090=CARTESIAN_POINT('Ctrl Pts',(100.597171543803,0.217264374219888,7.31062895572762));
#31091=CARTESIAN_POINT('Ctrl Pts',(100.531001008989,2.37189911809706,6.52719071977832));
#31092=CARTESIAN_POINT('Ctrl Pts',(100.464830474175,4.52653386197423,5.74375248382901));
#31093=CARTESIAN_POINT('Ctrl Pts',(100.398659939361,6.25917251115006,3.78177745518367));
#31094=CARTESIAN_POINT('Ctrl Pts',(100.332489404547,6.77102160540967,1.54322103541326));
#31095=CARTESIAN_POINT('Ctrl Pts',(100.266318869733,7.28287069966925,-0.695335384357018));
#31096=CARTESIAN_POINT('Ctrl Pts',(100.200148334919,6.57393023901274,-3.21047319525232));
#31097=CARTESIAN_POINT('Ctrl Pts',(100.133977800105,4.96835042337348,-4.85219113552126));
#31098=CARTESIAN_POINT('Ctrl Pts',(100.067807265291,3.36277060773414,-6.49390907579028));
#31099=CARTESIAN_POINT('Ctrl Pts',(100.001636730477,0.860551437111937,-7.26220714543285));
#31100=CARTESIAN_POINT('Ctrl Pts',(99.9354661956629,-1.38605742730384,-6.80506935504743));
#31101=CARTESIAN_POINT('Ctrl Pts',(99.8692956608489,-3.63266629171949,-6.34793156466204));
#31102=CARTESIAN_POINT('Ctrl Pts',(99.8031251260347,-5.62366484992875,-4.66535791424881));
#31103=CARTESIAN_POINT('Ctrl Pts',(99.7369545912207,-6.46628669943668,-2.52459367998469));
#31104=CARTESIAN_POINT('Ctrl Pts',(99.7122669486825,-6.78066147476532,-1.72589343791122));
#31105=CARTESIAN_POINT('Ctrl Pts',(99.6875793061444,-6.93518562941577,-0.863414429982868));
#31106=CARTESIAN_POINT('Ctrl Pts',(99.6628916636062,-6.93186678979006,-0.000948267261432489));
#31107=CARTESIAN_POINT('Ctrl Pts',(99.4835483363938,-6.92482311535644,-0.00754358095680571));
#31108=CARTESIAN_POINT('Ctrl Pts',(99.5068667351054,-6.93021552428664,-0.822381842477515));
#31109=CARTESIAN_POINT('Ctrl Pts',(99.5301851338169,-6.79757852095591,-1.63512275943323));
#31110=CARTESIAN_POINT('Ctrl Pts',(99.5535035325285,-6.51926479436836,-2.39359784836531));
#31111=CARTESIAN_POINT('Ctrl Pts',(99.6196740673425,-5.72949494944151,-4.54591983661744));
#31112=CARTESIAN_POINT('Ctrl Pts',(99.6858446021565,-3.76666029668156,-6.26126512949026));
#31113=CARTESIAN_POINT('Ctrl Pts',(99.7520151369706,-1.52353023483686,-6.7723919372603));
#31114=CARTESIAN_POINT('Ctrl Pts',(99.7851004043776,-0.401965203914322,
-7.02795534114536));
#31115=CARTESIAN_POINT('Ctrl Pts',(99.8181856717847,0.789673679279438,-6.98246412375461));
#31116=CARTESIAN_POINT('Ctrl Pts',(99.8512709391917,1.90031642472727,-6.66378427180821));
#31117=CARTESIAN_POINT('Ctrl Pts',(99.8843562065988,3.01095917017484,-6.34510441986188));
#31118=CARTESIAN_POINT('Ctrl Pts',(99.9174414740057,4.04060577787652,-5.75323593336004));
#31119=CARTESIAN_POINT('Ctrl Pts',(99.9505267414127,4.86048491773434,-4.94783034897748));
#31120=CARTESIAN_POINT('Ctrl Pts',(99.9836120088197,5.68036405759236,-4.14242476459473));
#31121=CARTESIAN_POINT('Ctrl Pts',(100.016697276227,6.29047572960643,-3.12348208233117));
#31122=CARTESIAN_POINT('Ctrl Pts',(100.049782543634,6.6288845593698,-2.01869087129143));
#31123=CARTESIAN_POINT('Ctrl Pts',(100.082867811041,6.9672933891331,-0.913899660251946));
#31124=CARTESIAN_POINT('Ctrl Pts',(100.115953078448,7.03399937664582,0.276740079563676));
#31125=CARTESIAN_POINT('Ctrl Pts',(100.149038345855,6.79845053797514,1.40267858436484));
#31126=CARTESIAN_POINT('Ctrl Pts',(100.215208880669,6.32735286063373,3.65455559396744));
#31127=CARTESIAN_POINT('Ctrl Pts',(100.281379415483,4.64723587855842,5.64762766351217));
#31128=CARTESIAN_POINT('Ctrl Pts',(100.347549950297,2.5093203053586,6.4756031166143));
#31129=CARTESIAN_POINT('Ctrl Pts',(100.413720485111,0.371404732158899,7.30357856971639));
#31130=CARTESIAN_POINT('Ctrl Pts',(100.479891019925,-2.22430943216523,6.96645740637609));
#31131=CARTESIAN_POINT('Ctrl Pts',(100.546061554739,-4.08281761268181,5.61772775120349));
#31132=CARTESIAN_POINT('Ctrl Pts',(100.608557148624,-5.83810903971579,4.34390306432321));
#31133=CARTESIAN_POINT('Ctrl Pts',(100.671052742509,-6.93580568086616,2.16771393087575));
#31134=CARTESIAN_POINT('Ctrl Pts',(100.733548336394,-6.94397743835492,-0.00162794009456958));
#31135=CARTESIAN_POINT('Origin',(29.75,0.,0.));
#31136=CARTESIAN_POINT('',(102.162891663606,-6.933,4.76702011198427E-12));
#31137=CARTESIAN_POINT('',(101.983548336394,-6.93371908702931,0.00569271503419462));
#31138=CARTESIAN_POINT('',(29.75,-6.933,-8.4904762584886E-16));
#31139=CARTESIAN_POINT('Ctrl Pts',(102.162891663606,-6.933,4.76702011198427E-12));
#31140=CARTESIAN_POINT('Ctrl Pts',(102.105667468321,-6.93299999999863,1.99420935702098));
#31141=CARTESIAN_POINT('Ctrl Pts',(102.048443273036,-6.02307502628983,3.97063309653446));
#31142=CARTESIAN_POINT('Ctrl Pts',(101.991219077751,-4.50798484753637,5.26731066241421));
#31143=CARTESIAN_POINT('Ctrl Pts',(101.933994882466,-2.99289466878292,6.56398822829397));
#31144=CARTESIAN_POINT('Ctrl Pts',(101.876770687181,-0.899664345624216,
7.15779044292466));
#31145=CARTESIAN_POINT('Ctrl Pts',(101.819546491896,1.07062371682277,6.84983604599239));
#31146=CARTESIAN_POINT('Ctrl Pts',(101.76232229661,3.04091177926975,6.54188164906011));
#31147=CARTESIAN_POINT('Ctrl Pts',(101.705098101325,4.85311303640206,5.33766370386103));
#31148=CARTESIAN_POINT('Ctrl Pts',(101.64787390604,5.9002697149398,3.64050907030379));
#31149=CARTESIAN_POINT('Ctrl Pts',(101.590649710755,6.94742639347755,1.94335443674655));
#31150=CARTESIAN_POINT('Ctrl Pts',(101.53342551547,7.21086008527496,-0.216464293128111));
#31151=CARTESIAN_POINT('Ctrl Pts',(101.476201320185,6.60233935005961,-2.11556236179755));
#31152=CARTESIAN_POINT('Ctrl Pts',(101.4189771249,5.99381861484427,-4.01466043046699));
#31153=CARTESIAN_POINT('Ctrl Pts',(101.361752929615,4.52419779646985,-5.61916312790689));
#31154=CARTESIAN_POINT('Ctrl Pts',(101.30452873433,2.68569473000057,-6.39167683923766));
#31155=CARTESIAN_POINT('Ctrl Pts',(101.247304539045,0.847191663531283,-7.16419055056844));
#31156=CARTESIAN_POINT('Ctrl Pts',(101.19008034376,-1.32739978994539,-7.09093574623716));
#31157=CARTESIAN_POINT('Ctrl Pts',(101.132856148474,-3.10974706736508,-6.19644754492558));
#31158=CARTESIAN_POINT('Ctrl Pts',(101.075631953189,-4.89209434478478,-5.301959343614));
#31159=CARTESIAN_POINT('Ctrl Pts',(101.018407757904,-6.2504052505883,-3.60219296582362));
#31160=CARTESIAN_POINT('Ctrl Pts',(100.961183562619,-6.72974280712843,-1.66644854403103));
#31161=CARTESIAN_POINT('Ctrl Pts',(100.945086262948,-6.86458158035643,-1.12191912096336));
#31162=CARTESIAN_POINT('Ctrl Pts',(100.928988963277,-6.93300000000044,-0.560975745773355));
#31163=CARTESIAN_POINT('Ctrl Pts',(100.912891663606,-6.933,5.40539835114373E-12));
#31164=CARTESIAN_POINT('Ctrl Pts',(100.733548336394,-6.94397743835492,-0.00162794009456958));
#31165=CARTESIAN_POINT('Ctrl Pts',(100.737223277323,-6.94445796384787,-0.129192184793122));
#31166=CARTESIAN_POINT('Ctrl Pts',(100.740898218252,-6.94117111235913,-0.256732752915367));
#31167=CARTESIAN_POINT('Ctrl Pts',(100.744573159181,-6.93402905925297,-0.384064773836234));
#31168=CARTESIAN_POINT('Ctrl Pts',(100.810743693995,-6.8054301285985,-2.6767894966986));
#31169=CARTESIAN_POINT('Ctrl Pts',(100.876914228809,-5.42693007058041,-4.9019007954182));
#31170=CARTESIAN_POINT('Ctrl Pts',(100.943084763623,-3.4344862106255,-6.03609381867223));
#31171=CARTESIAN_POINT('Ctrl Pts',(101.009255298437,-1.44204235067071,-7.1702868419262));
#31172=CARTESIAN_POINT('Ctrl Pts',(101.075425833251,1.16434531122071,-7.21356158971465));
#31173=CARTESIAN_POINT('Ctrl Pts',(101.141596368065,3.20756104559799,-6.15613426324448));
#31174=CARTESIAN_POINT('Ctrl Pts',(101.174681635472,4.22916891278669,-5.62742060000936));
#31175=CARTESIAN_POINT('Ctrl Pts',(101.207766902879,5.10998379809678,-4.82353141820959));
#31176=CARTESIAN_POINT('Ctrl Pts',(101.240852170286,5.75260410317904,-3.86325890504045));
#31177=CARTESIAN_POINT('Ctrl Pts',(101.273937437693,6.39522440826123,-2.90298639187141));
#31178=CARTESIAN_POINT('Ctrl Pts',(101.3070227051,6.79965013311558,-1.78633054733313));
#31179=CARTESIAN_POINT('Ctrl Pts',(101.340107972508,6.90602743040454,-0.641968790741197));
#31180=CARTESIAN_POINT('Ctrl Pts',(101.373193239915,7.01240472769351,0.502392965850864));
#31181=CARTESIAN_POINT('Ctrl Pts',(101.406278507322,6.82073359741688,1.67446063449685));
#31182=CARTESIAN_POINT('Ctrl Pts',(101.439363774729,6.36612416211952,2.73672915864262));
#31183=CARTESIAN_POINT('Ctrl Pts',(101.472449042136,5.9115147268222,3.79899768278826));
#31184=CARTESIAN_POINT('Ctrl Pts',(101.505534309543,5.19396698650421,4.75146706243399));
#31185=CARTESIAN_POINT('Ctrl Pts',(101.53861957695,4.2873175361163,5.45942719274101));
#31186=CARTESIAN_POINT('Ctrl Pts',(101.604790111764,2.47401863534027,6.8753474533552));
#31187=CARTESIAN_POINT('Ctrl Pts',(101.670960646578,-0.0956871057154265,
7.31323071661412));
#31188=CARTESIAN_POINT('Ctrl Pts',(101.737131181392,-2.2630495505609,6.56572393955883));
#31189=CARTESIAN_POINT('Ctrl Pts',(101.803301716206,-4.43041199540625,5.81821716250359));
#31190=CARTESIAN_POINT('Ctrl Pts',(101.86947225102,-6.19543114404131,3.88532034513432));
#31191=CARTESIAN_POINT('Ctrl Pts',(101.935642785834,-6.7444279485813,1.6555833991261));
#31192=CARTESIAN_POINT('Ctrl Pts',(101.951611302687,-6.87691387680221,1.1174950777781));
#31193=CARTESIAN_POINT('Ctrl Pts',(101.967579819541,-6.9385821686616,0.562119642924724));
#31194=CARTESIAN_POINT('Ctrl Pts',(101.983548336394,-6.93371908702931,0.00569271503419462));
#31195=CARTESIAN_POINT('Origin',(29.75,0.,0.));
#31196=CARTESIAN_POINT('',(103.412891663606,-6.933,4.91634510879635E-12));
#31197=CARTESIAN_POINT('',(103.233548336394,-6.92083937541073,0.000353000077293465));
#31198=CARTESIAN_POINT('',(29.75,-6.933,-8.4904762584886E-16));
#31199=CARTESIAN_POINT('Ctrl Pts',(103.412891663606,-6.933,4.91634510879635E-12));
#31200=CARTESIAN_POINT('Ctrl Pts',(103.355667468321,-6.93299999999859,1.99420935702113));
#31201=CARTESIAN_POINT('Ctrl Pts',(103.298443273036,-6.02307502628974,3.97063309653459));
#31202=CARTESIAN_POINT('Ctrl Pts',(103.241219077751,-4.50798484753626,5.26731066241431));
#31203=CARTESIAN_POINT('Ctrl Pts',(103.183994882466,-2.99289466878278,6.56398822829403));
#31204=CARTESIAN_POINT('Ctrl Pts',(103.126770687181,-0.899664345624063,
7.15779044292468));
#31205=CARTESIAN_POINT('Ctrl Pts',(103.069546491896,1.07062371682291,6.84983604599236));
#31206=CARTESIAN_POINT('Ctrl Pts',(103.01232229661,3.04091177926989,6.54188164906005));
#31207=CARTESIAN_POINT('Ctrl Pts',(102.955098101325,4.85311303640217,5.33766370386092));
#31208=CARTESIAN_POINT('Ctrl Pts',(102.89787390604,5.90026971493988,3.64050907030366));
#31209=CARTESIAN_POINT('Ctrl Pts',(102.840649710755,6.94742639347759,1.9433544367464));
#31210=CARTESIAN_POINT('Ctrl Pts',(102.78342551547,7.21086008527495,-0.216464293128266));
#31211=CARTESIAN_POINT('Ctrl Pts',(102.726201320185,6.60233935005957,-2.11556236179769));
#31212=CARTESIAN_POINT('Ctrl Pts',(102.6689771249,5.99381861484418,-4.01466043046711));
#31213=CARTESIAN_POINT('Ctrl Pts',(102.611752929615,4.52419779646973,-5.61916312790699));
#31214=CARTESIAN_POINT('Ctrl Pts',(102.55452873433,2.68569473000043,-6.39167683923772));
#31215=CARTESIAN_POINT('Ctrl Pts',(102.497304539045,0.847191663531128,-7.16419055056846));
#31216=CARTESIAN_POINT('Ctrl Pts',(102.44008034376,-1.32739978994555,-7.09093574623713));
#31217=CARTESIAN_POINT('Ctrl Pts',(102.382856148474,-3.10974706736522,-6.19644754492551));
#31218=CARTESIAN_POINT('Ctrl Pts',(102.325631953189,-4.89209434478489,-5.3019593436139));
#31219=CARTESIAN_POINT('Ctrl Pts',(102.268407757904,-6.25040525058838,-3.60219296582349));
#31220=CARTESIAN_POINT('Ctrl Pts',(102.211183562619,-6.72974280712847,-1.66644854403088));
#31221=CARTESIAN_POINT('Ctrl Pts',(102.195086262948,-6.8645815803564,-1.12191912096347));
#31222=CARTESIAN_POINT('Ctrl Pts',(102.178988963277,-6.93300000000039,-0.560975745773731));
#31223=CARTESIAN_POINT('Ctrl Pts',(102.162891663606,-6.933,4.76702011198427E-12));
#31224=CARTESIAN_POINT('Ctrl Pts',(101.983548336394,-6.93371908702931,0.00569271503419462));
#31225=CARTESIAN_POINT('Ctrl Pts',(102.033750354355,-6.91843047170635,-1.74360904444629));
#31226=CARTESIAN_POINT('Ctrl Pts',(102.083952372315,-6.24557536097976,-3.5033032932907));
#31227=CARTESIAN_POINT('Ctrl Pts',(102.134154390276,-5.0483366904737,-4.7689161666655));
#31228=CARTESIAN_POINT('Ctrl Pts',(102.20032492509,-3.47027416738121,-6.4371017118016));
#31229=CARTESIAN_POINT('Ctrl Pts',(102.266495459904,-0.981174660751704,
-7.24689572742639));
#31230=CARTESIAN_POINT('Ctrl Pts',(102.332665994718,1.27272408831404,-6.82717346445915));
#31231=CARTESIAN_POINT('Ctrl Pts',(102.398836529532,3.52662283737954,-6.40745120149195));
#31232=CARTESIAN_POINT('Ctrl Pts',(102.465007064346,5.54532082888111,-4.75821265993281));
#31233=CARTESIAN_POINT('Ctrl Pts',(102.53117759916,6.42341876570948,-2.63175384271813));
#31234=CARTESIAN_POINT('Ctrl Pts',(102.564262866567,6.86246773412369,-1.56852443411073));
#31235=CARTESIAN_POINT('Ctrl Pts',(102.597348133974,7.01636668886959,-0.385989956589359));
#31236=CARTESIAN_POINT('Ctrl Pts',(102.630433401381,6.8873943833032,0.762247954493993));
#31237=CARTESIAN_POINT('Ctrl Pts',(102.663518668788,6.75842207773681,1.91048586557734));
#31238=CARTESIAN_POINT('Ctrl Pts',(102.696603936195,6.34657851185811,3.02442721022279));
#31239=CARTESIAN_POINT('Ctrl Pts',(102.729689203602,5.68920193750754,3.96715516611671));
#31240=CARTESIAN_POINT('Ctrl Pts',(102.762774471009,5.03182536315704,4.90988312201052));
#31241=CARTESIAN_POINT('Ctrl Pts',(102.795859738416,4.12891578033466,5.68139768915293));
#31242=CARTESIAN_POINT('Ctrl Pts',(102.828945005823,3.09604298671421,6.19933392871387));
#31243=CARTESIAN_POINT('Ctrl Pts',(102.86203027323,2.06317019309352,6.71727016827494));
#31244=CARTESIAN_POINT('Ctrl Pts',(102.895115540637,0.900334188675,6.98162808025441));
#31245=CARTESIAN_POINT('Ctrl Pts',(102.928200808044,-0.249119839419829,
6.93717350467326));
#31246=CARTESIAN_POINT('Ctrl Pts',(102.994371342858,-2.54802789560923,6.84826435351098));
#31247=CARTESIAN_POINT('Ctrl Pts',(103.060541877673,-4.79340804650275,5.52410525210601));
#31248=CARTESIAN_POINT('Ctrl Pts',(103.126712412487,-5.96636769431135,3.55423418686299));
#31249=CARTESIAN_POINT('Ctrl Pts',(103.162324387122,-6.59763672279808,2.49407956353618));
#31250=CARTESIAN_POINT('Ctrl Pts',(103.197936361758,-6.91828681390554,1.24689908283008));
#31251=CARTESIAN_POINT('Ctrl Pts',(103.233548336394,-6.92083937541073,0.000353000077293465));
#31252=CARTESIAN_POINT('Origin',(29.75,0.,0.));
#31253=CARTESIAN_POINT('',(104.662891663606,-6.93409162044397,-0.00297428074398909));
#31254=CARTESIAN_POINT('',(104.483548336394,-6.93479064018689,-0.00208547980832093));
#31255=CARTESIAN_POINT('',(29.75,-6.933,-8.4904762584886E-16));
#31256=CARTESIAN_POINT('Ctrl Pts',(104.662891663606,-6.933,5.06567010560843E-12));
#31257=CARTESIAN_POINT('Ctrl Pts',(104.605667468321,-6.93299999999854,1.99420935702154));
#31258=CARTESIAN_POINT('Ctrl Pts',(104.548443273036,-6.0230750262894,3.97063309653523));
#31259=CARTESIAN_POINT('Ctrl Pts',(104.491219077751,-4.50798484753555,5.26731066241492));
#31260=CARTESIAN_POINT('Ctrl Pts',(104.433994882466,-2.99289466878169,6.56398822829461));
#31261=CARTESIAN_POINT('Ctrl Pts',(104.376770687181,-0.89966434562254,7.15779044292494));
#31262=CARTESIAN_POINT('Ctrl Pts',(104.319546491896,1.07062371682462,6.8498360459921));
#31263=CARTESIAN_POINT('Ctrl Pts',(104.26232229661,3.04091177927178,6.54188164905925));
#31264=CARTESIAN_POINT('Ctrl Pts',(104.205098101325,4.85311303640397,5.33766370385939));
#31265=CARTESIAN_POINT('Ctrl Pts',(104.14787390604,5.9002697149412,3.64050907030152));
#31266=CARTESIAN_POINT('Ctrl Pts',(104.090649710755,6.94742639347844,1.94335443674366));
#31267=CARTESIAN_POINT('Ctrl Pts',(104.03342551547,7.21086008527493,-0.216464293131451));
#31268=CARTESIAN_POINT('Ctrl Pts',(103.976201320185,6.60233935005856,-2.11556236180084));
#31269=CARTESIAN_POINT('Ctrl Pts',(103.9189771249,5.99381861484219,-4.01466043047022));
#31270=CARTESIAN_POINT('Ctrl Pts',(103.861752929615,4.52419779646666,-5.61916312790956));
#31271=CARTESIAN_POINT('Ctrl Pts',(103.80452873433,2.68569472999666,-6.39167683923931));
#31272=CARTESIAN_POINT('Ctrl Pts',(103.747304539045,0.847191663526659,-7.16419055056906));
#31273=CARTESIAN_POINT('Ctrl Pts',(103.690080343759,-1.3273997899503,-7.09093574623631));
#31274=CARTESIAN_POINT('Ctrl Pts',(103.632856148474,-3.10974706736958,-6.19644754492333));
#31275=CARTESIAN_POINT('Ctrl Pts',(103.575631953189,-4.89209434478886,-5.30195934361034));
#31276=CARTESIAN_POINT('Ctrl Pts',(103.518407757904,-6.25040525059126,-3.60219296581864));
#31277=CARTESIAN_POINT('Ctrl Pts',(103.461183562619,-6.72974280712983,-1.66644854402538));
#31278=CARTESIAN_POINT('Ctrl Pts',(103.445086262948,-6.86458158035687,-1.12191912095965));
#31279=CARTESIAN_POINT('Ctrl Pts',(103.428988963277,-6.9330000000004,-0.560975745771742));
#31280=CARTESIAN_POINT('Ctrl Pts',(103.412891663606,-6.933,4.91634510879635E-12));
#31281=CARTESIAN_POINT('Ctrl Pts',(103.233548336394,-6.92083937541073,0.000353000077293465));
#31282=CARTESIAN_POINT('Ctrl Pts',(103.264106896572,-6.92302972304416,-1.06930555928247));
#31283=CARTESIAN_POINT('Ctrl Pts',(103.29466545675,-6.69099468583458,-2.13849699113908));
#31284=CARTESIAN_POINT('Ctrl Pts',(103.325224016929,-6.22000895328616,-3.08864911670163));
#31285=CARTESIAN_POINT('Ctrl Pts',(103.391394551743,-5.20015141972855,-5.14607832594236));
#31286=CARTESIAN_POINT('Ctrl Pts',(103.457565086557,-3.05989720788957,-6.64535371534269));
#31287=CARTESIAN_POINT('Ctrl Pts',(103.523735621371,-0.777838836008096,
-6.9009587370364));
#31288=CARTESIAN_POINT('Ctrl Pts',(103.589906156185,1.50421953587338,-7.15656375873012));
#31289=CARTESIAN_POINT('Ctrl Pts',(103.656076690999,3.92808206779747,-6.16849841271689));
#31290=CARTESIAN_POINT('Ctrl Pts',(103.722247225813,5.37870678028656,-4.39313526885716));
#31291=CARTESIAN_POINT('Ctrl Pts',(103.788417760627,6.82933149277582,-2.61777212499723));
#31292=CARTESIAN_POINT('Ctrl Pts',(103.854588295441,7.30671838583013,-0.0551111832906592));
#31293=CARTESIAN_POINT('Ctrl Pts',(103.920758830255,6.60489006341062,2.13585209660723));
#31294=CARTESIAN_POINT('Ctrl Pts',(103.953844097662,6.25397590220092,3.23133373655599));
#31295=CARTESIAN_POINT('Ctrl Pts',(103.986929365069,5.60825793712291,4.23389096105253));
#31296=CARTESIAN_POINT('Ctrl Pts',(104.020014632476,4.76861880313492,5.0276732238417));
#31297=CARTESIAN_POINT('Ctrl Pts',(104.053099899883,3.92897966914701,5.82145548663078));
#31298=CARTESIAN_POINT('Ctrl Pts',(104.08618516729,2.89541936624924,6.40646278771246));
#31299=CARTESIAN_POINT('Ctrl Pts',(104.119270434697,1.78482986806082,6.70221762849317));
#31300=CARTESIAN_POINT('Ctrl Pts',(104.152355702104,0.674240369872153,6.99797246927394));
#31301=CARTESIAN_POINT('Ctrl Pts',(104.185440969511,-0.513378323607498,
7.00447484975354));
#31302=CARTESIAN_POINT('Ctrl Pts',(104.218526236918,-1.63659125345655,6.73340867650101));
#31303=CARTESIAN_POINT('Ctrl Pts',(104.251611504325,-2.75980418330561,6.46234250324848));
#31304=CARTESIAN_POINT('Ctrl Pts',(104.284696771732,-3.81861134952433,5.91370777626388));
#31305=CARTESIAN_POINT('Ctrl Pts',(104.317782039139,-4.66787442237867,5.13783858297635));
#31306=CARTESIAN_POINT('Ctrl Pts',(104.373037471557,-6.08622168099608,3.84206583773441));
#31307=CARTESIAN_POINT('Ctrl Pts',(104.428292903976,-6.92010719630414,1.91248924632851));
#31308=CARTESIAN_POINT('Ctrl Pts',(104.483548336394,-6.93794935432642,-0.0057642951309926));
#31309=CARTESIAN_POINT('Origin',(29.75,0.,0.));
#31310=CARTESIAN_POINT('',(105.912891663606,-6.94073003849348,0.00450623896247018));
#31311=CARTESIAN_POINT('',(105.733548336394,-6.93358984723115,0.000731892616234763));
#31312=CARTESIAN_POINT('',(29.75,-6.933,-8.4904762584886E-16));
#31313=CARTESIAN_POINT('Ctrl Pts',(105.912891663606,-6.94073003849348,0.00450623896247018));
#31314=CARTESIAN_POINT('Ctrl Pts',(105.905532552046,-6.94274293080495,0.260275666085527));
#31315=CARTESIAN_POINT('Ctrl Pts',(105.898173440486,-6.9300008501143,0.515842442486986));
#31316=CARTESIAN_POINT('Ctrl Pts',(105.890814328926,-6.90187421034804,0.769673494383096));
#31317=CARTESIAN_POINT('Ctrl Pts',(105.824643794112,-6.64896938879624,3.05203276010309));
#31318=CARTESIAN_POINT('Ctrl Pts',(105.758473259298,-5.15222728481638,5.19405918682688));
#31319=CARTESIAN_POINT('Ctrl Pts',(105.692302724484,-3.09600615901486,6.21635022080577));
#31320=CARTESIAN_POINT('Ctrl Pts',(105.62613218967,-1.03978503321322,7.23864125478473));
#31321=CARTESIAN_POINT('Ctrl Pts',(105.559961654856,1.57591511441003,7.14119689601862));
#31322=CARTESIAN_POINT('Ctrl Pts',(105.493791120042,3.54717258793725,5.97056873725912));
#31323=CARTESIAN_POINT('Ctrl Pts',(105.427620585228,5.51843006146448,4.79994057849962));
#31324=CARTESIAN_POINT('Ctrl Pts',(105.361450050414,6.84524486089555,2.55612861974682));
#31325=CARTESIAN_POINT('Ctrl Pts',(105.2952795156,6.93687390358686,0.257327369497228));
#31326=CARTESIAN_POINT('Ctrl Pts',(105.262194248193,6.98268842493251,-0.892073255627436));
#31327=CARTESIAN_POINT('Ctrl Pts',(105.229108980786,6.71970650709327,-2.05522120362623));
#31328=CARTESIAN_POINT('Ctrl Pts',(105.196023713379,6.20299267374967,-3.08870606767955));
#31329=CARTESIAN_POINT('Ctrl Pts',(105.162938445972,5.686278840406,-4.122190931733));
#31330=CARTESIAN_POINT('Ctrl Pts',(105.129853178565,4.91583309155763,-5.0260127118412));
#31331=CARTESIAN_POINT('Ctrl Pts',(105.096767911158,3.97388357095785,-5.68450421781766));
#31332=CARTESIAN_POINT('Ctrl Pts',(105.063682643751,3.03193405035818,-6.34299572379403));
#31333=CARTESIAN_POINT('Ctrl Pts',(105.030597376344,1.91848075800698,-6.75615695563902));
#31334=CARTESIAN_POINT('Ctrl Pts',(104.997512108937,0.770396244159204,-6.88648770729243));
#31335=CARTESIAN_POINT('Ctrl Pts',(104.96442684153,-0.377688269688576,-7.01681845894584));
#31336=CARTESIAN_POINT('Ctrl Pts',(104.931341574123,-1.56040400503286,-6.86431873040768));
#31337=CARTESIAN_POINT('Ctrl Pts',(104.898256306716,-2.62415213036371,-6.4265280307381));
#31338=CARTESIAN_POINT('Ctrl Pts',(104.832085771902,-4.75164838102565,-5.55094663139886));
#31339=CARTESIAN_POINT('Ctrl Pts',(104.765915237088,-6.40327419163353,-3.53420134753374));
#31340=CARTESIAN_POINT('Ctrl Pts',(104.699744702274,-6.82566286200369,-1.28080076989636));
#31341=CARTESIAN_POINT('Ctrl Pts',(104.687460356051,-6.90407795539624,-0.862464225520248));
#31342=CARTESIAN_POINT('Ctrl Pts',(104.675176009829,-6.94012772985068,-0.435971421728557));
#31343=CARTESIAN_POINT('Ctrl Pts',(104.662891663606,-6.93617806097948,-0.00865909541846954));
#31344=CARTESIAN_POINT('Ctrl Pts',(104.483548336394,-6.933,-4.16056078478277E-13));
#31345=CARTESIAN_POINT('Ctrl Pts',(104.540772531679,-6.93299999999988,-1.9942093570165));
#31346=CARTESIAN_POINT('Ctrl Pts',(104.597996726964,-6.02307502629244,-3.97063309653042));
#31347=CARTESIAN_POINT('Ctrl Pts',(104.655220922249,-4.50798484753998,-5.26731066241113));
#31348=CARTESIAN_POINT('Ctrl Pts',(104.712445117534,-2.99289466878752,-6.56398822829183));
#31349=CARTESIAN_POINT('Ctrl Pts',(104.769669312819,-0.899664345629392,
-7.15779044292397));
#31350=CARTESIAN_POINT('Ctrl Pts',(104.826893508104,1.07062371681769,-6.84983604599318));
#31351=CARTESIAN_POINT('Ctrl Pts',(104.884117703389,3.04091177926477,-6.54188164906239));
#31352=CARTESIAN_POINT('Ctrl Pts',(104.941341898675,4.85311303639787,-5.33766370386479));
#31353=CARTESIAN_POINT('Ctrl Pts',(104.99856609396,5.9002697149369,-3.6405090703085));
#31354=CARTESIAN_POINT('Ctrl Pts',(105.055790289245,6.94742639347593,-1.94335443675221));
#31355=CARTESIAN_POINT('Ctrl Pts',(105.11301448453,7.2108600852751,0.216464293122072));
#31356=CARTESIAN_POINT('Ctrl Pts',(105.170238679815,6.60233935006142,2.1155623617919));
#31357=CARTESIAN_POINT('Ctrl Pts',(105.2274628751,5.99381861484774,4.01466043046174));
#31358=CARTESIAN_POINT('Ctrl Pts',(105.284687070385,4.52419779647485,5.61916312790282));
#31359=CARTESIAN_POINT('Ctrl Pts',(105.34191126567,2.68569473000639,6.39167683923522));
#31360=CARTESIAN_POINT('Ctrl Pts',(105.399135460955,0.847191663537936,7.16419055056762));
#31361=CARTESIAN_POINT('Ctrl Pts',(105.45635965624,-1.32739978993864,7.09093574623839));
#31362=CARTESIAN_POINT('Ctrl Pts',(105.513583851525,-3.10974706735908,6.19644754492859));
#31363=CARTESIAN_POINT('Ctrl Pts',(105.57080804681,-4.89209434477952,5.3019593436188));
#31364=CARTESIAN_POINT('Ctrl Pts',(105.628032242096,-6.25040525058464,3.60219296582991));
#31365=CARTESIAN_POINT('Ctrl Pts',(105.685256437381,-6.72974280712672,1.66644854403793));
#31366=CARTESIAN_POINT('Ctrl Pts',(105.701353737052,-6.86458158035544,1.12191912096977));
#31367=CARTESIAN_POINT('Ctrl Pts',(105.717451036723,-6.93300000000002,0.560975745779151));
#31368=CARTESIAN_POINT('Ctrl Pts',(105.733548336394,-6.933,-2.66453525910038E-13));
#31369=CARTESIAN_POINT('Origin',(29.75,0.,0.));
#31370=CARTESIAN_POINT('',(107.162891663606,-6.92488577809423,0.00304253374609986));
#31371=CARTESIAN_POINT('',(106.983548336394,-6.9289346271905,0.00268695564041597));
#31372=CARTESIAN_POINT('',(29.75,-6.933,-8.4904762584886E-16));
#31373=CARTESIAN_POINT('Ctrl Pts',(107.162891663606,-6.92488577809423,0.00304253374609986));
#31374=CARTESIAN_POINT('Ctrl Pts',(107.135889094264,-6.92884091747773,0.947002408294073));
#31375=CARTESIAN_POINT('Ctrl Pts',(107.108886524921,-6.74871798472496,1.88952811505199));
#31376=CARTESIAN_POINT('Ctrl Pts',(107.081883955579,-6.377079692959,2.74976127902586));
#31377=CARTESIAN_POINT('Ctrl Pts',(107.015713420765,-5.46636989302528,4.85778617854933));
#31378=CARTESIAN_POINT('Ctrl Pts',(106.949542885951,-3.40559421461705,6.4716374201663));
#31379=CARTESIAN_POINT('Ctrl Pts',(106.883372351137,-1.1443604745777,6.84985187732506));
#31380=CARTESIAN_POINT('Ctrl Pts',(106.817201816323,1.11687326546152,7.2280663344838));
#31381=CARTESIAN_POINT('Ctrl Pts',(106.751031281509,3.57856506713182,6.37064400718454));
#31382=CARTESIAN_POINT('Ctrl Pts',(106.684860746695,5.1323120236005,4.67395393953337));
#31383=CARTESIAN_POINT('Ctrl Pts',(106.651775479288,5.90918550183488,3.82560890570773));
#31384=CARTESIAN_POINT('Ctrl Pts',(106.618690211881,6.45907276876884,2.76744693679409));
#31385=CARTESIAN_POINT('Ctrl Pts',(106.585604944474,6.7314677163284,1.64455469040912));
#31386=CARTESIAN_POINT('Ctrl Pts',(106.552519677067,7.00386266388793,0.521662444024272));
#31387=CARTESIAN_POINT('Ctrl Pts',(106.51943440966,6.99876529207313,-0.665960079831897));
#31388=CARTESIAN_POINT('Ctrl Pts',(106.486349142253,6.70432462161403,-1.77689798385835));
#31389=CARTESIAN_POINT('Ctrl Pts',(106.453263874846,6.4098839511549,-2.88783588788493));
#31390=CARTESIAN_POINT('Ctrl Pts',(106.420178607439,5.8260999820514,-3.92208917208177));
#31391=CARTESIAN_POINT('Ctrl Pts',(106.387093340031,5.03331171364945,-4.76266734495707));
#31392=CARTESIAN_POINT('Ctrl Pts',(106.354008072624,4.2405234452475,-5.60324551783236));
#31393=CARTESIAN_POINT('Ctrl Pts',(106.320922805217,3.2387308775471,-6.25014857938612));
#31394=CARTESIAN_POINT('Ctrl Pts',(106.28783753781,2.14366517559393,-6.60235830564033));
#31395=CARTESIAN_POINT('Ctrl Pts',(106.221667002996,-0.0464662283121736,
-7.30677775814868));
#31396=CARTESIAN_POINT('Ctrl Pts',(106.155496468182,-2.60969016922931,-6.83242386945914));
#31397=CARTESIAN_POINT('Ctrl Pts',(106.089325933368,-4.38676837012615,-5.38390087275648));
#31398=CARTESIAN_POINT('Ctrl Pts',(106.030514510114,-5.96621001318147,-4.09647438766379));
#31399=CARTESIAN_POINT('Ctrl Pts',(105.97170308686,-6.92464371329922,-2.03951278580644));
#31400=CARTESIAN_POINT('Ctrl Pts',(105.912891663606,-6.94073003849348,0.00450623896247018));
#31401=CARTESIAN_POINT('Ctrl Pts',(105.733548336394,-6.93549738005571,0.00309879224510982));
#31402=CARTESIAN_POINT('Ctrl Pts',(105.790990515821,-6.91749353528686,-1.99592298257485));
#31403=CARTESIAN_POINT('Ctrl Pts',(105.848432695249,-6.01582286335993,-4.00079412588348));
#31404=CARTESIAN_POINT('Ctrl Pts',(105.905874874676,-4.499576288691,-5.28998465377729));
#31405=CARTESIAN_POINT('Ctrl Pts',(105.97204540949,-2.75293561878853,-6.77506804647284));
#31406=CARTESIAN_POINT('Ctrl Pts',(106.038215944304,-0.190759207781901,
-7.31045081068274));
#31407=CARTESIAN_POINT('Ctrl Pts',(106.104386479118,2.00795219744992,-6.64803671598811));
#31408=CARTESIAN_POINT('Ctrl Pts',(106.170557013932,4.20666360268163,-5.98562262129351));
#31409=CARTESIAN_POINT('Ctrl Pts',(106.236727548746,6.04191000213856,-4.12541166769451));
#31410=CARTESIAN_POINT('Ctrl Pts',(106.30289808356,6.6745582169174,-1.91795138426491));
#31411=CARTESIAN_POINT('Ctrl Pts',(106.369068618374,7.30720643169628,0.289508899164824));
#31412=CARTESIAN_POINT('Ctrl Pts',(106.435239153188,6.73725646179693,2.8442185124252));
#31413=CARTESIAN_POINT('Ctrl Pts',(106.501409688002,5.22871076598718,4.57063552106892));
#31414=CARTESIAN_POINT('Ctrl Pts',(106.567580222817,3.72016507017752,6.29705252971253));
#31415=CARTESIAN_POINT('Ctrl Pts',(106.63375075763,1.27302364845756,7.19517693373959));
#31416=CARTESIAN_POINT('Ctrl Pts',(106.699921292445,-1.00430731665786,6.86860993177073));
#31417=CARTESIAN_POINT('Ctrl Pts',(106.733006559852,-2.14297279921577,6.70532643078627));
#31418=CARTESIAN_POINT('Ctrl Pts',(106.766091827259,-3.23918566762253,6.23587007830273));
#31419=CARTESIAN_POINT('Ctrl Pts',(106.799177094666,-4.16189215621188,5.54038633360014));
#31420=CARTESIAN_POINT('Ctrl Pts',(106.832262362073,-5.08459864480092,4.84490258889778));
#31421=CARTESIAN_POINT('Ctrl Pts',(106.86534762948,-5.83379875357268,3.92339145197653));
#31422=CARTESIAN_POINT('Ctrl Pts',(106.898432896887,-6.31064547973526,2.87768808353459));
#31423=CARTESIAN_POINT('Ctrl Pts',(106.926804710056,-6.7195587902587,1.98095963232713));
#31424=CARTESIAN_POINT('Ctrl Pts',(106.955176523225,-6.92819206609309,0.992904155184515));
#31425=CARTESIAN_POINT('Ctrl Pts',(106.983548336394,-6.9289346271905,0.00268695564041597));
#31426=CARTESIAN_POINT('Origin',(29.75,0.,0.));
#31427=CARTESIAN_POINT('',(108.412891663606,-6.92776634541837,-0.00844704756396031));
#31428=CARTESIAN_POINT('',(108.233548336394,-6.93028901950621,-0.00380765172104063));
#31429=CARTESIAN_POINT('',(29.75,-6.933,-8.4904762584886E-16));
#31430=CARTESIAN_POINT('Ctrl Pts',(108.412891663606,-6.92776634541837,-0.00844704756396031));
#31431=CARTESIAN_POINT('Ctrl Pts',(108.366245636481,-6.91355352143459,1.621272426568));
#31432=CARTESIAN_POINT('Ctrl Pts',(108.319599609356,-6.3407349699669,3.26180305496299));
#31433=CARTESIAN_POINT('Ctrl Pts',(108.272953582232,-5.29536157004919,4.49505663430979));
#31434=CARTESIAN_POINT('Ctrl Pts',(108.206783047418,-3.81242891283097,6.24450999479188));
#31435=CARTESIAN_POINT('Ctrl Pts',(108.140612512604,-1.37855827834812,7.17438608402479));
#31436=CARTESIAN_POINT('Ctrl Pts',(108.074441977789,0.903318468414054,6.88158564177937));
#31437=CARTESIAN_POINT('Ctrl Pts',(108.041356710382,2.04425684179514,6.73518542065666));
#31438=CARTESIAN_POINT('Ctrl Pts',(108.008271442975,3.14719674324603,6.28311606666432));
#31439=CARTESIAN_POINT('Ctrl Pts',(107.975186175568,4.08001313168627,5.60148092342676));
#31440=CARTESIAN_POINT('Ctrl Pts',(107.942100908161,5.0128295201265,4.9198457801892));
#31441=CARTESIAN_POINT('Ctrl Pts',(107.909015640754,5.77552239555616,4.00864484770638));
#31442=CARTESIAN_POINT('Ctrl Pts',(107.875930373347,6.26769096176187,2.96986524175247));
#31443=CARTESIAN_POINT('Ctrl Pts',(107.84284510594,6.75985952796753,1.93108563579867));
#31444=CARTESIAN_POINT('Ctrl Pts',(107.809759838533,6.98150378494936,0.764727356373722));
#31445=CARTESIAN_POINT('Ctrl Pts',(107.776674571126,6.9185152599161,-0.388891218753205));
#31446=CARTESIAN_POINT('Ctrl Pts',(107.743589303719,6.85552673488282,-1.5425097938804));
#31447=CARTESIAN_POINT('Ctrl Pts',(107.710504036312,6.50790542783433,-2.68338866470967));
#31448=CARTESIAN_POINT('Ctrl Pts',(107.677418768905,5.89882838853818,-3.65929881778214));
#31449=CARTESIAN_POINT('Ctrl Pts',(107.611248234091,4.68067430994609,-5.61111912392676));
#31450=CARTESIAN_POINT('Ctrl Pts',(107.545077699277,2.41669730236367,-6.90306455904472));
#31451=CARTESIAN_POINT('Ctrl Pts',(107.478907164463,0.124409193473775,-6.94364573346948));
#31452=CARTESIAN_POINT('Ctrl Pts',(107.412736629649,-2.16787891541625,-6.98422690789425));
#31453=CARTESIAN_POINT('Ctrl Pts',(107.346566094835,-4.48847812561356,-5.77344382162591));
#31454=CARTESIAN_POINT('Ctrl Pts',(107.280395560021,-5.76845576998274,-3.86695299977675));
#31455=CARTESIAN_POINT('Ctrl Pts',(107.241227594549,-6.5261059887696,-2.73845423681513));
#31456=CARTESIAN_POINT('Ctrl Pts',(107.202059629078,-6.91914874022781,-1.36619708578935));
#31457=CARTESIAN_POINT('Ctrl Pts',(107.162891663606,-6.92488577809423,0.00304253374609986));
#31458=CARTESIAN_POINT('Ctrl Pts',(106.983548336394,-6.9289346271905,0.00268695564041597));
#31459=CARTESIAN_POINT('Ctrl Pts',(106.988261790632,-6.92905799004118,-0.161819395360096));
#31460=CARTESIAN_POINT('Ctrl Pts',(106.99297524487,-6.92344363092686,-0.326385409256667));
#31461=CARTESIAN_POINT('Ctrl Pts',(106.997688699108,-6.91205665349178,-0.490602246874311));
#31462=CARTESIAN_POINT('Ctrl Pts',(107.030773966515,-6.83212775753224,-1.64329360887824));
#31463=CARTESIAN_POINT('Ctrl Pts',(107.063859233922,-6.46777662205971,-2.77878073292303));
#31464=CARTESIAN_POINT('Ctrl Pts',(107.096944501329,-5.8444237086234,-3.74555518589093));
#31465=CARTESIAN_POINT('Ctrl Pts',(107.163115036143,-4.59771788175101,-5.6791040918264));
#31466=CARTESIAN_POINT('Ctrl Pts',(107.229285570957,-2.31500494302391,-6.93780231345459));
#31467=CARTESIAN_POINT('Ctrl Pts',(107.295456105771,-0.0223697880795398,
-6.94474846410226));
#31468=CARTESIAN_POINT('Ctrl Pts',(107.361626640585,2.27026536686496,-6.95169461474993));
#31469=CARTESIAN_POINT('Ctrl Pts',(107.427797175399,4.57282273802673,-5.70688869441693));
#31470=CARTESIAN_POINT('Ctrl Pts',(107.493967710213,5.82465096202989,-3.78176859055449));
#31471=CARTESIAN_POINT('Ctrl Pts',(107.560138245027,7.07647918603296,-1.85664848669215));
#31472=CARTESIAN_POINT('Ctrl Pts',(107.626308779841,7.27757826287754,0.748785800699566));
#31473=CARTESIAN_POINT('Ctrl Pts',(107.692479314655,6.3359900190534,2.84317392207816));
#31474=CARTESIAN_POINT('Ctrl Pts',(107.758649849469,5.3944017752292,4.93756204345687));
#31475=CARTESIAN_POINT('Ctrl Pts',(107.824820384283,3.31012621073615,6.5209039988224));
#31476=CARTESIAN_POINT('Ctrl Pts',(107.890990919097,1.04358538120297,6.86590294655329));
#31477=CARTESIAN_POINT('Ctrl Pts',(107.957161453911,-1.22295544833022,7.21090189428418));
#31478=CARTESIAN_POINT('Ctrl Pts',(108.023331988725,-3.67176154290354,6.31755783438044));
#31479=CARTESIAN_POINT('Ctrl Pts',(108.089502523539,-5.20043113550107,4.59806048243787));
#31480=CARTESIAN_POINT('Ctrl Pts',(108.122587790946,-5.96476593179974,3.73831180646669));
#31481=CARTESIAN_POINT('Ctrl Pts',(108.155673058353,-6.49906660260453,2.67202480748586));
#31482=CARTESIAN_POINT('Ctrl Pts',(108.18875832576,-6.75491755697916,1.54537328180927));
#31483=CARTESIAN_POINT('Ctrl Pts',(108.203688329305,-6.87037243931928,1.03696236087581));
#31484=CARTESIAN_POINT('Ctrl Pts',(108.218618332849,-6.92912546191901,0.516259163369478));
#31485=CARTESIAN_POINT('Ctrl Pts',(108.233548336394,-6.93028901950621,-0.00380765172104063));
#31486=CARTESIAN_POINT('Origin',(-87.75,0.,0.));
#31487=CARTESIAN_POINT('',(-86.1648283363937,-6.93261614350334,-0.000140194423062512));
#31488=CARTESIAN_POINT('',(-86.3441716636063,-6.93270425418277,-0.000130097846330653));
#31489=CARTESIAN_POINT('',(-87.75,-6.933,-8.4904762584886E-16));
#31490=CARTESIAN_POINT('',(-86.51072,1.15840596835136,6.8358145694558));
#31491=CARTESIAN_POINT('Ctrl Pts',(-86.1648283363937,-6.93261614350334,
-0.000140194423062512));
#31492=CARTESIAN_POINT('Ctrl Pts',(-86.1862819769683,-6.93206966311315,
0.747603057917331));
#31493=CARTESIAN_POINT('Ctrl Pts',(-86.2077356175428,-6.81152017995217,
1.49551828662709));
#31494=CARTESIAN_POINT('Ctrl Pts',(-86.2291892581174,-6.57390952823857,
2.20418517192447));
#31495=CARTESIAN_POINT('Ctrl Pts',(-86.2622185198563,-6.20809262270579,
3.2952234951791));
#31496=CARTESIAN_POINT('Ctrl Pts',(-86.2952477815952,-5.56481047477723,
4.29323309462037));
#31497=CARTESIAN_POINT('Ctrl Pts',(-86.3282770433341,-4.72221552560607,
5.07695161393405));
#31498=CARTESIAN_POINT('Ctrl Pts',(-86.361306305073,-3.87962057643491,5.86067013324773));
#31499=CARTESIAN_POINT('Ctrl Pts',(-86.3943355668118,-2.83771282602114,
6.43009757243381));
#31500=CARTESIAN_POINT('Ctrl Pts',(-86.4273648285507,-1.72308180962127,
6.71607370144116));
#31501=CARTESIAN_POINT('Ctrl Pts',(-86.4551498857004,-0.785425777936701,
6.95664411293718));
#31502=CARTESIAN_POINT('Ctrl Pts',(-86.4829349428502,0.2036936247524,6.99662727440187));
#31503=CARTESIAN_POINT('Ctrl Pts',(-86.51072,1.15840596835136,6.8358145694558));
#31504=CARTESIAN_POINT('',(-86.51072,-6.933,-8.4904762584886E-16));
#31505=CARTESIAN_POINT('Origin',(-86.51072,0.,0.));
#31506=CARTESIAN_POINT('',(-109.067,-6.933,-8.4904762584886E-16));
#31507=CARTESIAN_POINT('',(-87.75,-6.933,-8.4904762584886E-16));
#31508=CARTESIAN_POINT('Origin',(-109.067,0.,0.));
#31509=CARTESIAN_POINT('',(-86.51072,-4.64214617842358,5.1494628708388));
#31510=CARTESIAN_POINT('Origin',(-86.51072,0.,0.));
#31511=CARTESIAN_POINT('Ctrl Pts',(-86.51072,-4.64214617842358,5.14946287083879));
#31512=CARTESIAN_POINT('Ctrl Pts',(-86.4776907382611,-5.49707636744032,
4.37875901117264));
#31513=CARTESIAN_POINT('Ctrl Pts',(-86.4446614765222,-6.15592316322177,
3.39140242300292));
#31514=CARTESIAN_POINT('Ctrl Pts',(-86.4116322147833,-6.53873675821753,
2.30636006071919));
#31515=CARTESIAN_POINT('Ctrl Pts',(-86.389145364391,-6.79936238487788,1.56764584231125));
#31516=CARTESIAN_POINT('Ctrl Pts',(-86.3666585139986,-6.93204373903408,
0.783653246999931));
#31517=CARTESIAN_POINT('Ctrl Pts',(-86.3441716636063,-6.93270425418277,
-0.000130097846330653));
#31518=CARTESIAN_POINT('Origin',(-87.75,0.,0.));
#31519=CARTESIAN_POINT('',(-84.9148283363937,-6.93288145074965,0.000176808201168416));
#31520=CARTESIAN_POINT('',(-85.0941716636063,-6.9327762777167,0.000168448225849813));
#31521=CARTESIAN_POINT('',(-87.75,-6.933,-8.4904762584886E-16));
#31522=CARTESIAN_POINT('Ctrl Pts',(-84.9148283363937,-6.93288145074965,
0.000176808201168416));
#31523=CARTESIAN_POINT('Ctrl Pts',(-84.9235682410294,-6.93318021234269,
0.304763539330887));
#31524=CARTESIAN_POINT('Ctrl Pts',(-84.932308145665,-6.91347845811148,0.609311906094795));
#31525=CARTESIAN_POINT('Ctrl Pts',(-84.9410480503007,-6.87346355102493,
0.911167498725949));
#31526=CARTESIAN_POINT('Ctrl Pts',(-84.9740773120396,-6.72224189647419,
2.05191992017604));
#31527=CARTESIAN_POINT('Ctrl Pts',(-85.0071065737784,-6.28091092139654,
3.15421455619275));
#31528=CARTESIAN_POINT('Ctrl Pts',(-85.0401358355174,-5.60308949675388,
4.08412970976292));
#31529=CARTESIAN_POINT('Ctrl Pts',(-85.0731650972563,-4.92526807211124,
5.01404486333308));
#31530=CARTESIAN_POINT('Ctrl Pts',(-85.1061943589952,-4.01095619790362,
5.77158053445669));
#31531=CARTESIAN_POINT('Ctrl Pts',(-85.1392236207341,-2.97123687706053,
6.26470101639398));
#31532=CARTESIAN_POINT('Ctrl Pts',(-85.1722528824729,-1.93151755621743,
6.75782149833127));
#31533=CARTESIAN_POINT('Ctrl Pts',(-85.2052821442118,-0.766390788738866,
6.98652679108223));
#31534=CARTESIAN_POINT('Ctrl Pts',(-85.2383114059506,0.382588027107184,
6.92303067917854));
#31535=CARTESIAN_POINT('Ctrl Pts',(-85.2713406676895,1.53156684295325,6.85953456727484));
#31536=CARTESIAN_POINT('Ctrl Pts',(-85.3043699294285,2.6643977071668,6.50383705071648));
#31537=CARTESIAN_POINT('Ctrl Pts',(-85.3373991911674,3.64344896848527,5.8991530776003));
#31538=CARTESIAN_POINT('Ctrl Pts',(-85.3704284529063,4.62250022980373,5.29446910448412));
#31539=CARTESIAN_POINT('Ctrl Pts',(-85.4034577146451,5.44777188822712,4.44079867481011));
#31540=CARTESIAN_POINT('Ctrl Pts',(-85.436486976384,6.01899874927411,3.4418572653518));
#31541=CARTESIAN_POINT('Ctrl Pts',(-85.4695162381229,6.5902256103211,2.44291585589349));
#31542=CARTESIAN_POINT('Ctrl Pts',(-85.5025454998618,6.90740767399169,1.29870346665087));
#31543=CARTESIAN_POINT('Ctrl Pts',(-85.5355747616007,6.9320093702799,0.148234495631678));
#31544=CARTESIAN_POINT('Ctrl Pts',(-85.5686040233396,6.95661106656811,-1.0022344753875));
#31545=CARTESIAN_POINT('Ctrl Pts',(-85.6016332850785,6.68863239547394,-2.15896002818325));
#31546=CARTESIAN_POINT('Ctrl Pts',(-85.6346625468174,6.1606310238489,-3.18140738363518));
#31547=CARTESIAN_POINT('Ctrl Pts',(-85.6676918085563,5.63262965222386,-4.20385473908712));
#31548=CARTESIAN_POINT('Ctrl Pts',(-85.7007210702952,4.84460558006794,-5.09202389719524));
#31549=CARTESIAN_POINT('Ctrl Pts',(-85.7337503320341,3.89229868783116,-5.73800817878655));
#31550=CARTESIAN_POINT('Ctrl Pts',(-85.766779593773,2.93999179559439,-6.38399246037785));
#31551=CARTESIAN_POINT('Ctrl Pts',(-85.7998088555118,1.82340208327677,-6.78779186545236));
#31552=CARTESIAN_POINT('Ctrl Pts',(-85.8328381172507,0.678187944654679,
-6.90034705779794));
#31553=CARTESIAN_POINT('Ctrl Pts',(-85.8658673789896,-0.467026193967406,
-7.01290225014353));
#31554=CARTESIAN_POINT('Ctrl Pts',(-85.8988966407285,-1.64086475889396,
-6.83421322976019));
#31555=CARTESIAN_POINT('Ctrl Pts',(-85.9319259024674,-2.70071379568421,
-6.38599018928669));
#31556=CARTESIAN_POINT('Ctrl Pts',(-85.9649551642063,-3.76056283247446,
-5.93776714881318));
#31557=CARTESIAN_POINT('Ctrl Pts',(-85.9979844259452,-4.70642234112842,
-5.22001008824951));
#31558=CARTESIAN_POINT('Ctrl Pts',(-86.0310136876841,-5.4233767471659,-4.31992059426439));
#31559=CARTESIAN_POINT('Ctrl Pts',(-86.0640429494229,-6.14033115320338,
-3.41983110027927));
#31560=CARTESIAN_POINT('Ctrl Pts',(-86.0970722111618,-6.62838045662438,
-2.33740917287272));
#31561=CARTESIAN_POINT('Ctrl Pts',(-86.1301014729007,-6.82822927676637,
-1.20416468563544));
#31562=CARTESIAN_POINT('Ctrl Pts',(-86.141677094065,-6.89826942027279,-0.807001437648487));
#31563=CARTESIAN_POINT('Ctrl Pts',(-86.1532527152294,-6.9329110048789,-0.403595849755758));
#31564=CARTESIAN_POINT('Ctrl Pts',(-86.1648283363937,-6.93261614350334,
-0.000140194423062512));
#31565=CARTESIAN_POINT('Ctrl Pts',(-86.3441716636063,-6.93270425418277,
-0.000130097846330653));
#31566=CARTESIAN_POINT('Ctrl Pts',(-86.3336292522597,-6.93301392060011,
-0.367587802405469));
#31567=CARTESIAN_POINT('Ctrl Pts',(-86.3230868409132,-6.90430574294555,
-0.734999514245483));
#31568=CARTESIAN_POINT('Ctrl Pts',(-86.3125444295667,-6.84615964459705,
-1.09767788462958));
#31569=CARTESIAN_POINT('Ctrl Pts',(-86.2795151678278,-6.66398854177075,
-2.23394533129684));
#31570=CARTESIAN_POINT('Ctrl Pts',(-86.2464859060889,-6.19286594190809,
-3.32375208823362));
#31571=CARTESIAN_POINT('Ctrl Pts',(-86.21345664435,-5.49002272730517,-4.23488005538391));
#31572=CARTESIAN_POINT('Ctrl Pts',(-86.1804273826111,-4.78717951270224,
-5.1460080225342));
#31573=CARTESIAN_POINT('Ctrl Pts',(-86.1473981208722,-3.85261568335905,
-5.878457199898));
#31574=CARTESIAN_POINT('Ctrl Pts',(-86.1143688591333,-2.79987809561172,
-6.34314896472182));
#31575=CARTESIAN_POINT('Ctrl Pts',(-86.0813395973944,-1.7471405078644,-6.80784072954562));
#31576=CARTESIAN_POINT('Ctrl Pts',(-86.0483103356556,-0.576229161712943,
-7.00477508182944));
#31577=CARTESIAN_POINT('Ctrl Pts',(-86.0152810739167,0.570599361365794,
-6.91007040330406));
#31578=CARTESIAN_POINT('Ctrl Pts',(-85.9822518121778,1.71742788444454,-6.81536572477869));
#31579=CARTESIAN_POINT('Ctrl Pts',(-85.9492225504389,2.84017358445056,-6.42902201544412));
#31580=CARTESIAN_POINT('Ctrl Pts',(-85.9161932887,3.80242930172544,-5.7979555409898));
#31581=CARTESIAN_POINT('Ctrl Pts',(-85.8831640269611,4.76468501900033,-5.16688906653548));
#31582=CARTESIAN_POINT('Ctrl Pts',(-85.8501347652222,5.56645075354407,-4.29109982696142));
#31583=CARTESIAN_POINT('Ctrl Pts',(-85.8171055034833,6.11031752189778,-3.27700142574845));
#31584=CARTESIAN_POINT('Ctrl Pts',(-85.7840762417444,6.65418429025149,-2.26290302453548));
#31585=CARTESIAN_POINT('Ctrl Pts',(-85.7510469800056,6.94015209241517,-1.11049546168359));
#31586=CARTESIAN_POINT('Ctrl Pts',(-85.7180177182666,6.93347749064973,0.0402165186038079));
#31587=CARTESIAN_POINT('Ctrl Pts',(-85.6849884565277,6.92680288888429,1.19092849889121));
#31588=CARTESIAN_POINT('Ctrl Pts',(-85.6519591947888,6.62748588318974,2.33994489661413));
#31589=CARTESIAN_POINT('Ctrl Pts',(-85.6189299330499,6.07189165634794,3.34766498136383));
#31590=CARTESIAN_POINT('Ctrl Pts',(-85.5859006713111,5.51629742950615,4.35538506611354));
#31591=CARTESIAN_POINT('Ctrl Pts',(-85.5528714095722,4.70442598151711,5.22180883789003));
#31592=CARTESIAN_POINT('Ctrl Pts',(-85.5198421478333,3.73491441718631,5.84167269083401));
#31593=CARTESIAN_POINT('Ctrl Pts',(-85.4868128860944,2.76540285285553,6.46153654377797));
#31594=CARTESIAN_POINT('Ctrl Pts',(-85.4537836243555,1.63825117218298,6.83484047788943));
#31595=CARTESIAN_POINT('Ctrl Pts',(-85.4207543626166,0.490401067077939,
6.9162298278678));
#31596=CARTESIAN_POINT('Ctrl Pts',(-85.3877251008777,-0.65744903802711,
6.99761917784616));
#31597=CARTESIAN_POINT('Ctrl Pts',(-85.3546958391389,-1.82599756756465,
6.78709394369144));
#31598=CARTESIAN_POINT('Ctrl Pts',(-85.3216665774,-2.87327341347956,6.31023190183795));
#31599=CARTESIAN_POINT('Ctrl Pts',(-85.2886373156611,-3.92054925939447,
5.83336985998445));
#31600=CARTESIAN_POINT('Ctrl Pts',(-85.2556080539222,-4.84655242168673,
5.09017101043218));
#31601=CARTESIAN_POINT('Ctrl Pts',(-85.2225787921833,-5.53877947518409,
4.17092907015388));
#31602=CARTESIAN_POINT('Ctrl Pts',(-85.1895495304444,-6.23100652868145,
3.2516871298756));
#31603=CARTESIAN_POINT('Ctrl Pts',(-85.1565202687055,-6.68945747338392,
2.15640209887129));
#31604=CARTESIAN_POINT('Ctrl Pts',(-85.1234910069666,-6.85843347527675,
1.01814413035879));
#31605=CARTESIAN_POINT('Ctrl Pts',(-85.1137178925132,-6.90843222545892,
0.681342009507277));
#31606=CARTESIAN_POINT('Ctrl Pts',(-85.1039447780597,-6.93308673909412,
0.340777503273612));
#31607=CARTESIAN_POINT('Ctrl Pts',(-85.0941716636063,-6.9327762777167,0.000168448225849813));
#31608=CARTESIAN_POINT('Origin',(-87.75,0.,0.));
#31609=CARTESIAN_POINT('',(-83.6648283363937,-6.93338479581795,-0.000128863436223425));
#31610=CARTESIAN_POINT('',(-83.8441716636063,-6.93347143000264,-0.000100837253274565));
#31611=CARTESIAN_POINT('',(-87.75,-6.933,-8.4904762584886E-16));
#31612=CARTESIAN_POINT('Ctrl Pts',(-83.6648283363937,-6.93338479581795,
-0.000128863436223425));
#31613=CARTESIAN_POINT('Ctrl Pts',(-83.6938837668294,-6.93251907425441,
1.01224445621453));
#31614=CARTESIAN_POINT('Ctrl Pts',(-83.722939197265,-6.70811950439672,2.02498894125545));
#31615=CARTESIAN_POINT('Ctrl Pts',(-83.7519946277007,-6.27864669710701,
2.94165311522865));
#31616=CARTESIAN_POINT('Ctrl Pts',(-83.7850238894395,-5.79043607523614,
3.98368692697662));
#31617=CARTESIAN_POINT('Ctrl Pts',(-83.8180531511784,-5.03722165824491,
4.90156193873623));
#31618=CARTESIAN_POINT('Ctrl Pts',(-83.8510824129173,-4.11051414613749,
5.5837622488632));
#31619=CARTESIAN_POINT('Ctrl Pts',(-83.8841116746562,-3.18380663403007,
6.26596255899017));
#31620=CARTESIAN_POINT('Ctrl Pts',(-83.9171409363951,-2.08360602680646,
6.7124881674845));
#31621=CARTESIAN_POINT('Ctrl Pts',(-83.950170198134,-0.943579611550886,
6.86908908910737));
#31622=CARTESIAN_POINT('Ctrl Pts',(-83.9831994598728,0.196446803704693,
7.02569001073024));
#31623=CARTESIAN_POINT('Ctrl Pts',(-84.0162287216118,1.37629902699225,6.89236624548166));
#31624=CARTESIAN_POINT('Ctrl Pts',(-84.0492579833507,2.45263261293338,6.48531577206538));
#31625=CARTESIAN_POINT('Ctrl Pts',(-84.0822872450896,3.52896619887452,6.07826529864909));
#31626=CARTESIAN_POINT('Ctrl Pts',(-84.1153165068284,4.50178114746923,5.3974881170651));
#31627=CARTESIAN_POINT('Ctrl Pts',(-84.1483457685673,5.25288670863111,4.52569426980176));
#31628=CARTESIAN_POINT('Ctrl Pts',(-84.1813750303062,6.00399226979299,3.65390042253842));
#31629=CARTESIAN_POINT('Ctrl Pts',(-84.2144042920451,6.53338844352204,2.59108990959573));
#31630=CARTESIAN_POINT('Ctrl Pts',(-84.247433553784,6.7767570046951,1.46638736244647));
#31631=CARTESIAN_POINT('Ctrl Pts',(-84.2804628155229,7.02012556586816,0.34168481529722));
#31632=CARTESIAN_POINT('Ctrl Pts',(-84.3134920772618,6.97746651448524,-0.844909766058596));
#31633=CARTESIAN_POINT('Ctrl Pts',(-84.3465213390007,6.65396265051231,-1.94923278317452));
#31634=CARTESIAN_POINT('Ctrl Pts',(-84.3795506007396,6.33045878653939,-3.05355580029043));
#31635=CARTESIAN_POINT('Ctrl Pts',(-84.4125798624785,5.72611010997647,-4.07560725316645));
#31636=CARTESIAN_POINT('Ctrl Pts',(-84.4456091242173,4.91434109224742,-4.89121447357585));
#31637=CARTESIAN_POINT('Ctrl Pts',(-84.4786383859562,4.10257207451836,-5.70682169398526));
#31638=CARTESIAN_POINT('Ctrl Pts',(-84.5116676476951,3.08338271562318,-6.31598468192806));
#31639=CARTESIAN_POINT('Ctrl Pts',(-84.544696909434,1.98059795779642,-6.64469405818632));
#31640=CARTESIAN_POINT('Ctrl Pts',(-84.5777261711729,0.877813199969654,
-6.97340343444458));
#31641=CARTESIAN_POINT('Ctrl Pts',(-84.6107554329119,-0.308566956788687,
-7.02165919901831));
#31642=CARTESIAN_POINT('Ctrl Pts',(-84.6437846946507,-1.43440496524513,
-6.78359858727645));
#31643=CARTESIAN_POINT('Ctrl Pts',(-84.6768139563896,-2.56024297370157,
-6.5455379755346));
#31644=CARTESIAN_POINT('Ctrl Pts',(-84.7098432181284,-3.62553883385612,
-6.02116098747716));
#31645=CARTESIAN_POINT('Ctrl Pts',(-84.7428724798673,-4.5008659605355,-5.274176049627));
#31646=CARTESIAN_POINT('Ctrl Pts',(-84.7759017416062,-5.37619308721488,
-4.52719111177684));
#31647=CARTESIAN_POINT('Ctrl Pts',(-84.8089310033451,-6.0615514804191,-3.55759822413396));
#31648=CARTESIAN_POINT('Ctrl Pts',(-84.841960265084,-6.4736745100093,-2.48319667687079));
#31649=CARTESIAN_POINT('Ctrl Pts',(-84.8662496221873,-6.77674526936564,
-1.69309355376585));
#31650=CARTESIAN_POINT('Ctrl Pts',(-84.8905389792905,-6.93205115255709,
-0.846310217657153));
#31651=CARTESIAN_POINT('Ctrl Pts',(-84.9148283363937,-6.93288145074965,
0.000176808201168416));
#31652=CARTESIAN_POINT('Ctrl Pts',(-85.0941716636063,-6.9327762777167,0.000168448225849813));
#31653=CARTESIAN_POINT('Ctrl Pts',(-85.0709155163209,-6.93203750242105,
-0.810346397239332));
#31654=CARTESIAN_POINT('Ctrl Pts',(-85.0476593690354,-6.78993411546133,
-1.62111350115066));
#31655=CARTESIAN_POINT('Ctrl Pts',(-85.02440322175,-6.51157649632067,-2.38203667921726));
#31656=CARTESIAN_POINT('Ctrl Pts',(-84.9913739600111,-6.11624245638856,
-3.46272861426011));
#31657=CARTESIAN_POINT('Ctrl Pts',(-84.9583446982721,-5.44607331744114,
-4.44288157832512));
#31658=CARTESIAN_POINT('Ctrl Pts',(-84.9253154365332,-4.58249031378848,
-5.20341328099003));
#31659=CARTESIAN_POINT('Ctrl Pts',(-84.8922861747943,-3.71890731013583,
-5.96394498365495));
#31660=CARTESIAN_POINT('Ctrl Pts',(-84.8592569130555,-2.66191044177793,
-6.50485542491976));
#31661=CARTESIAN_POINT('Ctrl Pts',(-84.8262276513166,-1.53991801948317,
-6.76042747955588));
#31662=CARTESIAN_POINT('Ctrl Pts',(-84.7931983895778,-0.417925597188426,
-7.01599953419199));
#31663=CARTESIAN_POINT('Ctrl Pts',(-84.7601691278388,0.769062379043175,
-6.98623320219942));
#31664=CARTESIAN_POINT('Ctrl Pts',(-84.7271398660999,1.87683451565091,-6.67474489662896));
#31665=CARTESIAN_POINT('Ctrl Pts',(-84.694110604361,2.98460665225864,-6.3632565910585));
#31666=CARTESIAN_POINT('Ctrl Pts',(-84.6610813426221,4.01316294924251,-5.77004631191016));
#31667=CARTESIAN_POINT('Ctrl Pts',(-84.6280520808833,4.83754044181217,-4.96718528931603));
#31668=CARTESIAN_POINT('Ctrl Pts',(-84.5950228191444,5.66191793438184,-4.16432426672191));
#31669=CARTESIAN_POINT('Ctrl Pts',(-84.5619935574055,6.28211662253732,-3.15181250068199));
#31670=CARTESIAN_POINT('Ctrl Pts',(-84.5289642956666,6.62278636049758,-2.05266364779728));
#31671=CARTESIAN_POINT('Ctrl Pts',(-84.4959350339277,6.96345609845784,-0.953514794912575));
#31672=CARTESIAN_POINT('Ctrl Pts',(-84.4629057721888,7.0245968862229,0.232271144816923));
#31673=CARTESIAN_POINT('Ctrl Pts',(-84.4298765104499,6.79878051192343,1.36062881713992));
#31674=CARTESIAN_POINT('Ctrl Pts',(-84.396847248711,6.57296413762396,2.48898648946292));
#31675=CARTESIAN_POINT('Ctrl Pts',(-84.3638179869722,6.06019060125995,3.55991589437942));
#31676=CARTESIAN_POINT('Ctrl Pts',(-84.3307887252333,5.32275858457524,4.4433060076109));
#31677=CARTESIAN_POINT('Ctrl Pts',(-84.2977594634944,4.58532656789052,5.32669612084239));
#31678=CARTESIAN_POINT('Ctrl Pts',(-84.2647302017554,3.62323607088509,6.02254694238886));
#31679=CARTESIAN_POINT('Ctrl Pts',(-84.2317009400166,2.55337489186155,6.44631707946529));
#31680=CARTESIAN_POINT('Ctrl Pts',(-84.1986716782776,1.48351371283801,6.87008721654171));
#31681=CARTESIAN_POINT('Ctrl Pts',(-84.1656424165388,0.305881851796347,
7.02177666914809));
#31682=CARTESIAN_POINT('Ctrl Pts',(-84.1326131547999,-0.836446005598494,
6.88295614593155));
#31683=CARTESIAN_POINT('Ctrl Pts',(-84.099583893061,-1.97877386299333,6.74413562271501));
#31684=CARTESIAN_POINT('Ctrl Pts',(-84.0665546313221,-3.08579771674133,
6.31480512367556));
#31685=CARTESIAN_POINT('Ctrl Pts',(-84.0335253695832,-4.02302129925474,
5.64712553897888));
#31686=CARTESIAN_POINT('Ctrl Pts',(-84.0004961078443,-4.96024488176816,
4.97944595428219));
#31687=CARTESIAN_POINT('Ctrl Pts',(-83.9674668461054,-5.72766819304699,
4.07341728392825));
#31688=CARTESIAN_POINT('Ctrl Pts',(-83.9344375843665,-6.23205424395508,
3.03911617540227));
#31689=CARTESIAN_POINT('Ctrl Pts',(-83.9043489441131,-6.69153440293035,
2.09689971854705));
#31690=CARTESIAN_POINT('Ctrl Pts',(-83.8742603038597,-6.93272917490753,
1.04823446896903));
#31691=CARTESIAN_POINT('Ctrl Pts',(-83.8441716636063,-6.93347143000264,
-0.000100837253274565));
#31692=CARTESIAN_POINT('Origin',(-87.75,0.,0.));
#31693=CARTESIAN_POINT('',(-82.4148283363938,-6.93241284950548,5.58784473136953E-6));
#31694=CARTESIAN_POINT('',(-82.5941716636063,-6.93241904285695,-2.76930968138527E-5));
#31695=CARTESIAN_POINT('',(-87.75,-6.933,-8.4904762584886E-16));
#31696=CARTESIAN_POINT('Ctrl Pts',(-82.4148283363938,-6.93241284950548,
5.58784473136953E-6));
#31697=CARTESIAN_POINT('Ctrl Pts',(-82.4311700308905,-6.93242887600529,
0.569625986647833));
#31698=CARTESIAN_POINT('Ctrl Pts',(-82.4475117253872,-6.86301704074712,
1.1392425477305));
#31699=CARTESIAN_POINT('Ctrl Pts',(-82.4638534198839,-6.72413178121344,
1.69138380809983));
#31700=CARTESIAN_POINT('Ctrl Pts',(-82.4968826816228,-6.44342174898704,
2.80735242501566));
#31701=CARTESIAN_POINT('Ctrl Pts',(-82.5299119433617,-5.87890526500855,
3.85193254855472));
#31702=CARTESIAN_POINT('Ctrl Pts',(-82.5629412051006,-5.09916744587612,
4.6982144221336));
#31703=CARTESIAN_POINT('Ctrl Pts',(-82.5959704668395,-4.31942962674368,
5.54449629571249));
#31704=CARTESIAN_POINT('Ctrl Pts',(-82.6289997285784,-3.32447047245728,
6.1924799193312));
#31705=CARTESIAN_POINT('Ctrl Pts',(-82.6620289903173,-2.23517111145839,
6.56343945656001));
#31706=CARTESIAN_POINT('Ctrl Pts',(-82.6950582520562,-1.14587175045949,
6.93439899378882));
#31707=CARTESIAN_POINT('Ctrl Pts',(-82.728087513795,0.0377678172519116,
7.02833444462773));
#31708=CARTESIAN_POINT('Ctrl Pts',(-82.7611167755339,1.17194300834543,6.83383325686376));
#31709=CARTESIAN_POINT('Ctrl Pts',(-82.7941460372728,2.30611819943894,6.6393320690998));
#31710=CARTESIAN_POINT('Ctrl Pts',(-82.8271752990117,3.39082901391457,6.15639424273297));
#31711=CARTESIAN_POINT('Ctrl Pts',(-82.8602045607506,4.2942900747329,5.44369361293207));
#31712=CARTESIAN_POINT('Ctrl Pts',(-82.8932338224895,5.19775113555124,4.73099298313117));
#31713=CARTESIAN_POINT('Ctrl Pts',(-82.9262630842284,5.91996244271229,3.78852954989618));
#31714=CARTESIAN_POINT('Ctrl Pts',(-82.9592923459673,6.37317997435674,2.73080654970013));
#31715=CARTESIAN_POINT('Ctrl Pts',(-82.9923216077062,6.82639750600119,1.6730835495041));
#31716=CARTESIAN_POINT('Ctrl Pts',(-83.0253508694451,7.01062126212906,0.50010098234701));
#31717=CARTESIAN_POINT('Ctrl Pts',(-83.058380131184,6.90346924300647,-0.645631325363448));
#31718=CARTESIAN_POINT('Ctrl Pts',(-83.0914093929228,6.79631722388389,-1.79136363307392));
#31719=CARTESIAN_POINT('Ctrl Pts',(-83.1244386546617,6.39778942951084,-2.90984568133773));
#31720=CARTESIAN_POINT('Ctrl Pts',(-83.1574679164006,5.75630441987701,-3.86518910574001));
#31721=CARTESIAN_POINT('Ctrl Pts',(-83.1904971781395,5.11481941024318,-4.82053253014231));
#31722=CARTESIAN_POINT('Ctrl Pts',(-83.2235264398784,4.23037718534855,-5.61273733068305));
#31723=CARTESIAN_POINT('Ctrl Pts',(-83.2565557016173,3.2104317785833,-6.14555572690456));
#31724=CARTESIAN_POINT('Ctrl Pts',(-83.2895849633562,2.19048637181805,-6.67837412312607));
#31725=CARTESIAN_POINT('Ctrl Pts',(-83.3226142250951,1.03503778318217,-6.95180611502837));
#31726=CARTESIAN_POINT('Ctrl Pts',(-83.3556434868339,-0.115534426365817,
-6.93263147684566));
#31727=CARTESIAN_POINT('Ctrl Pts',(-83.3886727485728,-1.26610663591381,
-6.91345683866295));
#31728=CARTESIAN_POINT('Ctrl Pts',(-83.4217020103117,-2.4118024663739,-6.60167557039524));
#31729=CARTESIAN_POINT('Ctrl Pts',(-83.4547312720506,-3.41342725408578,
-6.03516708786852));
#31730=CARTESIAN_POINT('Ctrl Pts',(-83.4877605337895,-4.41505204179766,
-5.46865860534179));
#31731=CARTESIAN_POINT('Ctrl Pts',(-83.5207897955284,-5.27260578676133,
-4.64742290855603));
#31732=CARTESIAN_POINT('Ctrl Pts',(-83.5538190572673,-5.88190123270214,
-3.67123484486677));
#31733=CARTESIAN_POINT('Ctrl Pts',(-83.5868483190062,-6.49119667864295,
-2.69504678117752));
#31734=CARTESIAN_POINT('Ctrl Pts',(-83.6198775807451,-6.85223382556092,
-1.56390635058475));
#31735=CARTESIAN_POINT('Ctrl Pts',(-83.652906842484,-6.92114898564465,-0.415239829420204));
#31736=CARTESIAN_POINT('Ctrl Pts',(-83.6568806737872,-6.92944033719148,
-0.277040949442562));
#31737=CARTESIAN_POINT('Ctrl Pts',(-83.6608545050905,-6.93350319817502,
-0.138588377815766));
#31738=CARTESIAN_POINT('Ctrl Pts',(-83.6648283363937,-6.93338479581795,
-0.000128863436223425));
#31739=CARTESIAN_POINT('Ctrl Pts',(-83.8441716636063,-6.93347143000264,
-0.000100837253274565));
#31740=CARTESIAN_POINT('Ctrl Pts',(-83.8412310421208,-6.9335439720405,-0.102556691006701));
#31741=CARTESIAN_POINT('Ctrl Pts',(-83.8382904206354,-6.93131982367475,
-0.205009393294928));
#31742=CARTESIAN_POINT('Ctrl Pts',(-83.8353497991499,-6.92677829211024,
-0.307359267230395));
#31743=CARTESIAN_POINT('Ctrl Pts',(-83.802320537411,-6.87576749881995,-1.45696005463907));
#31744=CARTESIAN_POINT('Ctrl Pts',(-83.7692912756721,-6.53239712170201,
-2.59358808275837));
#31745=CARTESIAN_POINT('Ctrl Pts',(-83.7362620139332,-5.93838444983376,
-3.57915036750032));
#31746=CARTESIAN_POINT('Ctrl Pts',(-83.7032327521943,-5.34437177796551,
-4.56471265224226));
#31747=CARTESIAN_POINT('Ctrl Pts',(-83.6702034904554,-4.49971681134696,
-5.39920919360684));
#31748=CARTESIAN_POINT('Ctrl Pts',(-83.6371742287166,-3.50703968776827,
-5.98125403704088));
#31749=CARTESIAN_POINT('Ctrl Pts',(-83.6041449669777,-2.51436256418959,
-6.5632988804749));
#31750=CARTESIAN_POINT('Ctrl Pts',(-83.5711157052388,-1.37366328365078,
-6.8928920259784));
#31751=CARTESIAN_POINT('Ctrl Pts',(-83.5380864434999,-0.223529461180919,
-6.92999002937145));
#31752=CARTESIAN_POINT('Ctrl Pts',(-83.505057181761,0.92660436128894,-6.9670880327645));
#31753=CARTESIAN_POINT('Ctrl Pts',(-83.4720279200221,2.08617272568984,-6.7116908940471));
#31754=CARTESIAN_POINT('Ctrl Pts',(-83.4389986582832,3.11429554484444,-6.19482772049098));
#31755=CARTESIAN_POINT('Ctrl Pts',(-83.4059693965443,4.14241836399906,-5.67796454693485));
#31756=CARTESIAN_POINT('Ctrl Pts',(-83.3729401348054,5.03909563790738,-4.89963533853999));
#31757=CARTESIAN_POINT('Ctrl Pts',(-83.3399108730665,5.69538685353336,-3.95440208069459));
#31758=CARTESIAN_POINT('Ctrl Pts',(-83.3068816113276,6.35167806915934,-3.0091688228492));
#31759=CARTESIAN_POINT('Ctrl Pts',(-83.2738523495888,6.76758322650299,-1.89703151555327));
#31760=CARTESIAN_POINT('Ctrl Pts',(-83.2408230878499,6.89257252790607,-0.753107678062462));
#31761=CARTESIAN_POINT('Ctrl Pts',(-83.207793826111,7.01756182930914,0.390816159428331));
#31762=CARTESIAN_POINT('Ctrl Pts',(-83.1747645643721,6.85163527477164,1.566526527114));
#31763=CARTESIAN_POINT('Ctrl Pts',(-83.1417353026332,6.41495187189151,2.63118218839321));
#31764=CARTESIAN_POINT('Ctrl Pts',(-83.1087060408942,5.97826846901137,3.69583784967243));
#31765=CARTESIAN_POINT('Ctrl Pts',(-83.0756767791554,5.27082821778859,4.64943880454518));
#31766=CARTESIAN_POINT('Ctrl Pts',(-83.0426475174165,4.37858055193037,5.37612867939927));
#31767=CARTESIAN_POINT('Ctrl Pts',(-83.0096182556777,3.48633288607215,6.10281855425335));
#31768=CARTESIAN_POINT('Ctrl Pts',(-82.9765889939388,2.40927780557849,6.60259734908875));
#31769=CARTESIAN_POINT('Ctrl Pts',(-82.9435597321999,1.27827056512267,6.81474515954507));
#31770=CARTESIAN_POINT('Ctrl Pts',(-82.910530470461,0.14726332466687,7.02689297000139));
#31771=CARTESIAN_POINT('Ctrl Pts',(-82.8775012087221,-1.0376960757511,6.95140979607861));
#31772=CARTESIAN_POINT('Ctrl Pts',(-82.8444719469832,-2.13264270162839,
6.59746635720057));
#31773=CARTESIAN_POINT('Ctrl Pts',(-82.8114426852443,-3.22758932750568,
6.24352291832251));
#31774=CARTESIAN_POINT('Ctrl Pts',(-82.7784134235054,-4.23252317884229,
5.61111921448919));
#31775=CARTESIAN_POINT('Ctrl Pts',(-82.7453841617665,-5.02535126575494,
4.77708822223092));
#31776=CARTESIAN_POINT('Ctrl Pts',(-82.7123549000276,-5.81817935266758,
3.94305722997265));
#31777=CARTESIAN_POINT('Ctrl Pts',(-82.6793256382887,-6.39890167515627,
2.90739894928944));
#31778=CARTESIAN_POINT('Ctrl Pts',(-82.6462963765498,-6.69696421163009,
1.79593919032573));
#31779=CARTESIAN_POINT('Ctrl Pts',(-82.6289214722353,-6.8537587561742,1.21126045562967));
#31780=CARTESIAN_POINT('Ctrl Pts',(-82.6115465679208,-6.93233450307243,
0.605605618975589));
#31781=CARTESIAN_POINT('Ctrl Pts',(-82.5941716636063,-6.93241904285695,
-2.76930968138527E-5));
#31782=CARTESIAN_POINT('Origin',(-87.75,0.,0.));
#31783=CARTESIAN_POINT('',(-81.1648283363937,-6.93341558550125,0.000120073986537225));
#31784=CARTESIAN_POINT('',(-81.3441716636063,-6.93331923438577,0.000144398752376666));
#31785=CARTESIAN_POINT('',(-87.75,-6.933,-8.4904762584886E-16));
#31786=CARTESIAN_POINT('Ctrl Pts',(-81.1648283363937,-6.93341558550125,
0.000120073986537225));
#31787=CARTESIAN_POINT('Ctrl Pts',(-81.1684562949515,-6.93351814222822,
0.126526778809456));
#31788=CARTESIAN_POINT('Ctrl Pts',(-81.1720842535094,-6.93013211229906,
0.252927991280468));
#31789=CARTESIAN_POINT('Ctrl Pts',(-81.1757122120672,-6.92322057912816,
0.379136136715153));
#31790=CARTESIAN_POINT('Ctrl Pts',(-81.2087414738061,-6.86029735812661,
1.52814646930247));
#31791=CARTESIAN_POINT('Ctrl Pts',(-81.241770735545,-6.5051647142299,2.66115454536162));
#31792=CARTESIAN_POINT('Ctrl Pts',(-81.2747999972839,-5.90096897616487,
3.64050718166668));
#31793=CARTESIAN_POINT('Ctrl Pts',(-81.3078292590228,-5.29677323809984,
4.61985981797174));
#31794=CARTESIAN_POINT('Ctrl Pts',(-81.3408585207617,-4.44351440586649,
5.44555701452271));
#31795=CARTESIAN_POINT('Ctrl Pts',(-81.3738877825006,-3.44485793150741,
6.01728188048037));
#31796=CARTESIAN_POINT('Ctrl Pts',(-81.4069170442394,-2.44620145714835,
6.58900674643802));
#31797=CARTESIAN_POINT('Ctrl Pts',(-81.4399463059783,-1.30214734066357,
6.90675928180237));
#31798=CARTESIAN_POINT('Ctrl Pts',(-81.4729755677172,-0.15169078804013,
6.93193460025776));
#31799=CARTESIAN_POINT('Ctrl Pts',(-81.5060048294561,0.998765764583344,
6.95710991871314));
#31800=CARTESIAN_POINT('Ctrl Pts',(-81.539034091195,2.15562475334548,6.68970802025954));
#31801=CARTESIAN_POINT('Ctrl Pts',(-81.5720633529339,3.17833526275718,6.16221651315021));
#31802=CARTESIAN_POINT('Ctrl Pts',(-81.6050926146728,4.20104577216889,5.63472500604088));
#31803=CARTESIAN_POINT('Ctrl Pts',(-81.6381218764117,5.08960780223017,4.84714389027584));
#31804=CARTESIAN_POINT('Ctrl Pts',(-81.6711511381506,5.73606678975991,3.8951591983949));
#31805=CARTESIAN_POINT('Ctrl Pts',(-81.7041803998895,6.38252577728964,2.94317450651398));
#31806=CARTESIAN_POINT('Ctrl Pts',(-81.7372096616284,6.78688172228784,1.82678623851717));
#31807=CARTESIAN_POINT('Ctrl Pts',(-81.7702389233673,6.9000079820046,0.681628378003572));
#31808=CARTESIAN_POINT('Ctrl Pts',(-81.8032681851061,7.01313424172135,-0.463529482510025));
#31809=CARTESIAN_POINT('Ctrl Pts',(-81.836297446845,6.83503081615665,-1.63745693554042));
#31810=CARTESIAN_POINT('Ctrl Pts',(-81.8693267085839,6.38733612430369,-2.69752935713257));
#31811=CARTESIAN_POINT('Ctrl Pts',(-81.9023559703228,5.93964143245071,-3.75760177872474));
#31812=CARTESIAN_POINT('Ctrl Pts',(-81.9353852320616,5.22235547430947,-4.70381916887868));
#31813=CARTESIAN_POINT('Ctrl Pts',(-81.9684144938006,4.32262387355884,-5.42122220953598));
#31814=CARTESIAN_POINT('Ctrl Pts',(-82.0014437555395,3.42289227280822,-6.13862525019326));
#31815=CARTESIAN_POINT('Ctrl Pts',(-82.0344730172784,2.34071502944824,-6.62721394135391));
#31816=CARTESIAN_POINT('Ctrl Pts',(-82.0675022790173,1.20756970794717,-6.82762790417546));
#31817=CARTESIAN_POINT('Ctrl Pts',(-82.1005315407562,0.0744243864461097,
-7.028041866997));
#31818=CARTESIAN_POINT('Ctrl Pts',(-82.133560802495,-1.10968901319603,-6.94028110147943));
#31819=CARTESIAN_POINT('Ctrl Pts',(-82.1665900642339,-2.20090834012137,
-6.57500797534202));
#31820=CARTESIAN_POINT('Ctrl Pts',(-82.1996193259728,-3.29212766704672,
-6.2097348492046));
#31821=CARTESIAN_POINT('Ctrl Pts',(-82.2326485877117,-4.29045292125526,
-5.56694936244733));
#31822=CARTESIAN_POINT('Ctrl Pts',(-82.2656778494506,-5.07459401484698,
-4.72474581135389));
#31823=CARTESIAN_POINT('Ctrl Pts',(-82.2987071111895,-5.8587351084387,-3.88254226026045));
#31824=CARTESIAN_POINT('Ctrl Pts',(-82.3317363729284,-6.4286920414136,-2.84092064483084));
#31825=CARTESIAN_POINT('Ctrl Pts',(-82.3647656346673,-6.71521871766388,
-1.72643128196972));
#31826=CARTESIAN_POINT('Ctrl Pts',(-82.3814532019094,-6.85998226746399,
-1.16335129760796));
#31827=CARTESIAN_POINT('Ctrl Pts',(-82.3981407691516,-6.93239648380404,
-0.581670853936292));
#31828=CARTESIAN_POINT('Ctrl Pts',(-82.4148283363938,-6.93241284950548,
5.58784473136953E-6));
#31829=CARTESIAN_POINT('Ctrl Pts',(-82.5941716636063,-6.93241904285695,
-2.76930968138527E-5));
#31830=CARTESIAN_POINT('Ctrl Pts',(-82.5785173061819,-6.93249521110396,
-0.545688271345749));
#31831=CARTESIAN_POINT('Ctrl Pts',(-82.5628629487576,-6.86885565040568,
-1.0913313768807));
#31832=CARTESIAN_POINT('Ctrl Pts',(-82.5472085913332,-6.74130112803958,
-1.62159992855644));
#31833=CARTESIAN_POINT('Ctrl Pts',(-82.5141793295943,-6.47217275751627,
-2.74041805123071));
#31834=CARTESIAN_POINT('Ctrl Pts',(-82.4811500678554,-5.91851326601068,
-3.79079305933502));
#31835=CARTESIAN_POINT('Ctrl Pts',(-82.4481208061165,-5.14758871546834,
-4.64511115513774));
#31836=CARTESIAN_POINT('Ctrl Pts',(-82.4150915443776,-4.37666416492601,
-5.49942925094045));
#31837=CARTESIAN_POINT('Ctrl Pts',(-82.3820622826387,-3.38847455534694,
-6.15769043444157));
#31838=CARTESIAN_POINT('Ctrl Pts',(-82.3490330208998,-2.30307855909514,
-6.53992021188625));
#31839=CARTESIAN_POINT('Ctrl Pts',(-82.3160037591609,-1.21768256284332,
-6.92214998933094));
#31840=CARTESIAN_POINT('Ctrl Pts',(-82.2829744974221,-0.0350801799187911,
-7.02834836071917));
#31841=CARTESIAN_POINT('Ctrl Pts',(-82.2499452356832,1.10105001761894,-6.84561290798008));
#31842=CARTESIAN_POINT('Ctrl Pts',(-82.2169159739443,2.23718021515667,-6.66287745524098));
#31843=CARTESIAN_POINT('Ctrl Pts',(-82.1838867122054,3.32683822730758,-6.19120817837455));
#31844=CARTESIAN_POINT('Ctrl Pts',(-82.1508574504665,4.23763762438095,-5.48790985636909));
#31845=CARTESIAN_POINT('Ctrl Pts',(-82.1178281887276,5.14843702145431,-4.78461153436364));
#31846=CARTESIAN_POINT('Ctrl Pts',(-82.0847989269887,5.88037780345013,-3.84968416721917));
#31847=CARTESIAN_POINT('Ctrl Pts',(-82.0517696652499,6.34453387998692,-2.79671540792056));
#31848=CARTESIAN_POINT('Ctrl Pts',(-82.018740403511,6.8086899565237,-1.74374664862195));
#31849=CARTESIAN_POINT('Ctrl Pts',(-81.9857111417721,7.00506132760144,-0.572736497169197));
#31850=CARTESIAN_POINT('Ctrl Pts',(-81.9526818800332,6.90979013651598,0.574044855833212));
#31851=CARTESIAN_POINT('Ctrl Pts',(-81.9196526182943,6.81451894543051,1.72082620883562));
#31852=CARTESIAN_POINT('Ctrl Pts',(-81.8866233565553,6.42760519218184,2.84337876338767));
#31853=CARTESIAN_POINT('Ctrl Pts',(-81.8535940948165,5.79605640557224,3.80531961477969));
#31854=CARTESIAN_POINT('Ctrl Pts',(-81.8205648330776,5.16450761896264,4.76726046617172));
#31855=CARTESIAN_POINT('Ctrl Pts',(-81.7875355713387,4.28832379899209,5.56858961440372));
#31856=CARTESIAN_POINT('Ctrl Pts',(-81.7545063095998,3.27395563604716,6.11195072954594));
#31857=CARTESIAN_POINT('Ctrl Pts',(-81.721477047861,2.25958747310221,6.65531184468816));
#31858=CARTESIAN_POINT('Ctrl Pts',(-81.688447786122,1.10703496718287,6.94070492674061));
#31859=CARTESIAN_POINT('Ctrl Pts',(-81.6554185243831,-0.0436741761479686,
6.93345655452891));
#31860=CARTESIAN_POINT('Ctrl Pts',(-81.6223892626442,-1.19438331947877,
6.9262081823172));
#31861=CARTESIAN_POINT('Ctrl Pts',(-81.5893600009054,-2.34324910022105,
6.62631835584136));
#31862=CARTESIAN_POINT('Ctrl Pts',(-81.5563307391665,-3.35069172617371,
6.0702217573457));
#31863=CARTESIAN_POINT('Ctrl Pts',(-81.5233014774276,-4.35813435212639,
5.51412515885003));
#31864=CARTESIAN_POINT('Ctrl Pts',(-81.4902722156887,-5.22415382328944,
4.70182178833453));
#31865=CARTESIAN_POINT('Ctrl Pts',(-81.4572429539498,-5.84353435218509,
3.7320012730484));
#31866=CARTESIAN_POINT('Ctrl Pts',(-81.4242136922109,-6.46291488108073,
2.76218075776228));
#31867=CARTESIAN_POINT('Ctrl Pts',(-81.391184430472,-6.83565646770898,1.63484309770552));
#31868=CARTESIAN_POINT('Ctrl Pts',(-81.3581551687331,-6.91647341022511,
0.486952557084495));
#31869=CARTESIAN_POINT('Ctrl Pts',(-81.3534940003575,-6.92787849035219,
0.324959499870164));
#31870=CARTESIAN_POINT('Ctrl Pts',(-81.3488328319819,-6.9334697367279,0.162557121164403));
#31871=CARTESIAN_POINT('Ctrl Pts',(-81.3441716636063,-6.93331923438577,
0.000144398752376666));
#31872=CARTESIAN_POINT('Origin',(-87.75,0.,0.));
#31873=CARTESIAN_POINT('',(-79.9148283363937,-6.93284541734693,-0.000174722887704981));
#31874=CARTESIAN_POINT('',(-80.0941716636063,-6.93295492521967,-0.000178757583534305));
#31875=CARTESIAN_POINT('',(-87.75,-6.933,-8.4904762584886E-16));
#31876=CARTESIAN_POINT('Ctrl Pts',(-79.9148283363937,-6.93284541734693,
-0.000174722887704981));
#31877=CARTESIAN_POINT('Ctrl Pts',(-79.9387718207516,-6.9320436991393,0.834271057150727));
#31878=CARTESIAN_POINT('Ctrl Pts',(-79.9627153051094,-6.78122672642066,
1.66899880820083));
#31879=CARTESIAN_POINT('Ctrl Pts',(-79.9866587894672,-6.48653785546341,
2.44939871133041));
#31880=CARTESIAN_POINT('Ctrl Pts',(-80.0196880512061,-6.08002409560584,
3.52593511999483));
#31881=CARTESIAN_POINT('Ctrl Pts',(-80.052717312945,-5.39973204692025,4.49908938508927));
#31882=CARTESIAN_POINT('Ctrl Pts',(-80.0857465746839,-4.52831281137459,
5.25062953175785));
#31883=CARTESIAN_POINT('Ctrl Pts',(-80.1187758364227,-3.65689357582891,
6.00216967842645));
#31884=CARTESIAN_POINT('Ctrl Pts',(-80.1518050981616,-2.59434715342316,
6.53209570666917));
#31885=CARTESIAN_POINT('Ctrl Pts',(-80.1848343599005,-1.46976609032717,
6.77602501745318));
#31886=CARTESIAN_POINT('Ctrl Pts',(-80.2178636216394,-0.345185027231233,
7.01995432823717));
#31887=CARTESIAN_POINT('Ctrl Pts',(-80.2508928833782,0.841430676554926,
6.97788692156249));
#31888=CARTESIAN_POINT('Ctrl Pts',(-80.2839221451171,1.94591485633796,6.6549337163724));
#31889=CARTESIAN_POINT('Ctrl Pts',(-80.3169514068561,3.050399036121,6.33198051118231));
#31890=CARTESIAN_POINT('Ctrl Pts',(-80.349980668595,4.07275169190092,5.72814150747681));
#31891=CARTESIAN_POINT('Ctrl Pts',(-80.3830099303339,4.88876356125384,4.91677925471376));
#31892=CARTESIAN_POINT('Ctrl Pts',(-80.4160391920728,5.70477543060677,4.1054170019507));
#31893=CARTESIAN_POINT('Ctrl Pts',(-80.4490684538116,6.31444651353271,3.08653150013008));
#31894=CARTESIAN_POINT('Ctrl Pts',(-80.4820977155505,6.64370570051452,1.9839107748026));
#31895=CARTESIAN_POINT('Ctrl Pts',(-80.5151269772894,6.97296488749633,0.881290049475117));
#31896=CARTESIAN_POINT('Ctrl Pts',(-80.5481562390284,7.02181217853402,-0.305065899359219));
#31897=CARTESIAN_POINT('Ctrl Pts',(-80.5811855007673,6.78431294240529,-1.43102246556055));
#31898=CARTESIAN_POINT('Ctrl Pts',(-80.6142147625062,6.54681370627656,-2.55697903176186));
#31899=CARTESIAN_POINT('Ctrl Pts',(-80.647244024245,6.02296794298142,-3.62253621533017));
#31900=CARTESIAN_POINT('Ctrl Pts',(-80.6802732859838,5.27641953852623,-4.49823568200751));
#31901=CARTESIAN_POINT('Ctrl Pts',(-80.7133025477227,4.52987113407103,-5.37393514868486));
#31902=CARTESIAN_POINT('Ctrl Pts',(-80.7463318094616,3.56062008845578,-6.05977689847124));
#31903=CARTESIAN_POINT('Ctrl Pts',(-80.7793610712005,2.48642416051135,-6.47243557646211));
#31904=CARTESIAN_POINT('Ctrl Pts',(-80.8123903329394,1.41222823256689,-6.88509425445299));
#31905=CARTESIAN_POINT('Ctrl Pts',(-80.8454195946783,0.233087422293255,
-7.02456986064836));
#31906=CARTESIAN_POINT('Ctrl Pts',(-80.8784488564172,-0.90774025703015,
-6.87391700729604));
#31907=CARTESIAN_POINT('Ctrl Pts',(-80.9114781181561,-2.04856793635356,
-6.72326415394373));
#31908=CARTESIAN_POINT('Ctrl Pts',(-80.944507379895,-3.15108248472673,-6.28248284104374));
#31909=CARTESIAN_POINT('Ctrl Pts',(-80.9775366416339,-4.08133548612042,
-5.60512515892028));
#31910=CARTESIAN_POINT('Ctrl Pts',(-81.0105659033728,-5.01158848751409,
-4.92776747679684));
#31911=CARTESIAN_POINT('Ctrl Pts',(-81.0435951651117,-5.76957994192829,
-4.01383342544995));
#31912=CARTESIAN_POINT('Ctrl Pts',(-81.0766244268506,-6.26321877008219,
-2.97436010521878));
#31913=CARTESIAN_POINT('Ctrl Pts',(-81.1060257300316,-6.7026359439577,-2.04906330390524));
#31914=CARTESIAN_POINT('Ctrl Pts',(-81.1354270332127,-6.93258445654129,
-1.02429125634669));
#31915=CARTESIAN_POINT('Ctrl Pts',(-81.1648283363937,-6.93341558550125,
0.000120073986537225));
#31916=CARTESIAN_POINT('Ctrl Pts',(-81.3441716636063,-6.93331923438577,
0.000144398752376666));
#31917=CARTESIAN_POINT('Ctrl Pts',(-81.315803570243,-6.93240326994323,-0.988307187091753));
#31918=CARTESIAN_POINT('Ctrl Pts',(-81.2874354768797,-6.71881306293981,
-1.97714190358189));
#31919=CARTESIAN_POINT('Ctrl Pts',(-81.2590673835164,-6.30879853137859,
-2.87641935706139));
#31920=CARTESIAN_POINT('Ctrl Pts',(-81.2260381217775,-5.83141441161191,
-3.92345730940097));
#31921=CARTESIAN_POINT('Ctrl Pts',(-81.1930088600387,-5.08775387367453,
-4.84908979289483));
#31922=CARTESIAN_POINT('Ctrl Pts',(-81.1599795982998,-4.16816688280468,
-5.54085842305075));
#31923=CARTESIAN_POINT('Ctrl Pts',(-81.1269503365609,-3.24857989193482,
-6.23262705320668));
#31924=CARTESIAN_POINT('Ctrl Pts',(-81.093921074822,-2.15306644813249,-6.69053183002466));
#31925=CARTESIAN_POINT('Ctrl Pts',(-81.0608918130831,-1.01472437831761,
-6.85894027261136));
#31926=CARTESIAN_POINT('Ctrl Pts',(-81.0278625513442,0.123617691497245,
-7.02734871519806));
#31927=CARTESIAN_POINT('Ctrl Pts',(-80.9948332896053,1.30478838732467,-6.90626082355348));
#31928=CARTESIAN_POINT('Ctrl Pts',(-80.9618040278665,2.38528307786546,-6.51038799655218));
#31929=CARTESIAN_POINT('Ctrl Pts',(-80.9287747661276,3.46577776840626,-6.11451516955088));
#31930=CARTESIAN_POINT('Ctrl Pts',(-80.8957455043887,4.44559645366045,-5.44385740719286));
#31931=CARTESIAN_POINT('Ctrl Pts',(-80.8627162426498,5.2056974746501,-4.57989530771432));
#31932=CARTESIAN_POINT('Ctrl Pts',(-80.8296869809109,5.96579849563975,-3.71593320823578));
#31933=CARTESIAN_POINT('Ctrl Pts',(-80.796657719172,6.50618185236486,-2.65866677163672));
#31934=CARTESIAN_POINT('Ctrl Pts',(-80.7636284574331,6.76119444774047,-1.53654705982131));
#31935=CARTESIAN_POINT('Ctrl Pts',(-80.7305991956942,7.01620704311609,-0.414427348005899));
#31936=CARTESIAN_POINT('Ctrl Pts',(-80.6975699339554,6.98584887714221,0.772545639025848));
#31937=CARTESIAN_POINT('Ctrl Pts',(-80.6645406722164,6.67380827143942,1.8801623289676));
#31938=CARTESIAN_POINT('Ctrl Pts',(-80.6315114104775,6.36176766573663,2.98777901890934));
#31939=CARTESIAN_POINT('Ctrl Pts',(-80.5984821487386,5.76804462030492,4.01603941176109));
#31940=CARTESIAN_POINT('Ctrl Pts',(-80.5654528869998,4.96477266083155,4.8400164930981));
#31941=CARTESIAN_POINT('Ctrl Pts',(-80.5324236252609,4.16150070135818,5.66399357443512));
#31942=CARTESIAN_POINT('Ctrl Pts',(-80.499394363522,3.14867982784313,6.28368734425741));
#31943=CARTESIAN_POINT('Ctrl Pts',(-80.4663651017831,2.04936125256192,6.6238090011488));
#31944=CARTESIAN_POINT('Ctrl Pts',(-80.4333358400442,0.950042677280704,
6.9639306580402));
#31945=CARTESIAN_POINT('Ctrl Pts',(-80.4003065783053,-0.235773599766704,
7.02448020200071));
#31946=CARTESIAN_POINT('Ctrl Pts',(-80.3672773165664,-1.36401853908634,
6.79810125345532));
#31947=CARTESIAN_POINT('Ctrl Pts',(-80.3342480548275,-2.49226347840598,
6.57172230490993));
#31948=CARTESIAN_POINT('Ctrl Pts',(-80.3012187930887,-3.56293707999787,
6.05841486385864));
#31949=CARTESIAN_POINT('Ctrl Pts',(-80.2681895313498,-4.44595939777042,
5.32054247803539));
#31950=CARTESIAN_POINT('Ctrl Pts',(-80.2351602696109,-5.32898171554296,
4.58267009221216));
#31951=CARTESIAN_POINT('Ctrl Pts',(-80.2021310078719,-6.02435274949617,
3.62023276161698));
#31952=CARTESIAN_POINT('Ctrl Pts',(-80.169101746133,-6.44758939807997,2.55016042259479));
#31953=CARTESIAN_POINT('Ctrl Pts',(-80.1441250519574,-6.76764052181244,
1.74097280681279));
#31954=CARTESIAN_POINT('Ctrl Pts',(-80.1191483577819,-6.93207516122631,
0.870235521082701));
#31955=CARTESIAN_POINT('Ctrl Pts',(-80.0941716636063,-6.93295492521967,
-0.000178757583534305));
#31956=CARTESIAN_POINT('Origin',(-87.75,0.,0.));
#31957=CARTESIAN_POINT('',(-78.6648283363938,-6.93264414159005,0.000146499032823016));
#31958=CARTESIAN_POINT('',(-78.8441716636063,-6.93256537376933,0.000124608584710398));
#31959=CARTESIAN_POINT('',(-87.75,-6.933,-8.4904762584886E-16));
#31960=CARTESIAN_POINT('Ctrl Pts',(-78.6648283363938,-6.93264414159005,
0.000146499032823016));
#31961=CARTESIAN_POINT('Ctrl Pts',(-78.6760580848127,-6.93294570416691,
0.391543037810179));
#31962=CARTESIAN_POINT('Ctrl Pts',(-78.6872878332316,-6.90035368842132,
0.782889892230009));
#31963=CARTESIAN_POINT('Ctrl Pts',(-78.6985175816505,-6.83441674149118,
1.16853549413445));
#31964=CARTESIAN_POINT('Ctrl Pts',(-78.7315468433894,-6.64048108085322,
2.30280752308806));
#31965=CARTESIAN_POINT('Ctrl Pts',(-78.7645761051282,-6.15808415438807,
3.38775899689383));
#31966=CARTESIAN_POINT('Ctrl Pts',(-78.7976053668671,-5.44583408141055,
4.29157529995388));
#31967=CARTESIAN_POINT('Ctrl Pts',(-78.830634628606,-4.73358400843304,5.19539160301392));
#31968=CARTESIAN_POINT('Ctrl Pts',(-78.8636638903449,-3.79148078894316,
5.91807273532824));
#31969=CARTESIAN_POINT('Ctrl Pts',(-78.8966931520838,-2.73398389576414,
6.37181759430771));
#31970=CARTESIAN_POINT('Ctrl Pts',(-78.9297224138227,-1.67648700258512,
6.82556245328718));
#31971=CARTESIAN_POINT('Ctrl Pts',(-78.9627516755616,-0.50359643571695,
7.0103710389318));
#31972=CARTESIAN_POINT('Ctrl Pts',(-78.9957809373005,0.642189155875181,
6.90379029848845));
#31973=CARTESIAN_POINT('Ctrl Pts',(-79.0288101990394,1.78797474746733,6.7972095580451));
#31974=CARTESIAN_POINT('Ctrl Pts',(-79.0618394607782,2.90665536378344,6.39923949151378));
#31975=CARTESIAN_POINT('Ctrl Pts',(-79.0948687225171,3.86231851566927,5.75823089854386));
#31976=CARTESIAN_POINT('Ctrl Pts',(-79.127897984256,4.81798166755509,5.11722230557395));
#31977=CARTESIAN_POINT('Ctrl Pts',(-79.1609272459949,5.61062735501063,4.23317518616545));
#31978=CARTESIAN_POINT('Ctrl Pts',(-79.1939565077338,6.14395423265796,3.21349557093693));
#31979=CARTESIAN_POINT('Ctrl Pts',(-79.2269857694727,6.67728111030527,2.19381595570843));
#31980=CARTESIAN_POINT('Ctrl Pts',(-79.2600150312116,6.95128917814437,1.03850384465991));
#31981=CARTESIAN_POINT('Ctrl Pts',(-79.2930442929505,6.93268822089381,-0.112077782397874));
#31982=CARTESIAN_POINT('Ctrl Pts',(-79.3260735546894,6.91408726364324,-1.26265940945566));
#31983=CARTESIAN_POINT('Ctrl Pts',(-79.3591028164283,6.60287728130299,-2.40851055252272));
#31984=CARTESIAN_POINT('Ctrl Pts',(-79.3921320781672,6.03686828213871,-3.41041767845737));
#31985=CARTESIAN_POINT('Ctrl Pts',(-79.425161339906,5.47085928297442,-4.41232480439202));
#31986=CARTESIAN_POINT('Ctrl Pts',(-79.4581906016449,4.6500512669861,-5.27028791319426));
#31987=CARTESIAN_POINT('Ctrl Pts',(-79.4912198633838,3.67416712106713,-5.88007001351993));
#31988=CARTESIAN_POINT('Ctrl Pts',(-79.5242491251227,2.69828297514816,-6.48985211384559));
#31989=CARTESIAN_POINT('Ctrl Pts',(-79.5572783868616,1.56732269929855,-6.85145320569469));
#31990=CARTESIAN_POINT('Ctrl Pts',(-79.5903076486005,0.4186906822092,-6.92094108557919));
#31991=CARTESIAN_POINT('Ctrl Pts',(-79.6233369103394,-0.729941334880146,
-6.9904289654637));
#31992=CARTESIAN_POINT('Ctrl Pts',(-79.6563661720783,-1.89624509320922,
-6.76780363338362));
#31993=CARTESIAN_POINT('Ctrl Pts',(-79.6893954338172,-2.93852219862291,
-6.28011263319595));
#31994=CARTESIAN_POINT('Ctrl Pts',(-79.7224246955561,-3.98079930403662,
-5.79242163300826));
#31995=CARTESIAN_POINT('Ctrl Pts',(-79.755453957295,-4.89904975653494,-5.03966496471298));
#31996=CARTESIAN_POINT('Ctrl Pts',(-79.7884832190338,-5.58171204084191,
-4.11329771479616));
#31997=CARTESIAN_POINT('Ctrl Pts',(-79.8215124807727,-6.26437432514887,
-3.18693046487936));
#31998=CARTESIAN_POINT('Ctrl Pts',(-79.8545417425116,-6.71144844126449,
-2.08695263334102));
#31999=CARTESIAN_POINT('Ctrl Pts',(-79.8875710042505,-6.86861776380751,
-0.947004441454659));
#32000=CARTESIAN_POINT('Ctrl Pts',(-79.8966567816316,-6.91185232009428,
-0.63342445352396));
#32001=CARTESIAN_POINT('Ctrl Pts',(-79.9057425590127,-6.93314964345906,
-0.316819889510455));
#32002=CARTESIAN_POINT('Ctrl Pts',(-79.9148283363937,-6.93284541734693,
-0.000174722887704981));
#32003=CARTESIAN_POINT('Ctrl Pts',(-80.0941716636063,-6.93295492521967,
-0.000178757583534305));
#32004=CARTESIAN_POINT('Ctrl Pts',(-80.086119096043,-6.93323856399694,-0.280803156382215));
#32005=CARTESIAN_POINT('Ctrl Pts',(-80.0780665284797,-6.9165216776303,-0.561393980579732));
#32006=CARTESIAN_POINT('Ctrl Pts',(-80.0700139609165,-6.88253823603364,
-0.839877762973264));
#32007=CARTESIAN_POINT('Ctrl Pts',(-80.0369846991776,-6.74314816218912,
-1.98213626206991));
#32008=CARTESIAN_POINT('Ctrl Pts',(-80.0039554374386,-6.31326575128568,
-3.08894591281398));
#32009=CARTESIAN_POINT('Ctrl Pts',(-79.9709261756997,-5.64511894725778,
-4.0258364719041));
#32010=CARTESIAN_POINT('Ctrl Pts',(-79.9378969139608,-4.97697214322988,
-4.96272703099423));
#32011=CARTESIAN_POINT('Ctrl Pts',(-79.904867652222,-4.07056094607752,-5.72969849843039));
#32012=CARTESIAN_POINT('Ctrl Pts',(-79.8718383904831,-3.03600847781199,
-6.23356878119234));
#32013=CARTESIAN_POINT('Ctrl Pts',(-79.8388091287442,-2.00145600954648,
-6.73743906395428));
#32014=CARTESIAN_POINT('Ctrl Pts',(-79.8057798670053,-0.838762270167813,
-6.97820816204202));
#32015=CARTESIAN_POINT('Ctrl Pts',(-79.7727506052664,0.310812940218244,
-6.92662418089757));
#32016=CARTESIAN_POINT('Ctrl Pts',(-79.7397213435275,1.46038815060428,-6.87504019975313));
#32017=CARTESIAN_POINT('Ctrl Pts',(-79.7066920817886,2.59684483199772,-6.5311031393765));
#32018=CARTESIAN_POINT('Ctrl Pts',(-79.6736628200497,3.58211081783791,-5.93659913721069));
#32019=CARTESIAN_POINT('Ctrl Pts',(-79.6406335583108,4.56737680367813,-5.34209513504485));
#32020=CARTESIAN_POINT('Ctrl Pts',(-79.6076042965719,5.40145209396511,-4.49702419108981));
#32021=CARTESIAN_POINT('Ctrl Pts',(-79.574575034833,5.98300191343629,-3.50405698170275));
#32022=CARTESIAN_POINT('Ctrl Pts',(-79.5415457730942,6.56455173290748,-2.51108977231567));
#32023=CARTESIAN_POINT('Ctrl Pts',(-79.5085165113553,6.89357608156287,-1.37022629749662));
#32024=CARTESIAN_POINT('Ctrl Pts',(-79.4754872496164,6.93010062037677,-0.220074120822001));
#32025=CARTESIAN_POINT('Ctrl Pts',(-79.4424579878775,6.96662515919067,0.93007805585257));
#32026=CARTESIAN_POINT('Ctrl Pts',(-79.4094287261386,6.71064988816308,2.08951893438267));
#32027=CARTESIAN_POINT('Ctrl Pts',(-79.3763994643997,6.19327415391706,3.11738391630306));
#32028=CARTESIAN_POINT('Ctrl Pts',(-79.3433702026608,5.67589841967103,4.14524889822346));
#32029=CARTESIAN_POINT('Ctrl Pts',(-79.310340940922,4.89712222220651,5.0415379835342));
#32030=CARTESIAN_POINT('Ctrl Pts',(-79.2773116791831,3.95156185320478,5.69735782161336));
#32031=CARTESIAN_POINT('Ctrl Pts',(-79.2442824174442,3.00600148420302,6.35317765969253));
#32032=CARTESIAN_POINT('Ctrl Pts',(-79.2112531557053,1.89365694366406,6.76852825054014));
#32033=CARTESIAN_POINT('Ctrl Pts',(-79.1782238939664,0.749670928347523,
6.89294717275511));
#32034=CARTESIAN_POINT('Ctrl Pts',(-79.1451946322275,-0.394315086968993,
7.01736609497008));
#32035=CARTESIAN_POINT('Ctrl Pts',(-79.1121653704886,-1.56994257706304,
6.8508533485524));
#32036=CARTESIAN_POINT('Ctrl Pts',(-79.0791361087497,-2.63438037442674,
6.41363915963763));
#32037=CARTESIAN_POINT('Ctrl Pts',(-79.0461068470108,-3.69881817179041,
5.97642497072288));
#32038=CARTESIAN_POINT('Ctrl Pts',(-79.0130775852719,-4.65206627642376,
5.26850933931104));
#32039=CARTESIAN_POINT('Ctrl Pts',(-78.980048323533,-5.37831118374589,4.37589945474024));
#32040=CARTESIAN_POINT('Ctrl Pts',(-78.9470190617941,-6.10455609106804,
3.48328957016942));
#32041=CARTESIAN_POINT('Ctrl Pts',(-78.9139898000553,-6.60379780107896,
2.40598543243962));
#32042=CARTESIAN_POINT('Ctrl Pts',(-78.8809605383164,-6.81538166176488,
1.27487255507408));
#32043=CARTESIAN_POINT('Ctrl Pts',(-78.8686975800797,-6.89393758189603,
0.854917967963368));
#32044=CARTESIAN_POINT('Ctrl Pts',(-78.856434621843,-6.93284114622974,0.427546085291084));
#32045=CARTESIAN_POINT('Ctrl Pts',(-78.8441716636063,-6.93256537376933,
0.000124608584710398));
#32046=CARTESIAN_POINT('Origin',(-87.75,0.,0.));
#32047=CARTESIAN_POINT('',(-77.4148283363937,-6.93355988365441,-5.3614765520571E-5));
#32048=CARTESIAN_POINT('',(-77.5941716636063,-6.93359074487482,-1.65665743479807E-5));
#32049=CARTESIAN_POINT('',(-87.75,-6.933,-8.4904762584886E-16));
#32050=CARTESIAN_POINT('Ctrl Pts',(-77.4148283363937,-6.93355988365441,
-5.3614765520571E-5));
#32051=CARTESIAN_POINT('Ctrl Pts',(-77.4463736106126,-6.9331052532896,1.09899237861107));
#32052=CARTESIAN_POINT('Ctrl Pts',(-77.4779188848315,-6.66710498440094,
2.198250639548));
#32053=CARTESIAN_POINT('Ctrl Pts',(-77.5094641590504,-6.16380047409797,
3.17526236914945));
#32054=CARTESIAN_POINT('Ctrl Pts',(-77.5424934207893,-5.63681895890149,
4.19823576018895));
#32055=CARTESIAN_POINT('Ctrl Pts',(-77.5755226825282,-4.8496809805689,5.08719036996541));
#32056=CARTESIAN_POINT('Ctrl Pts',(-77.6085519442671,-3.89801873329636,
5.73412393939105));
#32057=CARTESIAN_POINT('Ctrl Pts',(-77.641581206006,-2.94635648602384,6.38105750881668));
#32058=CARTESIAN_POINT('Ctrl Pts',(-77.6746104677449,-1.83016996981136,
6.7859700378915));
#32059=CARTESIAN_POINT('Ctrl Pts',(-77.7076397294838,-0.685068656715781,
6.89966726248539));
#32060=CARTESIAN_POINT('Ctrl Pts',(-77.7406689912226,0.460032656379802,
7.01336448707927));
#32061=CARTESIAN_POINT('Ctrl Pts',(-77.7736982529615,1.6340487663585,6.83584640719222));
#32062=CARTESIAN_POINT('Ctrl Pts',(-77.8067275147004,2.69434427801713,6.38868032608795));
#32063=CARTESIAN_POINT('Ctrl Pts',(-77.8397567764393,3.75463978967577,5.94151424498368));
#32064=CARTESIAN_POINT('Ctrl Pts',(-77.8727860381782,4.70121470301435,5.22470016266219));
#32065=CARTESIAN_POINT('Ctrl Pts',(-77.9058152999171,5.41906626321042,4.32532637292975));
#32066=CARTESIAN_POINT('Ctrl Pts',(-77.938844561656,6.13691782340649,3.42595258319731));
#32067=CARTESIAN_POINT('Ctrl Pts',(-77.9718738233948,6.62604603046005,2.34401908605393));
#32068=CARTESIAN_POINT('Ctrl Pts',(-78.0049030851337,6.82702495782282,1.21097383237262));
#32069=CARTESIAN_POINT('Ctrl Pts',(-78.0379323468726,7.02800388518558,0.0779285786913365));
#32070=CARTESIAN_POINT('Ctrl Pts',(-78.0709616086116,6.94083353285755,-1.10622843152787));
#32071=CARTESIAN_POINT('Ctrl Pts',(-78.1039908703505,6.57610453715848,-2.19762974902292));
#32072=CARTESIAN_POINT('Ctrl Pts',(-78.1370201320894,6.21137554145941,-3.28903106651797));
#32073=CARTESIAN_POINT('Ctrl Pts',(-78.1700493938282,5.56908790238929,-4.28767669128886));
#32074=CARTESIAN_POINT('Ctrl Pts',(-78.2030786555671,4.7272754309446,-5.07223761247583));
#32075=CARTESIAN_POINT('Ctrl Pts',(-78.236107917306,3.88546295949989,-5.85679853366282));
#32076=CARTESIAN_POINT('Ctrl Pts',(-78.2691371790449,2.8441256556806,-6.42727475126589));
#32077=CARTESIAN_POINT('Ctrl Pts',(-78.3021664407838,1.72977929436205,-6.71435707943979));
#32078=CARTESIAN_POINT('Ctrl Pts',(-78.3351957025227,0.615432933043514,
-7.00143940761369));
#32079=CARTESIAN_POINT('Ctrl Pts',(-78.3682249642616,-0.571922485774274,
-7.00512784635843));
#32080=CARTESIAN_POINT('Ctrl Pts',(-78.4012542260005,-1.68803092678632,
-6.72497427412476));
#32081=CARTESIAN_POINT('Ctrl Pts',(-78.4342834877393,-2.80413936779834,
-6.44482070189109));
#32082=CARTESIAN_POINT('Ctrl Pts',(-78.4673127494782,-3.84900083100463,
-5.88082511867903));
#32083=CARTESIAN_POINT('Ctrl Pts',(-78.5003420112171,-4.69567137886439,
-5.10150935499884));
#32084=CARTESIAN_POINT('Ctrl Pts',(-78.533371272956,-5.54234192672416,-4.32219359131866));
#32085=CARTESIAN_POINT('Ctrl Pts',(-78.5664005346949,-6.1908215592374,-3.32755764717036));
#32086=CARTESIAN_POINT('Ctrl Pts',(-78.5994297964338,-6.56232417808864,
-2.23844338304549));
#32087=CARTESIAN_POINT('Ctrl Pts',(-78.6212293097538,-6.80751816250399,
-1.51962135500671));
#32088=CARTESIAN_POINT('Ctrl Pts',(-78.6430288230738,-6.93205873956981,
-0.759643813464775));
#32089=CARTESIAN_POINT('Ctrl Pts',(-78.6648283363938,-6.93264414159005,
0.000146499032823016));
#32090=CARTESIAN_POINT('Ctrl Pts',(-78.8441716636063,-6.93256537376933,
0.000124608584710398));
#32091=CARTESIAN_POINT('Ctrl Pts',(-78.8234053601041,-6.9320983759618,-0.723678240394669));
#32092=CARTESIAN_POINT('Ctrl Pts',(-78.8026390566018,-6.81927829988588,
-1.44762330827946));
#32093=CARTESIAN_POINT('Ctrl Pts',(-78.7818727530997,-6.59640219545387,
-2.13593195186867));
#32094=CARTESIAN_POINT('Ctrl Pts',(-78.7488434913608,-6.24191285709603,
-3.23070196444461));
#32095=CARTESIAN_POINT('Ctrl Pts',(-78.715814229622,-5.60900816901946,-4.23532037259521));
#32096=CARTESIAN_POINT('Ctrl Pts',(-78.6827849678831,-4.77458197411304,
-5.02773251075243));
#32097=CARTESIAN_POINT('Ctrl Pts',(-78.6497557061442,-3.94015577920663,
-5.82014464890964));
#32098=CARTESIAN_POINT('Ctrl Pts',(-78.6167264444052,-2.9042080774704,-6.40035051707347));
#32099=CARTESIAN_POINT('Ctrl Pts',(-78.5836971826663,-1.79259984184248,
-6.69785883952688));
#32100=CARTESIAN_POINT('Ctrl Pts',(-78.5506679209274,-0.680991606214557,
-6.9953671619803));
#32101=CARTESIAN_POINT('Ctrl Pts',(-78.5176386591886,0.506277163305044,
-7.01017793872329));
#32102=CARTESIAN_POINT('Ctrl Pts',(-78.4846093974497,1.62496095874294,-6.74049175578187));
#32103=CARTESIAN_POINT('Ctrl Pts',(-78.4515801357108,2.74364475418086,-6.47080557284044));
#32104=CARTESIAN_POINT('Ctrl Pts',(-78.4185508739719,3.79374357553707,-5.91662243021457));
#32105=CARTESIAN_POINT('Ctrl Pts',(-78.385521612233,4.64767717999083,-5.14527201008796));
#32106=CARTESIAN_POINT('Ctrl Pts',(-78.3524923504941,5.50161078444459,-4.37392158996134));
#32107=CARTESIAN_POINT('Ctrl Pts',(-78.3194630887553,6.15937917199591,-3.38540389233398));
#32108=CARTESIAN_POINT('Ctrl Pts',(-78.2864338270164,6.54106772042358,-2.29981745015442));
#32109=CARTESIAN_POINT('Ctrl Pts',(-78.2534045652775,6.92275626885124,-1.21423100797489));
#32110=CARTESIAN_POINT('Ctrl Pts',(-78.2203753035385,7.02836497815528,-0.0315758212431301));
#32111=CARTESIAN_POINT('Ctrl Pts',(-78.1873460417997,6.84506307040986,1.10446312265876));
#32112=CARTESIAN_POINT('Ctrl Pts',(-78.1543167800608,6.66176116266444,2.24050206656066));
#32113=CARTESIAN_POINT('Ctrl Pts',(-78.1212875183219,6.18954863786957,3.32992476763274));
#32114=CARTESIAN_POINT('Ctrl Pts',(-78.088258256583,5.48579627613764,4.24037338496465));
#32115=CARTESIAN_POINT('Ctrl Pts',(-78.0552289948441,4.78204391440569,5.15082200229657));
#32116=CARTESIAN_POINT('Ctrl Pts',(-78.0221997331052,3.84675171573669,5.88229653588832));
#32117=CARTESIAN_POINT('Ctrl Pts',(-77.9891704713663,2.79355165779576,6.34592754153627));
#32118=CARTESIAN_POINT('Ctrl Pts',(-77.9561412096274,1.74035159985484,6.80955854718422));
#32119=CARTESIAN_POINT('Ctrl Pts',(-77.9231119478886,0.56924368264199,7.00534602488837));
#32120=CARTESIAN_POINT('Ctrl Pts',(-77.8900826861497,-0.577490025328187,
6.9095030572284));
#32121=CARTESIAN_POINT('Ctrl Pts',(-77.8570534244108,-1.72422373329835,
6.81366008956843));
#32122=CARTESIAN_POINT('Ctrl Pts',(-77.8240241626719,-2.84658323202583,
6.42618667654436));
#32123=CARTESIAN_POINT('Ctrl Pts',(-77.790994900933,-3.80820907184011,5.79415834201627));
#32124=CARTESIAN_POINT('Ctrl Pts',(-77.7579656391941,-4.76983491165438,
5.16213000748818));
#32125=CARTESIAN_POINT('Ctrl Pts',(-77.7249363774552,-5.57072709255544,
4.28554675145607));
#32126=CARTESIAN_POINT('Ctrl Pts',(-77.6919071157163,-6.11358237332966,
3.27090779321506));
#32127=CARTESIAN_POINT('Ctrl Pts',(-77.6593286316797,-6.64902885829029,
2.27011645354264));
#32128=CARTESIAN_POINT('Ctrl Pts',(-77.626750147643,-6.93343366709735,1.13501201807639));
#32129=CARTESIAN_POINT('Ctrl Pts',(-77.5941716636063,-6.93359074487482,
-1.65665743479807E-5));
#32130=CARTESIAN_POINT('Origin',(-87.75,0.,0.));
#32131=CARTESIAN_POINT('',(-76.1648283363937,-6.93245908794419,-7.27747633805231E-5));
#32132=CARTESIAN_POINT('',(-76.3441716636063,-6.93250871142555,-0.000101958036885148));
#32133=CARTESIAN_POINT('',(-87.75,-6.933,-8.4904762584886E-16));
#32134=CARTESIAN_POINT('Ctrl Pts',(-76.1648283363937,-6.93245908794419,
-7.27747633805231E-5));
#32135=CARTESIAN_POINT('Ctrl Pts',(-76.1836598746737,-6.93221658934376,
0.656323270318536));
#32136=CARTESIAN_POINT('Ctrl Pts',(-76.2024914129537,-6.83971996360292,
1.31278624755817));
#32137=CARTESIAN_POINT('Ctrl Pts',(-76.2213229512337,-6.65590312778372,
1.94259644573592));
#32138=CARTESIAN_POINT('Ctrl Pts',(-76.2543522129726,-6.33350066166455,
3.04724151360787));
#32139=CARTESIAN_POINT('Ctrl Pts',(-76.2873814747115,-5.73017148093525,
4.06989511813717));
#32140=CARTESIAN_POINT('Ctrl Pts',(-76.3204107364504,-4.91921619484598,
4.8863114335654));
#32141=CARTESIAN_POINT('Ctrl Pts',(-76.3534399981892,-4.10826090875669,
5.70272774899365));
#32142=CARTESIAN_POINT('Ctrl Pts',(-76.3864692599281,-3.0896795173074,6.31290677532083));
#32143=CARTESIAN_POINT('Ctrl Pts',(-76.4194985216671,-1.98722309859757,
6.64271569117836));
#32144=CARTESIAN_POINT('Ctrl Pts',(-76.4525277834059,-0.884766679887746,
6.97252460703589));
#32145=CARTESIAN_POINT('Ctrl Pts',(-76.4855570451448,0.301564766082627,
7.02196341242377));
#32146=CARTESIAN_POINT('Ctrl Pts',(-76.5185863068837,1.42763961011382,6.78502561093626));
#32147=CARTESIAN_POINT('Ctrl Pts',(-76.5516155686226,2.55371445414502,6.54808780944875));
#32148=CARTESIAN_POINT('Ctrl Pts',(-76.5846448303615,3.61953269623705,6.02477340108585));
#32149=CARTESIAN_POINT('Ctrl Pts',(-76.6176740921004,4.49560428520284,5.27866171565225));
#32150=CARTESIAN_POINT('Ctrl Pts',(-76.6507033538393,5.37167587416864,4.53255003021866));
#32151=CARTESIAN_POINT('Ctrl Pts',(-76.6837326155782,6.05800081000821,3.56364106771436));
#32152=CARTESIAN_POINT('Ctrl Pts',(-76.7167618773171,6.47119503382389,2.48965102607572));
#32153=CARTESIAN_POINT('Ctrl Pts',(-76.7497911390559,6.88438925763956,1.41566098443711));
#32154=CARTESIAN_POINT('Ctrl Pts',(-76.7828204007948,7.02445276943136,0.236589863664146));
#32155=CARTESIAN_POINT('Ctrl Pts',(-76.8158496625337,6.874368754704,-0.904312789789189));
#32156=CARTESIAN_POINT('Ctrl Pts',(-76.8488789242726,6.72428473997664,-2.04521544324256));
#32157=CARTESIAN_POINT('Ctrl Pts',(-76.8819081860115,6.28405319873012,-3.1479496293763));
#32158=CARTESIAN_POINT('Ctrl Pts',(-76.9149374477504,5.60715942757398,-4.078540247588));
#32159=CARTESIAN_POINT('Ctrl Pts',(-76.9479667094893,4.93026565641784,-5.00913086579971));
#32160=CARTESIAN_POINT('Ctrl Pts',(-76.9809959712282,4.01670965535209,-5.76757791608937));
#32161=CARTESIAN_POINT('Ctrl Pts',(-77.014025232967,2.97748259404187,-6.26173496721194));
#32162=CARTESIAN_POINT('Ctrl Pts',(-77.0470544947059,1.93825553273165,-6.7558920183345));
#32163=CARTESIAN_POINT('Ctrl Pts',(-77.0800837564448,0.773357411176957,
-6.98575907028995));
#32164=CARTESIAN_POINT('Ctrl Pts',(-77.1131130181837,-0.375684152281078,
-6.92340875690233));
#32165=CARTESIAN_POINT('Ctrl Pts',(-77.1461422799226,-1.5247257157391,-6.8610584435147));
#32166=CARTESIAN_POINT('Ctrl Pts',(-77.1791715416615,-2.65791072110042,
-6.50649076478404));
#32167=CARTESIAN_POINT('Ctrl Pts',(-77.2122008034004,-3.63756448936863,
-5.90278340980857));
#32168=CARTESIAN_POINT('Ctrl Pts',(-77.2452300651393,-4.61721825763681,
-5.29907605483312));
#32169=CARTESIAN_POINT('Ctrl Pts',(-77.2782593268782,-5.44334078881188,
-4.44622902361285));
#32170=CARTESIAN_POINT('Ctrl Pts',(-77.3112885886171,-6.01556351663744,
-3.44785773701984));
#32171=CARTESIAN_POINT('Ctrl Pts',(-77.344317850356,-6.58778624446302,-2.44948645042679));
#32172=CARTESIAN_POINT('Ctrl Pts',(-77.3773471120949,-6.9061091689391,-1.30559090846094));
#32173=CARTESIAN_POINT('Ctrl Pts',(-77.4103763738337,-6.93185810514696,
-0.155147051326755));
#32174=CARTESIAN_POINT('Ctrl Pts',(-77.4118603613537,-6.93301499143427,
-0.103458208265699));
#32175=CARTESIAN_POINT('Ctrl Pts',(-77.4133443488737,-6.93358127087656,
-0.0517561463953276));
#32176=CARTESIAN_POINT('Ctrl Pts',(-77.4148283363937,-6.93355988365441,
-5.3614765520571E-5));
#32177=CARTESIAN_POINT('Ctrl Pts',(-77.5941716636063,-6.93359074487482,
-1.65665743479807E-5));
#32178=CARTESIAN_POINT('Ctrl Pts',(-77.5937208859041,-6.93359291830805,
-0.0157215814777106));
#32179=CARTESIAN_POINT('Ctrl Pts',(-77.5932701082019,-6.93354067154366,
-0.0314265818591758));
#32180=CARTESIAN_POINT('Ctrl Pts',(-77.5928193304997,-6.93343391661625,
-0.047131211712011));
#32181=CARTESIAN_POINT('Ctrl Pts',(-77.5597900687608,-6.92561179848128,
-1.19783659794813));
#32182=CARTESIAN_POINT('Ctrl Pts',(-77.5267608070219,-6.62514918156395,
-2.34655270997042));
#32183=CARTESIAN_POINT('Ctrl Pts',(-77.493731545283,-6.06855033845775,-3.35371793936318));
#32184=CARTESIAN_POINT('Ctrl Pts',(-77.4607022835441,-5.51195149535157,
-4.3608831687559));
#32185=CARTESIAN_POINT('Ctrl Pts',(-77.4276730218052,-4.69921642605653,
-5.2264975155191));
#32186=CARTESIAN_POINT('Ctrl Pts',(-77.3946437600663,-3.72908720644287,
-5.84539441218008));
#32187=CARTESIAN_POINT('Ctrl Pts',(-77.3616144983274,-2.75895798682919,
-6.46429130884108));
#32188=CARTESIAN_POINT('Ctrl Pts',(-77.3285852365886,-1.63143461689687,
-6.83647075539986));
#32189=CARTESIAN_POINT('Ctrl Pts',(-77.2955559748497,-0.483503923405929,
-6.91671534640924));
#32190=CARTESIAN_POINT('Ctrl Pts',(-77.2625267131108,0.664426770085027,
-6.99695993741863));
#32191=CARTESIAN_POINT('Ctrl Pts',(-77.2294974513719,1.83276478713461,-6.78526967287862));
#32192=CARTESIAN_POINT('Ctrl Pts',(-77.196468189633,2.87956458425637,-6.30736355637587));
#32193=CARTESIAN_POINT('Ctrl Pts',(-77.1634389278941,3.92636438137815,-5.82945743987311));
#32194=CARTESIAN_POINT('Ctrl Pts',(-77.1304096661552,4.85162595857206,-5.08533547140764));
#32195=CARTESIAN_POINT('Ctrl Pts',(-77.0973804044163,5.54293599407229,-4.1654036770546));
#32196=CARTESIAN_POINT('Ctrl Pts',(-77.0643511426775,6.23424602957248,-3.24547188270159));
#32197=CARTESIAN_POINT('Ctrl Pts',(-77.0313218809385,6.69160452337899,-2.14973026246101));
#32198=CARTESIAN_POINT('Ctrl Pts',(-76.9982926191996,6.85944536446558,-1.01130436522037));
#32199=CARTESIAN_POINT('Ctrl Pts',(-76.9652633574607,7.02728620555217,0.127121532020305));
#32200=CARTESIAN_POINT('Ctrl Pts',(-76.9322340957219,6.90560939391885,1.30823170626106));
#32201=CARTESIAN_POINT('Ctrl Pts',(-76.899204833983,6.5091978784254,2.38852887918575));
#32202=CARTESIAN_POINT('Ctrl Pts',(-76.8661755722441,6.11278636293196,3.46882605211044));
#32203=CARTESIAN_POINT('Ctrl Pts',(-76.8331463105052,5.44164014357837,4.44831022371903));
#32204=CARTESIAN_POINT('Ctrl Pts',(-76.8001170487663,4.57729916297956,5.20798037628682));
#32205=CARTESIAN_POINT('Ctrl Pts',(-76.7670877870274,3.71295818238075,5.96765052885462));
#32206=CARTESIAN_POINT('Ctrl Pts',(-76.7340585252885,2.65542244053669,6.50750666238162));
#32207=CARTESIAN_POINT('Ctrl Pts',(-76.7010292635496,1.53317571820417,6.76195973400546));
#32208=CARTESIAN_POINT('Ctrl Pts',(-76.6680000018108,0.410928995871668,
7.0164128056293));
#32209=CARTESIAN_POINT('Ctrl Pts',(-76.6349707400718,-0.77602870694931,
6.98546281535));
#32210=CARTESIAN_POINT('Ctrl Pts',(-76.601941478333,-1.88348967488557,6.67286998762912));
#32211=CARTESIAN_POINT('Ctrl Pts',(-76.5689122165941,-2.99095064282184,
6.36027715990825));
#32212=CARTESIAN_POINT('Ctrl Pts',(-76.5358829548552,-4.0189148758734,5.76604149474581));
#32213=CARTESIAN_POINT('Ctrl Pts',(-76.5028536931163,-4.84249134112358,
4.9623587978244));
#32214=CARTESIAN_POINT('Ctrl Pts',(-76.4698244313774,-5.66606780637378,
4.15867610090298));
#32215=CARTESIAN_POINT('Ctrl Pts',(-76.4367951696385,-6.2852565038226,3.14554637222259));
#32216=CARTESIAN_POINT('Ctrl Pts',(-76.4037659078996,-6.62482999509395,
2.0460583479719));
#32217=CARTESIAN_POINT('Ctrl Pts',(-76.3839011598018,-6.82905926058937,
1.3847946233713));
#32218=CARTESIAN_POINT('Ctrl Pts',(-76.364036411704,-6.93214707574568,0.692293673219922));
#32219=CARTESIAN_POINT('Ctrl Pts',(-76.3441716636063,-6.93250871142555,
-0.000101958036885148));
#32220=CARTESIAN_POINT('Origin',(-87.75,0.,0.));
#32221=CARTESIAN_POINT('',(-74.9148283363937,-6.93316696520231,0.00016807782604461));
#32222=CARTESIAN_POINT('',(-75.0941716636063,-6.93305363032429,0.000176774812155918));
#32223=CARTESIAN_POINT('',(-87.75,-6.933,-8.4904762584886E-16));
#32224=CARTESIAN_POINT('Ctrl Pts',(-74.9148283363937,-6.93316696520231,
0.00016807782604461));
#32225=CARTESIAN_POINT('Ctrl Pts',(-74.9209461387348,-6.93338316350285,
0.213348952983918));
#32226=CARTESIAN_POINT('Ctrl Pts',(-74.9270639410759,-6.92374509836824,
0.426510353887417));
#32227=CARTESIAN_POINT('Ctrl Pts',(-74.933181743417,-6.90410963765511,0.63874682673552));
#32228=CARTESIAN_POINT('Ctrl Pts',(-74.9662110051559,-6.7981002023875,1.78458541736159));
#32229=CARTESIAN_POINT('Ctrl Pts',(-74.9992402668948,-6.40068796263517,
2.90346432362064));
#32230=CARTESIAN_POINT('Ctrl Pts',(-75.0322695286337,-5.76015594568697,
3.8594469654076));
#32231=CARTESIAN_POINT('Ctrl Pts',(-75.0652987903726,-5.11962392873879,
4.81542960719453));
#32232=CARTESIAN_POINT('Ctrl Pts',(-75.0983280521114,-4.23597213459477,
5.60851598450938));
#32233=CARTESIAN_POINT('Ctrl Pts',(-75.1313573138503,-3.21655856440023,
6.1423512109949));
#32234=CARTESIAN_POINT('Ctrl Pts',(-75.1643865755892,-2.19714499420567,
6.67618643748043));
#32235=CARTESIAN_POINT('Ctrl Pts',(-75.1974158373281,-1.04196964796058,
6.95077051313662));
#32236=CARTESIAN_POINT('Ctrl Pts',(-75.230445099067,0.108621110566956,6.93274324144246));
#32237=CARTESIAN_POINT('Ctrl Pts',(-75.2634743608059,1.25921186909442,6.9147159697483));
#32238=CARTESIAN_POINT('Ctrl Pts',(-75.2965036225447,2.40521803990433,6.60407735070382));
#32239=CARTESIAN_POINT('Ctrl Pts',(-75.3295328842836,3.40740725498283,6.03856797561452));
#32240=CARTESIAN_POINT('Ctrl Pts',(-75.3625621460225,4.40959647006133,5.47305860052522));
#32241=CARTESIAN_POINT('Ctrl Pts',(-75.3955914077615,5.26796872940841,4.65267846939111));
#32242=CARTESIAN_POINT('Ctrl Pts',(-75.4286206695004,5.87823733252418,3.6770984838519));
#32243=CARTESIAN_POINT('Ctrl Pts',(-75.4616499312393,6.48850593563994,2.7015184983127));
#32244=CARTESIAN_POINT('Ctrl Pts',(-75.4946791929781,6.85067088252439,1.57073865836841));
#32245=CARTESIAN_POINT('Ctrl Pts',(-75.527708454717,6.92073146493465,0.422141430909675));
#32246=CARTESIAN_POINT('Ctrl Pts',(-75.5607377164559,6.9907920473449,-0.726455796549087));
#32247=CARTESIAN_POINT('Ctrl Pts',(-75.5937669781948,6.76874826528096,-1.89287041152229));
#32248=CARTESIAN_POINT('Ctrl Pts',(-75.6267962399337,6.28157700801878,-2.9353905514866));
#32249=CARTESIAN_POINT('Ctrl Pts',(-75.6598255016726,5.7944057507566,-3.97791069145091));
#32250=CARTESIAN_POINT('Ctrl Pts',(-75.6928547634115,5.04210701829618,-4.89653635640633));
#32251=CARTESIAN_POINT('Ctrl Pts',(-75.7258840251504,4.11608026086934,-5.57966044518022));
#32252=CARTESIAN_POINT('Ctrl Pts',(-75.7589132868893,3.1900535034425,-6.2627845339541));
#32253=CARTESIAN_POINT('Ctrl Pts',(-75.7919425486281,2.09029872104924,-6.71040704654646));
#32254=CARTESIAN_POINT('Ctrl Pts',(-75.824971810367,0.950429035928664,-6.86814473093649));
#32255=CARTESIAN_POINT('Ctrl Pts',(-75.8580010721059,-0.189440649191916,
-7.02588241532651));
#32256=CARTESIAN_POINT('Ctrl Pts',(-75.8910303338448,-1.36942523703982,
-6.8937352715142));
#32257=CARTESIAN_POINT('Ctrl Pts',(-75.9240595955837,-2.44616420079535,
-6.48775832627682));
#32258=CARTESIAN_POINT('Ctrl Pts',(-75.9570888573226,-3.52290316455086,
-6.08178138103944));
#32259=CARTESIAN_POINT('Ctrl Pts',(-75.9901181190614,-4.496396504214,-5.40197463437701));
#32260=CARTESIAN_POINT('Ctrl Pts',(-76.0231473808003,-5.24837104955287,
-4.5309302271876));
#32261=CARTESIAN_POINT('Ctrl Pts',(-76.0561766425392,-6.00034559489176,
-3.65988581999817));
#32262=CARTESIAN_POINT('Ctrl Pts',(-76.0892059042781,-6.53080134590636,
-2.59760375228175));
#32263=CARTESIAN_POINT('Ctrl Pts',(-76.122235166017,-6.77529134565915,-1.47314445281622));
#32264=CARTESIAN_POINT('Ctrl Pts',(-76.1364328894759,-6.88038607748807,
-0.989792378500842));
#32265=CARTESIAN_POINT('Ctrl Pts',(-76.1506306129348,-6.93264191570988,
-0.494951599266496));
#32266=CARTESIAN_POINT('Ctrl Pts',(-76.1648283363937,-6.93245908794419,
-7.27747633805231E-5));
#32267=CARTESIAN_POINT('Ctrl Pts',(-76.3441716636063,-6.93250871142555,
-0.000101958036885148));
#32268=CARTESIAN_POINT('Ctrl Pts',(-76.3310071499652,-6.93274837003171,
-0.458957599591355));
#32269=CARTESIAN_POINT('Ctrl Pts',(-76.3178426363241,-6.88787264551702,
-0.917766987091575));
#32270=CARTESIAN_POINT('Ctrl Pts',(-76.304678122683,-6.79742030494444,-1.3674079219937));
#32271=CARTESIAN_POINT('Ctrl Pts',(-76.2716488609441,-6.57047883842969,
-2.49553984788754));
#32272=CARTESIAN_POINT('Ctrl Pts',(-76.2386195992052,-6.05663762030631,
-3.56595737985428));
#32273=CARTESIAN_POINT('Ctrl Pts',(-76.2055903374663,-5.31832504878431,
-4.44861168261239));
#32274=CARTESIAN_POINT('Ctrl Pts',(-76.1725610757274,-4.58001247726231,
-5.33126598537049));
#32275=CARTESIAN_POINT('Ctrl Pts',(-76.1395318139885,-3.61722855234165,
-6.02615705891999));
#32276=CARTESIAN_POINT('Ctrl Pts',(-76.1065025522496,-2.54694531934537,
-6.44886011380824));
#32277=CARTESIAN_POINT('Ctrl Pts',(-76.0734732905107,-1.47666208634905,
-6.8715631686965));
#32278=CARTESIAN_POINT('Ctrl Pts',(-76.0404440287718,-0.298879545277113,
-7.02207820492352));
#32279=CARTESIAN_POINT('Ctrl Pts',(-76.0074147670329,0.843309311550133,
-6.88211861509629));
#32280=CARTESIAN_POINT('Ctrl Pts',(-75.974385505294,1.98549816837733,-6.74215902526907));
#32281=CARTESIAN_POINT('Ctrl Pts',(-75.9413562435551,3.09209334095979,-6.31172480938761));
#32282=CARTESIAN_POINT('Ctrl Pts',(-75.9083269818163,4.02865064371125,-5.64311095213686));
#32283=CARTESIAN_POINT('Ctrl Pts',(-75.8752977200774,4.96520794646275,-4.97449709488609));
#32284=CARTESIAN_POINT('Ctrl Pts',(-75.8422684583385,5.73172737938323,-4.06770359626603));
#32285=CARTESIAN_POINT('Ctrl Pts',(-75.8092391965996,6.23508176873444,-3.03290002545378));
#32286=CARTESIAN_POINT('Ctrl Pts',(-75.7762099348607,6.73843615808564,-1.99809645464153));
#32287=CARTESIAN_POINT('Ctrl Pts',(-75.7431806731218,6.97862550386755,-0.835282811637106));
#32288=CARTESIAN_POINT('Ctrl Pts',(-75.7101514113829,6.92646834769301,0.314266535935534));
#32289=CARTESIAN_POINT('Ctrl Pts',(-75.677122149644,6.87431119151848,1.46381588350816));
#32290=CARTESIAN_POINT('Ctrl Pts',(-75.6440928879051,6.52980753338749,2.60010093564904));
#32291=CARTESIAN_POINT('Ctrl Pts',(-75.6110636261663,5.93481234872058,3.58507037764613));
#32292=CARTESIAN_POINT('Ctrl Pts',(-75.5780343644274,5.33981716405367,4.57003981964324));
#32293=CARTESIAN_POINT('Ctrl Pts',(-75.5450051026885,4.49433045285084,5.40369365149659));
#32294=CARTESIAN_POINT('Ctrl Pts',(-75.5119758409496,3.5010734045118,5.98474830242862));
#32295=CARTESIAN_POINT('Ctrl Pts',(-75.4789465792107,2.5078163561728,6.56580295336062));
#32296=CARTESIAN_POINT('Ctrl Pts',(-75.4459173174718,1.36678897069762,6.89425842337131));
#32297=CARTESIAN_POINT('Ctrl Pts',(-75.4128880557329,0.216618725751648,
6.930209488526));
#32298=CARTESIAN_POINT('Ctrl Pts',(-75.379858793994,-0.93355151919432,6.96616055368069));
#32299=CARTESIAN_POINT('Ctrl Pts',(-75.3468295322551,-2.09286462361106,
6.70960721397939));
#32300=CARTESIAN_POINT('Ctrl Pts',(-75.3138002705162,-3.1204715127651,6.19171904766548));
#32301=CARTESIAN_POINT('Ctrl Pts',(-75.2807710087774,-4.14807840191918,
5.67383088135156));
#32302=CARTESIAN_POINT('Ctrl Pts',(-75.2477417470385,-5.04397907581053,
4.89460788842503));
#32303=CARTESIAN_POINT('Ctrl Pts',(-75.2147124852996,-5.69932737330293,
3.94872064333779));
#32304=CARTESIAN_POINT('Ctrl Pts',(-75.1816832235607,-6.35467567079534,
3.00283339825053));
#32305=CARTESIAN_POINT('Ctrl Pts',(-75.1486539618218,-6.76947159188878,
1.89028190100257));
#32306=CARTESIAN_POINT('Ctrl Pts',(-75.1156247000829,-6.89332010398449,
0.746233992260691));
#32307=CARTESIAN_POINT('Ctrl Pts',(-75.108473687924,-6.92013397051462,0.498541489460373));
#32308=CARTESIAN_POINT('Ctrl Pts',(-75.1013226757651,-6.93330980226047,
0.249372605904462));
#32309=CARTESIAN_POINT('Ctrl Pts',(-75.0941716636063,-6.93305363032429,
0.000176774812155918));
#32310=CARTESIAN_POINT('Origin',(-87.75,0.,0.));
#32311=CARTESIAN_POINT('',(-73.6648283363937,-6.9331147324061,-0.00017295491683611));
#32312=CARTESIAN_POINT('',(-73.8441716636062,-6.9332265516286,-0.000160595751058418));
#32313=CARTESIAN_POINT('',(-87.75,-6.933,-8.4904762584886E-16));
#32314=CARTESIAN_POINT('Ctrl Pts',(-73.6648283363937,-6.9331147324061,-0.00017295491683611));
#32315=CARTESIAN_POINT('Ctrl Pts',(-73.6912616645348,-6.93217036533797,
0.920942522637482));
#32316=CARTESIAN_POINT('Ctrl Pts',(-73.7176949926758,-6.74746695301234,
1.84242538290147));
#32317=CARTESIAN_POINT('Ctrl Pts',(-73.7441283208169,-6.3900229396157,2.6911585290748));
#32318=CARTESIAN_POINT('Ctrl Pts',(-73.7771575825558,-5.94338558042776,
3.75167686720537));
#32319=CARTESIAN_POINT('Ctrl Pts',(-73.8101868442948,-5.22704355212943,
4.69860906840553));
#32320=CARTESIAN_POINT('Ctrl Pts',(-73.8432161060336,-4.32802779700381,
5.41690896967904));
#32321=CARTESIAN_POINT('Ctrl Pts',(-73.8762453677725,-3.42901204187819,
6.13520887095255));
#32322=CARTESIAN_POINT('Ctrl Pts',(-73.9092746295114,-2.34732255992529,
6.62487647229942));
#32323=CARTESIAN_POINT('Ctrl Pts',(-73.9423038912502,-1.21437765574423,
6.82642031423909));
#32324=CARTESIAN_POINT('Ctrl Pts',(-73.9753331529891,-0.0814327515631799,
7.02796415617876));
#32325=CARTESIAN_POINT('Ctrl Pts',(-74.0083624147281,1.10276757484602,6.94138423871124));
#32326=CARTESIAN_POINT('Ctrl Pts',(-74.041391676467,2.1943506115832,6.57719946412387));
#32327=CARTESIAN_POINT('Ctrl Pts',(-74.0744209382059,3.28593364832035,6.21301468953652));
#32328=CARTESIAN_POINT('Ctrl Pts',(-74.1074501999447,4.28489939538549,5.57122505782934));
#32329=CARTESIAN_POINT('Ctrl Pts',(-74.1404794616836,5.06987994912212,4.729803875312));
#32330=CARTESIAN_POINT('Ctrl Pts',(-74.1735087234225,5.85486050285878,3.88838269279463));
#32331=CARTESIAN_POINT('Ctrl Pts',(-74.2065379851614,6.42585586326691,2.8473299594671));
#32332=CARTESIAN_POINT('Ctrl Pts',(-74.2395672469003,6.71349377199439,1.73312687672298));
#32333=CARTESIAN_POINT('Ctrl Pts',(-74.2725965086392,7.00113168072186,0.61892379397887));
#32334=CARTESIAN_POINT('Ctrl Pts',(-74.3056257703781,7.00541213776869,-0.568429638181864));
#32335=CARTESIAN_POINT('Ctrl Pts',(-74.3386550321169,6.72581509517529,-1.68467762582019));
#32336=CARTESIAN_POINT('Ctrl Pts',(-74.3716842938559,6.44621805258187,-2.80092561345853));
#32337=CARTESIAN_POINT('Ctrl Pts',(-74.4047135555948,5.88274351034823,-3.84606815657449));
#32338=CARTESIAN_POINT('Ctrl Pts',(-74.4377428173337,5.10384999586191,-4.6931271682288));
#32339=CARTESIAN_POINT('Ctrl Pts',(-74.4707720790725,4.32495648137559,-5.54018617988311));
#32340=CARTESIAN_POINT('Ctrl Pts',(-74.5038013408114,3.33064399463661,-6.18916166007575));
#32341=CARTESIAN_POINT('Ctrl Pts',(-74.5368306025503,2.24171509814475,-6.56120726819209));
#32342=CARTESIAN_POINT('Ctrl Pts',(-74.5698598642892,1.15278620165293,-6.93325287630843));
#32343=CARTESIAN_POINT('Ctrl Pts',(-74.6028891260281,-0.0307591045917431,
-7.02836861234847));
#32344=CARTESIAN_POINT('Ctrl Pts',(-74.635918387767,-1.16512768941995,-6.83499852704987));
#32345=CARTESIAN_POINT('Ctrl Pts',(-74.6689476495059,-2.2994962742482,-6.64162844175125));
#32346=CARTESIAN_POINT('Ctrl Pts',(-74.7019769112448,-3.38468813765996,
-6.15977253511398));
#32347=CARTESIAN_POINT('Ctrl Pts',(-74.7350061729836,-4.28885945826866,
-5.44797319602862));
#32348=CARTESIAN_POINT('Ctrl Pts',(-74.7680354347225,-5.19303077887736,
-4.73617385694327));
#32349=CARTESIAN_POINT('Ctrl Pts',(-74.8010646964614,-5.91618155668299,
-3.79443108540985));
#32350=CARTESIAN_POINT('Ctrl Pts',(-74.8340939582003,-6.37045363019433,
-2.73716056214661));
#32351=CARTESIAN_POINT('Ctrl Pts',(-74.8610054175981,-6.74058374568103,
-1.87572160585925));
#32352=CARTESIAN_POINT('Ctrl Pts',(-74.8879168769959,-6.93221593549224,
-0.937588349456712));
#32353=CARTESIAN_POINT('Ctrl Pts',(-74.9148283363937,-6.93316696520231,
0.00016807782604461));
#32354=CARTESIAN_POINT('Ctrl Pts',(-75.0941716636063,-6.93305363032429,
0.000176774812155918));
#32355=CARTESIAN_POINT('Ctrl Pts',(-75.0682934140262,-6.93212658934707,
-0.90161891061375));
#32356=CARTESIAN_POINT('Ctrl Pts',(-75.0424151644463,-6.75529560991023,
-1.80376749780292));
#32357=CARTESIAN_POINT('Ctrl Pts',(-75.0165369148662,-6.41232485292237,
-2.63757790554064));
#32358=CARTESIAN_POINT('Ctrl Pts',(-74.9835076531273,-5.97457998666652,
-3.70179757436449));
#32359=CARTESIAN_POINT('Ctrl Pts',(-74.9504783913884,-5.2661891510568,-4.65469259177645));
#32360=CARTESIAN_POINT('Ctrl Pts',(-74.9174491296495,-4.37321726968046,
-5.38049235101869));
#32361=CARTESIAN_POINT('Ctrl Pts',(-74.8844198679106,-3.48024538830414,
-6.1062921102609));
#32362=CARTESIAN_POINT('Ctrl Pts',(-74.8513906061717,-2.40269246116121,
-6.60499661133342));
#32363=CARTESIAN_POINT('Ctrl Pts',(-74.8183613444329,-1.27147422808607,
-6.81601646964816));
#32364=CARTESIAN_POINT('Ctrl Pts',(-74.785332082694,-0.140255995010866,
-7.02703632796292));
#32365=CARTESIAN_POINT('Ctrl Pts',(-74.7523028209551,1.04462754399656,-6.95037154351987));
#32366=CARTESIAN_POINT('Ctrl Pts',(-74.7192735592162,2.13922067110611,-6.59533639380998));
#32367=CARTESIAN_POINT('Ctrl Pts',(-74.6862442974773,3.23381379821559,-6.24030124410011));
#32368=CARTESIAN_POINT('Ctrl Pts',(-74.6532150357384,4.2381165134272,-5.60689572912343));
#32369=CARTESIAN_POINT('Ctrl Pts',(-74.6201857739995,5.03011250583151,-4.77207453901125));
#32370=CARTESIAN_POINT('Ctrl Pts',(-74.5871565122606,5.82210849823583,-3.93725334889907));
#32371=CARTESIAN_POINT('Ctrl Pts',(-74.5541272505218,6.40179776783287,-2.90101648365138));
#32372=CARTESIAN_POINT('Ctrl Pts',(-74.5210979887829,6.69875180230388,-1.7892600477104));
#32373=CARTESIAN_POINT('Ctrl Pts',(-74.488068727044,6.9957058367749,-0.677503611769395));
#32374=CARTESIAN_POINT('Ctrl Pts',(-74.4550394653051,7.0099246361199,0.509772394864872));
#32375=CARTESIAN_POINT('Ctrl Pts',(-74.4220102035662,6.73968070780564,1.62832158495628));
#32376=CARTESIAN_POINT('Ctrl Pts',(-74.3889809418273,6.46943677949138,2.74687077504773));
#32377=CARTESIAN_POINT('Ctrl Pts',(-74.3559516800884,5.91473012351782,3.79669314859627));
#32378=CARTESIAN_POINT('Ctrl Pts',(-74.3229224183495,5.14295402556832,4.65024204940911));
#32379=CARTESIAN_POINT('Ctrl Pts',(-74.2898931566106,4.37117792761887,5.50379095022191));
#32380=CARTESIAN_POINT('Ctrl Pts',(-74.2568638948718,3.38233238769347,6.16106637829903));
#32381=CARTESIAN_POINT('Ctrl Pts',(-74.2238346331329,2.29655576946821,6.54221360282011));
#32382=CARTESIAN_POINT('Ctrl Pts',(-74.190805371394,1.21077915124288,6.92336082734121));
#32383=CARTESIAN_POINT('Ctrl Pts',(-74.1577761096551,0.0280714547176494,
7.02837984830623));
#32384=CARTESIAN_POINT('Ctrl Pts',(-74.1247468479162,-1.10787595312376,
6.8445115311242));
#32385=CARTESIAN_POINT('Ctrl Pts',(-74.0917175861773,-2.24382336096507,
6.66064321394219));
#32386=CARTESIAN_POINT('Ctrl Pts',(-74.0586883244384,-3.33301048012259,
6.18788755861318));
#32387=CARTESIAN_POINT('Ctrl Pts',(-74.0256590626995,-4.24310809137114,
5.48368133211101));
#32388=CARTESIAN_POINT('Ctrl Pts',(-73.9926298009606,-5.15320570261977,
4.77947510560879));
#32389=CARTESIAN_POINT('Ctrl Pts',(-73.9596005392217,-5.88421380595942,
3.84381830793336));
#32390=CARTESIAN_POINT('Ctrl Pts',(-73.9265712774829,-6.34731962545765,
2.79038721318067));
#32391=CARTESIAN_POINT('Ctrl Pts',(-73.899104739524,-6.7324300669436,1.91437292682431));
#32392=CARTESIAN_POINT('Ctrl Pts',(-73.8716382015651,-6.93227843232692,
0.956914352367065));
#32393=CARTESIAN_POINT('Ctrl Pts',(-73.8441716636062,-6.9332265516286,-0.000160595751058418));
#32394=CARTESIAN_POINT('Origin',(-87.75,0.,0.));
#32395=CARTESIAN_POINT('',(-72.4148283363937,-6.93247994518944,8.66496906495873E-5));
#32396=CARTESIAN_POINT('',(-72.5941716636063,-6.93243957992525,5.60106990600447E-5));
#32397=CARTESIAN_POINT('',(-87.75,-6.933,-8.4904762584886E-16));
#32398=CARTESIAN_POINT('Ctrl Pts',(-72.4148283363937,-6.93247994518944,
8.66496906495873E-5));
#32399=CARTESIAN_POINT('Ctrl Pts',(-72.4285479285959,-6.93269109193388,
0.478295513083371));
#32400=CARTESIAN_POINT('Ctrl Pts',(-72.442267520798,-6.88392184964319,0.956461913326707));
#32401=CARTESIAN_POINT('Ctrl Pts',(-72.4559871130002,-6.78573659267738,
1.42425639974906));
#32402=CARTESIAN_POINT('Ctrl Pts',(-72.4890163747391,-6.54936028473497,
2.55044924166249));
#32403=CARTESIAN_POINT('Ctrl Pts',(-72.522045636478,-6.02657736140281,3.61652827731066));
#32404=CARTESIAN_POINT('Ctrl Pts',(-72.5550748982169,-5.2809025804778,4.4929717707693));
#32405=CARTESIAN_POINT('Ctrl Pts',(-72.5881041599558,-4.53522779955277,
5.36941526422797));
#32406=CARTESIAN_POINT('Ctrl Pts',(-72.6211334216947,-3.56666116103487,
6.05622321549709));
#32407=CARTESIAN_POINT('Ctrl Pts',(-72.6541626834336,-2.49287727270111,
6.46995288241554));
#32408=CARTESIAN_POINT('Ctrl Pts',(-72.6871919451724,-1.41909338436735,
6.88368254933399));
#32409=CARTESIAN_POINT('Ctrl Pts',(-72.7202212069113,-0.240092246217731,
7.02433393190177));
#32410=CARTESIAN_POINT('Ctrl Pts',(-72.7532504686502,0.900885097731738,
6.87481879311097));
#32411=CARTESIAN_POINT('Ctrl Pts',(-72.7862797303891,2.04186244168121,6.72530365432016));
#32412=CARTESIAN_POINT('Ctrl Pts',(-72.819308992128,3.14481599143052,6.28562199417078));
#32413=CARTESIAN_POINT('Ctrl Pts',(-72.8523382538669,4.07574399511096,5.60919230226098));
#32414=CARTESIAN_POINT('Ctrl Pts',(-72.8853675156058,5.0066719987914,4.93276261035119));
#32415=CARTESIAN_POINT('Ctrl Pts',(-72.9183967773447,5.76557445640296,4.019584886681));
#32416=CARTESIAN_POINT('Ctrl Pts',(-72.9514260390835,6.26024960764436,2.98060434264857));
#32417=CARTESIAN_POINT('Ctrl Pts',(-72.9844553008224,6.75492475888575,1.94162379861618));
#32418=CARTESIAN_POINT('Ctrl Pts',(-73.0174845625613,6.98537260375701,0.77684043422156));
#32419=CARTESIAN_POINT('Ctrl Pts',(-73.0505138243002,6.92359521348393,-0.37223207444993));
#32420=CARTESIAN_POINT('Ctrl Pts',(-73.0835430860391,6.86181782321086,-1.52130458312149));
#32421=CARTESIAN_POINT('Ctrl Pts',(-73.116572347778,6.50781519779342,-2.65466623606991));
#32422=CARTESIAN_POINT('Ctrl Pts',(-73.1496016095169,5.90459637599201,-3.6346208927547));
#32423=CARTESIAN_POINT('Ctrl Pts',(-73.1826308712558,5.30137755419063,-4.61457554943943));
#32424=CARTESIAN_POINT('Ctrl Pts',(-73.2156601329947,4.44894253600529,-5.44112320986056));
#32425=CARTESIAN_POINT('Ctrl Pts',(-73.2486893947336,3.45085668537816,-6.0138436572967));
#32426=CARTESIAN_POINT('Ctrl Pts',(-73.2817186564725,2.45277083475103,-6.58656410473285));
#32427=CARTESIAN_POINT('Ctrl Pts',(-73.3147479182114,1.3090341516821,-6.90545733918401));
#32428=CARTESIAN_POINT('Ctrl Pts',(-73.3477771799502,0.158603276043082,
-6.93177988674304));
#32429=CARTESIAN_POINT('Ctrl Pts',(-73.3808064416891,-0.991827599595997,
-6.95810243430206));
#32430=CARTESIAN_POINT('Ctrl Pts',(-73.413835703428,-2.14895266780516,-6.6918542949689));
#32431=CARTESIAN_POINT('Ctrl Pts',(-73.446864965167,-3.17218868615638,-6.16538290269537));
#32432=CARTESIAN_POINT('Ctrl Pts',(-73.4798942269059,-4.19542470450755,
-5.63891151042187));
#32433=CARTESIAN_POINT('Ctrl Pts',(-73.5129234886447,-5.08477167300079,
-4.85221686520803));
#32434=CARTESIAN_POINT('Ctrl Pts',(-73.5459527503836,-5.73217966349153,
-3.9008772991317));
#32435=CARTESIAN_POINT('Ctrl Pts',(-73.5789820121225,-6.37958765398229,
-2.94953773305535));
#32436=CARTESIAN_POINT('Ctrl Pts',(-73.6120112738614,-6.78505666647053,
-1.83355324611651));
#32437=CARTESIAN_POINT('Ctrl Pts',(-73.6450405356003,-6.89932482767586,
-0.688508765116595));
#32438=CARTESIAN_POINT('Ctrl Pts',(-73.6516364691981,-6.92214414497133,
-0.459843727946572));
#32439=CARTESIAN_POINT('Ctrl Pts',(-73.6582324027959,-6.93335038122188,
-0.230019779101979));
#32440=CARTESIAN_POINT('Ctrl Pts',(-73.6648283363937,-6.9331147324061,-0.00017295491683611));
#32441=CARTESIAN_POINT('Ctrl Pts',(-73.8441716636062,-6.9332265516286,-0.000160595751058418));
#32442=CARTESIAN_POINT('Ctrl Pts',(-73.8386089398262,-6.93341857167108,
-0.19399440113044));
#32443=CARTESIAN_POINT('Ctrl Pts',(-73.8330462160462,-6.92545223918872,
-0.387812471190364));
#32444=CARTESIAN_POINT('Ctrl Pts',(-73.8274834922662,-6.90921426020527,
-0.580935051256329));
#32445=CARTESIAN_POINT('Ctrl Pts',(-73.7944542305273,-6.81279953979783,
-1.72762082911074));
#32446=CARTESIAN_POINT('Ctrl Pts',(-73.7614249687884,-6.42476656332614,
-2.84978699298969));
#32447=CARTESIAN_POINT('Ctrl Pts',(-73.7283957070495,-5.79225883800486,
-3.81109758216143));
#32448=CARTESIAN_POINT('Ctrl Pts',(-73.6953664453106,-5.15975111268355,
-4.77240817133319));
#32449=CARTESIAN_POINT('Ctrl Pts',(-73.6623371835717,-4.28276863851263,
-5.57286318579773));
#32450=CARTESIAN_POINT('Ctrl Pts',(-73.6293079218328,-3.26785913721962,
-6.11521249724753));
#32451=CARTESIAN_POINT('Ctrl Pts',(-73.5962786600939,-2.25294963592661,
-6.65756180869732));
#32452=CARTESIAN_POINT('Ctrl Pts',(-73.5632493983551,-1.1001131075115,-6.94180541713237));
#32453=CARTESIAN_POINT('Ctrl Pts',(-73.5302201366162,0.050588235559008,
-6.93340955501874));
#32454=CARTESIAN_POINT('Ctrl Pts',(-73.4971908748773,1.20128957862948,-6.9250136929051));
#32455=CARTESIAN_POINT('Ctrl Pts',(-73.4641616131384,2.34985573635535,-6.62397836024279));
#32456=CARTESIAN_POINT('Ctrl Pts',(-73.4311323513995,3.35674331880206,-6.06687741089926));
#32457=CARTESIAN_POINT('Ctrl Pts',(-73.3981030896606,4.36363090124879,-5.50977646155573));
#32458=CARTESIAN_POINT('Ctrl Pts',(-73.3650738279217,5.22883990841635,-4.69660989553097));
#32459=CARTESIAN_POINT('Ctrl Pts',(-73.3320445661828,5.847253018982,-3.72617221276849));
#32460=CARTESIAN_POINT('Ctrl Pts',(-73.299015304444,6.46566612954764,-2.755734530006));
#32461=CARTESIAN_POINT('Ctrl Pts',(-73.265986042705,6.83728334351137,-1.62802573050579));
#32462=CARTESIAN_POINT('Ctrl Pts',(-73.2329567809661,6.91695556306483,-0.480055169525972));
#32463=CARTESIAN_POINT('Ctrl Pts',(-73.1999275192272,6.99662778261828,0.667915391453817));
#32464=CARTESIAN_POINT('Ctrl Pts',(-73.1668982574884,6.78435500776147,1.83614771391322));
#32465=CARTESIAN_POINT('Ctrl Pts',(-73.1338689957495,6.30592701333244,2.88270909557768));
#32466=CARTESIAN_POINT('Ctrl Pts',(-73.1008397340106,5.8274990189034,3.92927047724217));
#32467=CARTESIAN_POINT('Ctrl Pts',(-73.0678104722717,5.08291580490211,4.85416091811173));
#32468=CARTESIAN_POINT('Ctrl Pts',(-73.0347812105328,4.16263943576538,5.54501218709328));
#32469=CARTESIAN_POINT('Ctrl Pts',(-73.0017519487939,3.24236306662865,6.23586345607482));
#32470=CARTESIAN_POINT('Ctrl Pts',(-72.968722687055,2.14639354235647,6.69267555316836));
#32471=CARTESIAN_POINT('Ctrl Pts',(-72.9356934253161,1.00788410070812,6.85994875102882));
#32472=CARTESIAN_POINT('Ctrl Pts',(-72.9026641635773,-0.130625340940225,
7.02722194888928));
#32473=CARTESIAN_POINT('Ctrl Pts',(-72.8696349018384,-1.31167469996475,
6.90495624751666));
#32474=CARTESIAN_POINT('Ctrl Pts',(-72.8366056400995,-2.39177408670627,
6.50800614208088));
#32475=CARTESIAN_POINT('Ctrl Pts',(-72.8035763783606,-3.4718734734478,6.1110560366451));
#32476=CARTESIAN_POINT('Ctrl Pts',(-72.7705471166217,-4.45102288790632,
5.43942152714615));
#32477=CARTESIAN_POINT('Ctrl Pts',(-72.7375178548828,-5.21026198319463,
4.57470188030638));
#32478=CARTESIAN_POINT('Ctrl Pts',(-72.7044885931439,-5.96950107848292,
3.70998223346664));
#32479=CARTESIAN_POINT('Ctrl Pts',(-72.671459331405,-6.508829854601,2.65217744928609));
#32480=CARTESIAN_POINT('Ctrl Pts',(-72.6384300696661,-6.76272333921484,
1.5298039954324));
#32481=CARTESIAN_POINT('Ctrl Pts',(-72.6236772676462,-6.87612703386224,
1.02848630059374));
#32482=CARTESIAN_POINT('Ctrl Pts',(-72.6089244656262,-6.93258528704124,
0.514286907138951));
#32483=CARTESIAN_POINT('Ctrl Pts',(-72.5941716636063,-6.93243957992525,
5.60106990600447E-5));
#32484=CARTESIAN_POINT('Origin',(-87.75,0.,0.));
#32485=CARTESIAN_POINT('',(-71.1648283363937,-6.93357792730774,3.67079550465076E-5));
#32486=CARTESIAN_POINT('',(-71.3441716636063,-6.93353164992697,7.2489118278869E-5));
#32487=CARTESIAN_POINT('',(-87.75,-6.933,-8.4904762584886E-16));
#32488=CARTESIAN_POINT('Ctrl Pts',(-71.1648283363937,-6.93357792730774,
3.67079550465076E-5));
#32489=CARTESIAN_POINT('Ctrl Pts',(-71.165834192657,-6.93358820915741,0.0350807501651851));
#32490=CARTESIAN_POINT('Ctrl Pts',(-71.1668400489202,-6.93332806093716,
0.0701246392026087));
#32491=CARTESIAN_POINT('Ctrl Pts',(-71.1678459051835,-6.93279653847796,
0.105164411732063));
#32492=CARTESIAN_POINT('Ctrl Pts',(-71.2008751669224,-6.91534295682192,
1.25576401568685));
#32493=CARTESIAN_POINT('Ctrl Pts',(-71.2339044286613,-6.60527577829948,
2.40192492933702));
#32494=CARTESIAN_POINT('Ctrl Pts',(-71.2669336904002,-6.04026616787353,
3.40439598441036));
#32495=CARTESIAN_POINT('Ctrl Pts',(-71.2999629521391,-5.47525655744756,
4.40686703948373));
#32496=CARTESIAN_POINT('Ctrl Pts',(-71.332992213878,-4.65530451511805,5.26564823598026));
#32497=CARTESIAN_POINT('Ctrl Pts',(-71.3660214756168,-3.68002893249243,
5.87640319017046));
#32498=CARTESIAN_POINT('Ctrl Pts',(-71.3990507373557,-2.70475334986681,
6.48715814436066));
#32499=CARTESIAN_POINT('Ctrl Pts',(-71.4320799990946,-1.57415422694506,
6.84988685624452));
#32500=CARTESIAN_POINT('Ctrl Pts',(-71.4651092608335,-0.425592074663672,
6.92052012376312));
#32501=CARTESIAN_POINT('Ctrl Pts',(-71.4981385225724,0.722970077617721,
6.99115339128172));
#32502=CARTESIAN_POINT('Ctrl Pts',(-71.5311677843113,1.88949525925877,6.76969121443506));
#32503=CARTESIAN_POINT('Ctrl Pts',(-71.5641970460502,2.93225817459818,6.28303982121147));
#32504=CARTESIAN_POINT('Ctrl Pts',(-71.5972263077891,3.97502108993757,5.7963884279879));
#32505=CARTESIAN_POINT('Ctrl Pts',(-71.630255569528,4.89402173897534,5.04454781838742));
#32506=CARTESIAN_POINT('Ctrl Pts',(-71.6632848312669,5.57760746238822,4.11886178366526));
#32507=CARTESIAN_POINT('Ctrl Pts',(-71.6963140930058,6.26119318580114,3.19317574894305));
#32508=CARTESIAN_POINT('Ctrl Pts',(-71.7293433547446,6.70936398358914,2.09364428909914));
#32509=CARTESIAN_POINT('Ctrl Pts',(-71.7623726164835,6.86766999061181,0.953853394121363));
#32510=CARTESIAN_POINT('Ctrl Pts',(-71.7954018782224,7.02597599763448,-0.185937500856344));
#32511=CARTESIAN_POINT('Ctrl Pts',(-71.8284311399613,6.89441721389184,-1.36598783096791));
#32512=CARTESIAN_POINT('Ctrl Pts',(-71.8614604017002,6.48897718420248,-2.44292908213207));
#32513=CARTESIAN_POINT('Ctrl Pts',(-71.8944896634391,6.08353715451311,-3.51987033329624));
#32514=CARTESIAN_POINT('Ctrl Pts',(-71.9275189251779,5.40421587887703,-4.493702505513));
#32515=CARTESIAN_POINT('Ctrl Pts',(-71.9605481869168,4.53354651658966,-5.2461112625777));
#32516=CARTESIAN_POINT('Ctrl Pts',(-71.9935774486557,3.66287715430227,-5.99852001964243));
#32517=CARTESIAN_POINT('Ctrl Pts',(-72.0266067103947,2.60085970536358,-6.52950536155508));
#32518=CARTESIAN_POINT('Ctrl Pts',(-72.0596359721336,1.47652244907446,-6.77455598949526));
#32519=CARTESIAN_POINT('Ctrl Pts',(-72.0926652338725,0.352185192785344,
-7.01960661743543));
#32520=CARTESIAN_POINT('Ctrl Pts',(-72.1256944956113,-0.834471870854206,
-6.97872253140312));
#32521=CARTESIAN_POINT('Ctrl Pts',(-72.1587237573502,-1.93927755219505,
-6.65687088450567));
#32522=CARTESIAN_POINT('Ctrl Pts',(-72.1917530190891,-3.04408323353587,
-6.33501923760822));
#32523=CARTESIAN_POINT('Ctrl Pts',(-72.224782280828,-4.06703753257799,-5.73220002984564));
#32524=CARTESIAN_POINT('Ctrl Pts',(-72.2578115425669,-4.88385809111654,
-4.9216519120375));
#32525=CARTESIAN_POINT('Ctrl Pts',(-72.2908408043058,-5.70067864965511,
-4.11110379422934));
#32526=CARTESIAN_POINT('Ctrl Pts',(-72.3238700660447,-6.31136546769011,
-3.09282676637561));
#32527=CARTESIAN_POINT('Ctrl Pts',(-72.3568993277835,-6.64172403043128,
-1.99053492835938));
#32528=CARTESIAN_POINT('Ctrl Pts',(-72.3762089973202,-6.83485927897507,
-1.34610965196703));
#32529=CARTESIAN_POINT('Ctrl Pts',(-72.395518666857,-6.93218276625011,-0.672969443054267));
#32530=CARTESIAN_POINT('Ctrl Pts',(-72.4148283363937,-6.93247994518944,
8.66496906495873E-5));
#32531=CARTESIAN_POINT('Ctrl Pts',(-72.5941716636063,-6.93243957992525,
5.60106990600447E-5));
#32532=CARTESIAN_POINT('Ctrl Pts',(-72.5758952038873,-6.93225907114917,
-0.636997225174157));
#32533=CARTESIAN_POINT('Ctrl Pts',(-72.5576187441684,-6.84520613908146,
-1.27409880997282));
#32534=CARTESIAN_POINT('Ctrl Pts',(-72.5393422844495,-6.67193004491143,
-1.8868165525589));
#32535=CARTESIAN_POINT('Ctrl Pts',(-72.5063130227106,-6.35878507288456,
-2.99412152316961));
#32536=CARTESIAN_POINT('Ctrl Pts',(-72.4732837609717,-5.76403693572121,
-4.02178934086416));
#32537=CARTESIAN_POINT('Ctrl Pts',(-72.4402544992328,-4.95994370115113,
-4.84496498528249));
#32538=CARTESIAN_POINT('Ctrl Pts',(-72.4072252374939,-4.15585046658107,
-5.66814062970079));
#32539=CARTESIAN_POINT('Ctrl Pts',(-72.374195975755,-3.14241213460429,-6.28682410084286));
#32540=CARTESIAN_POINT('Ctrl Pts',(-72.3411667140161,-2.04275493472216,
-6.62584934207459));
#32541=CARTESIAN_POINT('Ctrl Pts',(-72.3081374522772,-0.94309773484001,
-6.96487458330633));
#32542=CARTESIAN_POINT('Ctrl Pts',(-72.2751081905383,0.24277833294748,-7.02424159462772));
#32543=CARTESIAN_POINT('Ctrl Pts',(-72.2420789287995,1.37079696495661,-6.79673766656238));
#32544=CARTESIAN_POINT('Ctrl Pts',(-72.2090496670606,2.49881559696574,-6.56923373849704));
#32545=CARTESIAN_POINT('Ctrl Pts',(-72.1760204053217,3.56897679319648,-6.05485887104497));
#32546=CARTESIAN_POINT('Ctrl Pts',(-72.1429911435828,4.45126286150812,-5.31610629737223));
#32547=CARTESIAN_POINT('Ctrl Pts',(-72.1099618818439,5.33354892981976,-4.57735372369949));
#32548=CARTESIAN_POINT('Ctrl Pts',(-72.076932620105,6.02795987021227,-3.61422344380608));
#32549=CARTESIAN_POINT('Ctrl Pts',(-72.0439033583661,6.45012922631898,-2.5437295829132));
#32550=CARTESIAN_POINT('Ctrl Pts',(-72.0108740966272,6.87229858242569,-1.47323572202035));
#32551=CARTESIAN_POINT('Ctrl Pts',(-71.9778448348883,7.02222635424661,-0.295378280127947));
#32552=CARTESIAN_POINT('Ctrl Pts',(-71.9448155731494,6.88169728323131,0.846740650476222));
#32553=CARTESIAN_POINT('Ctrl Pts',(-71.9117863114105,6.74116821221601,1.98885958108042));
#32554=CARTESIAN_POINT('Ctrl Pts',(-71.8787570496716,6.31018229836454,3.09524000039637));
#32555=CARTESIAN_POINT('Ctrl Pts',(-71.8457277879328,5.64110155411151,4.0314638139766));
#32556=CARTESIAN_POINT('Ctrl Pts',(-71.8126985261939,4.9720208098585,4.96768762755681));
#32557=CARTESIAN_POINT('Ctrl Pts',(-71.779669264455,4.06484523520388,5.73375483540125));
#32558=CARTESIAN_POINT('Ctrl Pts',(-71.7466400027161,3.02979081910206,6.23659320620537));
#32559=CARTESIAN_POINT('Ctrl Pts',(-71.7136107409772,1.9947364030002,6.7394315770095));
#32560=CARTESIAN_POINT('Ctrl Pts',(-71.6805814792383,0.831803145451077,
6.97904111077336));
#32561=CARTESIAN_POINT('Ctrl Pts',(-71.6475522174994,-0.31772005352466,
6.92631079253525));
#32562=CARTESIAN_POINT('Ctrl Pts',(-71.6145229557605,-1.46724325250037,
6.87358047429715));
#32563=CARTESIAN_POINT('Ctrl Pts',(-71.5814936940217,-2.60335639290266,
6.5285103040571));
#32564=CARTESIAN_POINT('Ctrl Pts',(-71.5484644322828,-3.58802904618852,
5.93302408480781));
#32565=CARTESIAN_POINT('Ctrl Pts',(-71.5154351705439,-4.57270169947441,
5.3375378655585));
#32566=CARTESIAN_POINT('Ctrl Pts',(-71.482405908805,-5.40593386564384,4.49163559729995));
#32567=CARTESIAN_POINT('Ctrl Pts',(-71.4493766470661,-5.98649320358376,
3.49808895693742));
#32568=CARTESIAN_POINT('Ctrl Pts',(-71.4163473853272,-6.56705254152368,
2.5045423165749));
#32569=CARTESIAN_POINT('Ctrl Pts',(-71.3833181235883,-6.89493905123409,
1.36335130410841));
#32570=CARTESIAN_POINT('Ctrl Pts',(-71.3502888618495,-6.93031663379197,
0.213163276828843));
#32571=CARTESIAN_POINT('Ctrl Pts',(-71.3482497957684,-6.93250067378638,
0.142156258512689));
#32572=CARTESIAN_POINT('Ctrl Pts',(-71.3462107296874,-6.9335698957285,0.0711149505267199));
#32573=CARTESIAN_POINT('Ctrl Pts',(-71.3441716636063,-6.93353164992697,
7.2489118278869E-5));
#32574=CARTESIAN_POINT('Origin',(-87.75,0.,0.));
#32575=CARTESIAN_POINT('',(-69.9148283363937,-6.93260597399068,-0.000136960269141728));
#32576=CARTESIAN_POINT('',(-70.0941716636062,-6.93269186048085,-0.000156184372951973));
#32577=CARTESIAN_POINT('',(-87.75,-6.933,-8.4904762584886E-16));
#32578=CARTESIAN_POINT('Ctrl Pts',(-69.9148283363937,-6.93260597399068,
-0.000136960269141728));
#32579=CARTESIAN_POINT('Ctrl Pts',(-69.9361497184569,-6.93207477653448,
0.74300050956666));
#32580=CARTESIAN_POINT('Ctrl Pts',(-69.9574711005202,-6.81303361409483,
1.48630411053334));
#32581=CARTESIAN_POINT('Ctrl Pts',(-69.9787924825834,-6.57829275596597,
2.19107092861746));
#32582=CARTESIAN_POINT('Ctrl Pts',(-70.0118217443223,-6.21465229302841,
3.28283541322393));
#32583=CARTESIAN_POINT('Ctrl Pts',(-70.0448510060613,-5.57336082823614,
4.28212103423564));
#32584=CARTESIAN_POINT('Ctrl Pts',(-70.0778802678001,-4.73233114382751,
5.06752102537199));
#32585=CARTESIAN_POINT('Ctrl Pts',(-70.110909529539,-3.89130145941882,5.85292101650838));
#32586=CARTESIAN_POINT('Ctrl Pts',(-70.1439387912779,-2.85053355539373,
6.42443537776939));
#32587=CARTESIAN_POINT('Ctrl Pts',(-70.1769680530168,-1.73647402822026,
6.71262879554228));
#32588=CARTESIAN_POINT('Ctrl Pts',(-70.2099973147557,-0.622414501046784,
7.00082221331518));
#32589=CARTESIAN_POINT('Ctrl Pts',(-70.2430265764946,0.564936649275099,
7.00569468759997));
#32590=CARTESIAN_POINT('Ctrl Pts',(-70.2760558382335,1.68132390603513,6.72665424415598));
#32591=CARTESIAN_POINT('Ctrl Pts',(-70.3090850999724,2.79771116279514,6.44761380071201));
#32592=CARTESIAN_POINT('Ctrl Pts',(-70.3421143617113,3.84313452599332,5.88466043953927));
#32593=CARTESIAN_POINT('Ctrl Pts',(-70.3751436234501,4.69058179085922,5.10618936788353));
#32594=CARTESIAN_POINT('Ctrl Pts',(-70.408172885189,5.53802905572517,4.32771829622775));
#32595=CARTESIAN_POINT('Ctrl Pts',(-70.4412021469279,6.18750022225883,3.33372951408891));
#32596=CARTESIAN_POINT('Ctrl Pts',(-70.4742314086668,6.56008872714797,2.24498625594301));
#32597=CARTESIAN_POINT('Ctrl Pts',(-70.5072606704057,6.9326772320371,1.15624299779714));
#32598=CARTESIAN_POINT('Ctrl Pts',(-70.5402899321446,7.02838307528173,-0.0272547363557275));
#32599=CARTESIAN_POINT('Ctrl Pts',(-70.5733191938835,6.8355786133952,-1.16171959504913));
#32600=CARTESIAN_POINT('Ctrl Pts',(-70.6063484556224,6.64277415150867,-2.29618445374251));
#32601=CARTESIAN_POINT('Ctrl Pts',(-70.6393777173613,6.16145938449097,-3.38161643697636));
#32602=CARTESIAN_POINT('Ctrl Pts',(-70.6724069791002,5.45011095625454,-4.28614255035237));
#32603=CARTESIAN_POINT('Ctrl Pts',(-70.7054362408391,4.7387625280181,-5.1906686637284));
#32604=CARTESIAN_POINT('Ctrl Pts',(-70.7384655025779,3.79738043856291,-5.91428890724661));
#32605=CARTESIAN_POINT('Ctrl Pts',(-70.7714947643168,2.740336548058,-6.36908808235563));
#32606=CARTESIAN_POINT('Ctrl Pts',(-70.8045240260557,1.68329265755312,-6.82388725746464));
#32607=CARTESIAN_POINT('Ctrl Pts',(-70.8375532877946,0.510586965998494,
-7.00986536416448));
#32608=CARTESIAN_POINT('Ctrl Pts',(-70.8705825495335,-0.635304338800435,
-6.90442726042705));
#32609=CARTESIAN_POINT('Ctrl Pts',(-70.9036118112724,-1.78119564359943,
-6.79898915668962));
#32610=CARTESIAN_POINT('Ctrl Pts',(-70.9366410730113,-2.90027256164274,
-6.40213484251487));
#32611=CARTESIAN_POINT('Ctrl Pts',(-70.9696703347502,-3.85657445566894,
-5.76207956082774));
#32612=CARTESIAN_POINT('Ctrl Pts',(-71.0026995964891,-4.81287634969511,
-5.12202427914062));
#32613=CARTESIAN_POINT('Ctrl Pts',(-71.0357288582279,-5.60640321970419,
-4.23876802994113));
#32614=CARTESIAN_POINT('Ctrl Pts',(-71.0687581199668,-6.14074666231391,
-3.21962075821167));
#32615=CARTESIAN_POINT('Ctrl Pts',(-71.1007815254425,-6.65881748270362,
-2.23151007684142));
#32616=CARTESIAN_POINT('Ctrl Pts',(-71.1328049309181,-6.93325058447245,
-1.11565905712287));
#32617=CARTESIAN_POINT('Ctrl Pts',(-71.1648283363937,-6.93357792730774,
3.67079550465076E-5));
#32618=CARTESIAN_POINT('Ctrl Pts',(-71.3441716636063,-6.93353164992697,
7.2489118278869E-5));
#32619=CARTESIAN_POINT('Ctrl Pts',(-71.3131814679485,-6.93295038143177,
-1.0796471921201));
#32620=CARTESIAN_POINT('Ctrl Pts',(-71.2821912722906,-6.67655934644521,
-2.1596332980329));
#32621=CARTESIAN_POINT('Ctrl Pts',(-71.2512010766328,-6.19016240212286,
-3.12355833346308));
#32622=CARTESIAN_POINT('Ctrl Pts',(-71.2181718148939,-5.67176193249052,
-4.1509068743828));
#32623=CARTESIAN_POINT('Ctrl Pts',(-71.185142553155,-4.8920923378205,-5.04641891412959));
#32624=CARTESIAN_POINT('Ctrl Pts',(-71.1521132914161,-3.94587845179987,
-5.70129550811248));
#32625=CARTESIAN_POINT('Ctrl Pts',(-71.1190840296772,-2.99966456577927,
-6.35617210209535));
#32626=CARTESIAN_POINT('Ctrl Pts',(-71.0860547679383,-1.88690638840805,
-6.77041325031432));
#32627=CARTESIAN_POINT('Ctrl Pts',(-71.0530255061994,-0.742796870656711,
-6.89369132150147));
#32628=CARTESIAN_POINT('Ctrl Pts',(-71.0199962444605,0.401312647094657,
-7.01696939268861));
#32629=CARTESIAN_POINT('Ctrl Pts',(-70.9869669827217,1.57677350522616,-6.84928438684391));
#32630=CARTESIAN_POINT('Ctrl Pts',(-70.9539377209828,2.64077478094005,-6.41100895207245));
#32631=CARTESIAN_POINT('Ctrl Pts',(-70.9209084592439,3.70477605665393,-5.97273351730099));
#32632=CARTESIAN_POINT('Ctrl Pts',(-70.8878791975049,4.65731774995022,-5.26386765360277));
#32633=CARTESIAN_POINT('Ctrl Pts',(-70.8548499357661,5.38267218067527,-4.37053399741801));
#32634=CARTESIAN_POINT('Ctrl Pts',(-70.8218206740272,6.10802661140029,-3.47720034123327));
#32635=CARTESIAN_POINT('Ctrl Pts',(-70.7887914122883,6.60619377955409,-2.39939889256199));
#32636=CARTESIAN_POINT('Ctrl Pts',(-70.7557621505494,6.81664958303712,-1.26807558500348));
#32637=CARTESIAN_POINT('Ctrl Pts',(-70.7227328888105,7.02710538652015,-0.136752277444937));
#32638=CARTESIAN_POINT('Ctrl Pts',(-70.6897036270716,6.94984982533242,1.04809288900076));
#32639=CARTESIAN_POINT('Ctrl Pts',(-70.6566743653327,6.59426895253398,2.14250885852276));
#32640=CARTESIAN_POINT('Ctrl Pts',(-70.6236451035938,6.23868807973553,3.2369248280448));
#32641=CARTESIAN_POINT('Ctrl Pts',(-70.590615841855,5.60478189532636,4.24091160064306));
#32642=CARTESIAN_POINT('Ctrl Pts',(-70.5575865801161,4.76956591754889,5.03249125040055));
#32643=CARTESIAN_POINT('Ctrl Pts',(-70.5245573183772,3.93434993977144,5.82407090015802));
#32644=CARTESIAN_POINT('Ctrl Pts',(-70.4915280566383,2.89782416862569,6.40324342707473));
#32645=CARTESIAN_POINT('Ctrl Pts',(-70.4584987948994,1.78591980875956,6.69964309973914));
#32646=CARTESIAN_POINT('Ctrl Pts',(-70.4254695331605,0.674015448893421,
6.99604277240355));
#32647=CARTESIAN_POINT('Ctrl Pts',(-70.3924402714216,-0.513267499693122,
7.00966959081566));
#32648=CARTESIAN_POINT('Ctrl Pts',(-70.3594110096827,-1.63168180636135,
6.73886798431246));
#32649=CARTESIAN_POINT('Ctrl Pts',(-70.3263817479438,-2.75009611302958,
6.46806637780926));
#32650=CARTESIAN_POINT('Ctrl Pts',(-70.293352486205,-3.79964177777951,5.91283634639075));
#32651=CARTESIAN_POINT('Ctrl Pts',(-70.2603232244661,-4.65280576275503,
5.14063476248562));
#32652=CARTESIAN_POINT('Ctrl Pts',(-70.2272939627272,-5.50596974773053,
4.36843317858052));
#32653=CARTESIAN_POINT('Ctrl Pts',(-70.1942647009883,-6.16275205293163,
3.3792600421888));
#32654=CARTESIAN_POINT('Ctrl Pts',(-70.1612354392494,-6.54335785879107,
2.29329351784705));
#32655=CARTESIAN_POINT('Ctrl Pts',(-70.1388808473683,-6.80095633388884,
1.55829863240126));
#32656=CARTESIAN_POINT('Ctrl Pts',(-70.1165262554873,-6.93204550151055,
0.778965200746742));
#32657=CARTESIAN_POINT('Ctrl Pts',(-70.0941716636062,-6.93269186048085,
-0.000156184372951973));
#32658=CARTESIAN_POINT('Origin',(-87.75,0.,0.));
#32659=CARTESIAN_POINT('',(-68.6648283363937,-6.93289541479494,0.00017741184833428));
#32660=CARTESIAN_POINT('',(-68.8441716636063,-6.93278929229388,0.000169878797845651));
#32661=CARTESIAN_POINT('',(-87.75,-6.933,-8.4904762584886E-16));
#32662=CARTESIAN_POINT('Ctrl Pts',(-68.6648283363937,-6.93289541479494,
0.00017741184833428));
#32663=CARTESIAN_POINT('Ctrl Pts',(-68.673435982518,-6.9331916959442,0.300153181373251));
#32664=CARTESIAN_POINT('Ctrl Pts',(-68.6820436286424,-6.91408350322542,
0.600091477363466));
#32665=CARTESIAN_POINT('Ctrl Pts',(-68.6906512747667,-6.87526712238957,
0.897457181683508));
#32666=CARTESIAN_POINT('Ctrl Pts',(-68.7236805365056,-6.7263208966894,2.03850893244921));
#32667=CARTESIAN_POINT('Ctrl Pts',(-68.7567097982446,-6.28718922697543,
3.14168157166794));
#32668=CARTESIAN_POINT('Ctrl Pts',(-68.7897390599834,-5.61122378248358,
4.07294672939748));
#32669=CARTESIAN_POINT('Ctrl Pts',(-68.8227683217223,-4.93525833799173,
5.00421188712702));
#32670=CARTESIAN_POINT('Ctrl Pts',(-68.8557975834612,-4.02245911872201,
5.76356956336737));
#32671=CARTESIAN_POINT('Ctrl Pts',(-68.8888268452001,-2.983725350259,6.25876269174234));
#32672=CARTESIAN_POINT('Ctrl Pts',(-68.9218561069389,-1.94499158179603,
6.75395582011729));
#32673=CARTESIAN_POINT('Ctrl Pts',(-68.9548853686779,-0.780323264139777,
6.98498440062688));
#32674=CARTESIAN_POINT('Ctrl Pts',(-68.9879146304168,0.368779904078343,
6.92377994882979));
#32675=CARTESIAN_POINT('Ctrl Pts',(-69.0209438921557,1.51788307229653,6.86257549703268));
#32676=CARTESIAN_POINT('Ctrl Pts',(-69.0539731538946,2.65142109107649,6.5091380129289));
#32677=CARTESIAN_POINT('Ctrl Pts',(-69.0870024156334,3.63167639255737,5.90640787426305));
#32678=CARTESIAN_POINT('Ctrl Pts',(-69.1200316773723,4.6119316940382,5.30367773559724));
#32679=CARTESIAN_POINT('Ctrl Pts',(-69.1530609391112,5.43890427821992,4.45165494236935));
#32680=CARTESIAN_POINT('Ctrl Pts',(-69.1860902008501,6.01212230288514,3.45385477583784));
#32681=CARTESIAN_POINT('Ctrl Pts',(-69.219119462589,6.58534032755038,2.4560546093063));
#32682=CARTESIAN_POINT('Ctrl Pts',(-69.2521487243279,6.90480379269919,1.31247706947107));
#32683=CARTESIAN_POINT('Ctrl Pts',(-69.2851779860668,6.93169994506568,0.162059461329396));
#32684=CARTESIAN_POINT('Ctrl Pts',(-69.3182072478057,6.95859609743217,-0.988358146812281));
#32685=CARTESIAN_POINT('Ctrl Pts',(-69.3512365095445,6.69292493701634,-2.14561582326041));
#32686=CARTESIAN_POINT('Ctrl Pts',(-69.3842657712834,6.16696379854899,-3.16911421454174));
#32687=CARTESIAN_POINT('Ctrl Pts',(-69.4172950330223,5.64100266008167,-4.19261260582304));
#32688=CARTESIAN_POINT('Ctrl Pts',(-69.4503242947612,4.85475154356283,-5.08235171193756));
#32689=CARTESIAN_POINT('Ctrl Pts',(-69.4833535565001,3.90373489519033,-5.73023396254479));
#32690=CARTESIAN_POINT('Ctrl Pts',(-69.516382818239,2.95271824681782,-6.37811621315202));
#32691=CARTESIAN_POINT('Ctrl Pts',(-69.5494120799779,1.83693606659164,-6.78414160825195));
#32692=CARTESIAN_POINT('Ctrl Pts',(-69.5824413417168,0.691948702350952,
-6.89898067766109));
#32693=CARTESIAN_POINT('Ctrl Pts',(-69.6154706034557,-0.453038661889801,
-7.01381974707024));
#32694=CARTESIAN_POINT('Ctrl Pts',(-69.6484998651946,-1.62723121014506,
-6.83747249078857));
#32695=CARTESIAN_POINT('Ctrl Pts',(-69.6815291269334,-2.68797211109765,
-6.39136396455314));
#32696=CARTESIAN_POINT('Ctrl Pts',(-69.7145583886723,-3.74871301205017,
-5.94525543831773));
#32697=CARTESIAN_POINT('Ctrl Pts',(-69.7475876504112,-4.69600226570003,
-5.2293856421286));
#32698=CARTESIAN_POINT('Ctrl Pts',(-69.7806169121501,-5.41475032947817,
-4.33072814510943));
#32699=CARTESIAN_POINT('Ctrl Pts',(-69.813646173889,-6.13349839325633,-3.43207064809025));
#32700=CARTESIAN_POINT('Ctrl Pts',(-69.8466754356279,-6.62370526716277,
-2.35062545024102));
#32701=CARTESIAN_POINT('Ctrl Pts',(-69.8797046973668,-6.82581397357457,
-1.21778117721575));
#32702=CARTESIAN_POINT('Ctrl Pts',(-69.8914125770424,-6.89745543001326,
-0.816221961491587));
#32703=CARTESIAN_POINT('Ctrl Pts',(-69.9031204567181,-6.9328976622069,-0.408204507367422));
#32704=CARTESIAN_POINT('Ctrl Pts',(-69.9148283363937,-6.93260597399068,
-0.000136960269141728));
#32705=CARTESIAN_POINT('Ctrl Pts',(-70.0941716636062,-6.93269186048085,
-0.000156184372951973));
#32706=CARTESIAN_POINT('Ctrl Pts',(-70.0834969937484,-6.93300050707366,
-0.372198922151348));
#32707=CARTESIAN_POINT('Ctrl Pts',(-70.0728223238906,-6.90356541513618,
-0.744193308803663));
#32708=CARTESIAN_POINT('Ctrl Pts',(-70.0621476540327,-6.84395829026021,
-1.11128850816545));
#32709=CARTESIAN_POINT('Ctrl Pts',(-70.0291183922938,-6.65952360935215,
-2.24714409754429));
#32710=CARTESIAN_POINT('Ctrl Pts',(-69.9960891305549,-6.18622494101828,
-3.33609536401019));
#32711=CARTESIAN_POINT('Ctrl Pts',(-69.963059868816,-5.48156502481484,-4.2458417429208));
#32712=CARTESIAN_POINT('Ctrl Pts',(-69.9300306070771,-4.77690510861136,
-5.15558812183147));
#32713=CARTESIAN_POINT('Ctrl Pts',(-69.8970013453382,-3.84088394453828,
-5.88612961318685));
#32714=CARTESIAN_POINT('Ctrl Pts',(-69.8639720835994,-2.78722207486187,
-6.34871013140502));
#32715=CARTESIAN_POINT('Ctrl Pts',(-69.8309428218605,-1.73356020518553,
-6.81129064962317));
#32716=CARTESIAN_POINT('Ctrl Pts',(-69.7979135601216,-0.562257629905866,
-7.00591019470415));
#32717=CARTESIAN_POINT('Ctrl Pts',(-69.7648842983827,0.584379932761237,
-6.90892374551841));
#32718=CARTESIAN_POINT('Ctrl Pts',(-69.7318550366438,1.73101749542841,-6.81193729633265));
#32719=CARTESIAN_POINT('Ctrl Pts',(-69.6988257749049,2.85299004548303,-6.42334485288014));
#32720=CARTESIAN_POINT('Ctrl Pts',(-69.665796513166,3.81398514502586,-5.79035789401002));
#32721=CARTESIAN_POINT('Ctrl Pts',(-69.6327672514271,4.77498024456863,-5.15737093513994));
#32722=CARTESIAN_POINT('Ctrl Pts',(-69.5997379896882,5.57499789359964,-4.27998946085228));
#32723=CARTESIAN_POINT('Ctrl Pts',(-69.5667087279493,6.11684110089434,-3.26480966881867));
#32724=CARTESIAN_POINT('Ctrl Pts',(-69.5336794662104,6.65868430818905,-2.24962987678502));
#32725=CARTESIAN_POINT('Ctrl Pts',(-69.5006502044716,6.94235307374744,-1.0966517670055));
#32726=CARTESIAN_POINT('Ctrl Pts',(-69.4676209427327,6.9333834697424,0.0540452468295327));
#32727=CARTESIAN_POINT('Ctrl Pts',(-69.4345916809938,6.92441386573736,1.2047422606645));
#32728=CARTESIAN_POINT('Ctrl Pts',(-69.4015624192549,6.62280589216886,2.353158178555));
#32729=CARTESIAN_POINT('Ctrl Pts',(-69.368533157516,6.06520297508595,3.35976786373859));
#32730=CARTESIAN_POINT('Ctrl Pts',(-69.3355038957771,5.50760005800299,4.36637754892227));
#32731=CARTESIAN_POINT('Ctrl Pts',(-69.3024746340382,4.69400219740564,5.23118100139905));
#32732=CARTESIAN_POINT('Ctrl Pts',(-69.2694453722993,3.7232562927498,5.84911017212886));
#32733=CARTESIAN_POINT('Ctrl Pts',(-69.2364161105604,2.75251038809402,6.46703934285863));
#32734=CARTESIAN_POINT('Ctrl Pts',(-69.2033868488216,1.6246164393798,6.83809423184139));
#32735=CARTESIAN_POINT('Ctrl Pts',(-69.1703575870827,0.476606296302118,
6.91719406013208));
#32736=CARTESIAN_POINT('Ctrl Pts',(-69.1373283253438,-0.671403846775601,
6.99629388842278));
#32737=CARTESIAN_POINT('Ctrl Pts',(-69.1042990636049,-1.83953018421682,
6.78343865602139));
#32738=CARTESIAN_POINT('Ctrl Pts',(-69.0712698018661,-2.88585289024383,
6.30448890260542));
#32739=CARTESIAN_POINT('Ctrl Pts',(-69.0382405401271,-3.93217559627087,
5.82553914918944));
#32740=CARTESIAN_POINT('Ctrl Pts',(-69.0052112783882,-4.85669467088372,
5.08049487475885));
#32741=CARTESIAN_POINT('Ctrl Pts',(-68.9721820166493,-5.54708700159773,
4.1598741596237));
#32742=CARTESIAN_POINT('Ctrl Pts',(-68.9391527549104,-6.23747933231171,
3.2392534444886));
#32743=CARTESIAN_POINT('Ctrl Pts',(-68.9061234931715,-6.69374491912688,
2.14305628864894));
#32744=CARTESIAN_POINT('Ctrl Pts',(-68.8730942314327,-6.86045043217612,
1.00446358563143));
#32745=CARTESIAN_POINT('Ctrl Pts',(-68.8634533754906,-6.90910982543695,
0.672121666719093));
#32746=CARTESIAN_POINT('Ctrl Pts',(-68.8538125195484,-6.93309904925115,
0.33616769826188));
#32747=CARTESIAN_POINT('Ctrl Pts',(-68.8441716636063,-6.93278929229388,
0.000169878797845651));
#32748=CARTESIAN_POINT('Origin',(-87.75,0.,0.));
#32749=CARTESIAN_POINT('',(-67.4148283363937,-6.93337279743796,-0.000131731084783704));
#32750=CARTESIAN_POINT('',(-67.5941716636062,-6.9334612849287,-0.000104716709421631));
#32751=CARTESIAN_POINT('',(-87.75,-6.933,-8.4904762584886E-16));
#32752=CARTESIAN_POINT('Ctrl Pts',(-67.4148283363937,-6.93337279743796,
-0.000131731084783704));
#32753=CARTESIAN_POINT('Ctrl Pts',(-67.4437515083181,-6.93249558801675,
1.00763853557119));
#32754=CARTESIAN_POINT('Ctrl Pts',(-67.4726746802424,-6.71019820674341,
2.01578265024431));
#32755=CARTESIAN_POINT('Ctrl Pts',(-67.5015978521667,-6.28450099732112,
2.92912494075186));
#32756=CARTESIAN_POINT('Ctrl Pts',(-67.5346271139056,-5.79836951117891,
3.97213023938542));
#32757=CARTESIAN_POINT('Ctrl Pts',(-67.5676563756445,-5.04698736297379,
4.89150590247039));
#32758=CARTESIAN_POINT('Ctrl Pts',(-67.6006856373834,-4.1216423195172,5.57555315608241));
#32759=CARTESIAN_POINT('Ctrl Pts',(-67.6337148991223,-3.1962972760606,6.25960040969444));
#32760=CARTESIAN_POINT('Ctrl Pts',(-67.6667441608612,-2.09698933735247,
6.70831925383352));
#32761=CARTESIAN_POINT('Ctrl Pts',(-67.6997734226,-0.957277496925685,6.86719351183532));
#32762=CARTESIAN_POINT('Ctrl Pts',(-67.7328026843389,0.182434343501171,
7.02606776983713));
#32763=CARTESIAN_POINT('Ctrl Pts',(-67.7658319460778,1.36255008564665,6.89509744170168));
#32764=CARTESIAN_POINT('Ctrl Pts',(-67.7988612078167,2.43969334714329,6.49019444427998));
#32765=CARTESIAN_POINT('Ctrl Pts',(-67.8318904695556,3.51683660863984,6.08529144685832));
#32766=CARTESIAN_POINT('Ctrl Pts',(-67.8649197312945,4.49100738948749,5.40645578015041));
#32767=CARTESIAN_POINT('Ctrl Pts',(-67.8979489930334,5.24385017583266,4.53616167136526));
#32768=CARTESIAN_POINT('Ctrl Pts',(-67.9309782547723,5.99669296217787,3.66586756258006));
#32769=CARTESIAN_POINT('Ctrl Pts',(-67.9640075165112,6.52820775402063,2.60411501171758));
#32770=CARTESIAN_POINT('Ctrl Pts',(-67.9970367782501,6.7738189469558,1.47990008199233));
#32771=CARTESIAN_POINT('Ctrl Pts',(-68.0300660399889,7.01943013989096,0.355685152267077));
#32772=CARTESIAN_POINT('Ctrl Pts',(-68.0630953017278,6.97913773391853,-0.830992156320916));
#32773=CARTESIAN_POINT('Ctrl Pts',(-68.0961245634667,6.65783698737675,-1.93595817837977));
#32774=CARTESIAN_POINT('Ctrl Pts',(-68.1291538252056,6.33653624083498,-3.04092420043856));
#32775=CARTESIAN_POINT('Ctrl Pts',(-68.1621830869445,5.73422715372385,-4.06417893596827));
#32776=CARTESIAN_POINT('Ctrl Pts',(-68.1952123486834,4.92408640515072,-4.88140353361028));
#32777=CARTESIAN_POINT('Ctrl Pts',(-68.2282416104223,4.11394565657754,-5.69862813125233));
#32778=CARTESIAN_POINT('Ctrl Pts',(-68.2612708721612,3.0959732465424,-6.30982259100668));
#32779=CARTESIAN_POINT('Ctrl Pts',(-68.2943001339001,1.99384626352711,-6.64073071896694));
#32780=CARTESIAN_POINT('Ctrl Pts',(-68.327329395639,0.891719280511826,-6.9716388469272));
#32781=CARTESIAN_POINT('Ctrl Pts',(-68.3603586573778,-0.294562275483611,
-7.0222606430933));
#32782=CARTESIAN_POINT('Ctrl Pts',(-68.3933879191167,-1.4208728354367,-6.7864458872314));
#32783=CARTESIAN_POINT('Ctrl Pts',(-68.4264171808556,-2.54718339538978,
-6.55063113136949));
#32784=CARTESIAN_POINT('Ctrl Pts',(-68.4594464425945,-3.61352295930058,
-6.02837982347959));
#32785=CARTESIAN_POINT('Ctrl Pts',(-68.4924757043334,-4.49033813929784,
-5.28314213255427));
#32786=CARTESIAN_POINT('Ctrl Pts',(-68.5255049660723,-5.3671533192951,-4.53790444162894));
#32787=CARTESIAN_POINT('Ctrl Pts',(-68.5585342278112,-6.05444411537879,
-3.56968036766821));
#32788=CARTESIAN_POINT('Ctrl Pts',(-68.5915634895501,-6.46870912257745,
-2.49610289953149));
#32789=CARTESIAN_POINT('Ctrl Pts',(-68.6159851051646,-6.77501390311845,
-1.70230688717924));
#32790=CARTESIAN_POINT('Ctrl Pts',(-68.6404067207792,-6.93205480584839,
-0.850913912212287));
#32791=CARTESIAN_POINT('Ctrl Pts',(-68.6648283363937,-6.93289541479494,
0.00017741184833428));
#32792=CARTESIAN_POINT('Ctrl Pts',(-68.8441716636063,-6.93278929229388,
0.000169878797845651));
#32793=CARTESIAN_POINT('Ctrl Pts',(-68.8207832578095,-6.9320378318988,-0.814950002218331));
#32794=CARTESIAN_POINT('Ctrl Pts',(-68.7973948520128,-6.78827910312482,
-1.63032796042549));
#32795=CARTESIAN_POINT('Ctrl Pts',(-68.774006446216,-6.50681278781459,-2.39501869962106));
#32796=CARTESIAN_POINT('Ctrl Pts',(-68.7409771844771,-6.1093241911205,-3.4749200316607));
#32797=CARTESIAN_POINT('Ctrl Pts',(-68.7079479227382,-5.43720155844903,
-4.45373444554453));
#32798=CARTESIAN_POINT('Ctrl Pts',(-68.6749186609993,-4.57210346034106,
-5.21254229480466));
#32799=CARTESIAN_POINT('Ctrl Pts',(-68.6418893992604,-3.70700536223314,
-5.97135014406476));
#32800=CARTESIAN_POINT('Ctrl Pts',(-68.6088601375215,-2.64893179868877,
-6.51015142870117));
#32801=CARTESIAN_POINT('Ctrl Pts',(-68.5758308757826,-1.52643189234264,
-6.76348526318229));
#32802=CARTESIAN_POINT('Ctrl Pts',(-68.5428016140437,-0.403931985996506,
-7.01681909766341));
#32803=CARTESIAN_POINT('Ctrl Pts',(-68.5097723523049,0.782994263151457,
-6.98468548198923));
#32804=CARTESIAN_POINT('Ctrl Pts',(-68.476743090566,1.89014296115799,-6.67098844351297));
#32805=CARTESIAN_POINT('Ctrl Pts',(-68.4437138288271,2.99729165916456,-6.3572914050367));
#32806=CARTESIAN_POINT('Ctrl Pts',(-68.4106845670882,4.0246628060297,-5.7620309437584));
#32807=CARTESIAN_POINT('Ctrl Pts',(-68.3776553053493,4.84743742496519,-4.95752737142637));
#32808=CARTESIAN_POINT('Ctrl Pts',(-68.3446260436104,5.67021204390068,-4.15302379909433));
#32809=CARTESIAN_POINT('Ctrl Pts',(-68.3115967818716,6.28839013490641,-3.13927711570861));
#32810=CARTESIAN_POINT('Ctrl Pts',(-68.2785675201327,6.62686704182652,-2.03945101360489));
#32811=CARTESIAN_POINT('Ctrl Pts',(-68.2455382583938,6.96534394874662,-0.939624911501181));
#32812=CARTESIAN_POINT('Ctrl Pts',(-68.2125089966549,7.02411967158108,0.246280609320601));
#32813=CARTESIAN_POINT('Ctrl Pts',(-68.179479734916,6.7960533385008,1.3741856670747));
#32814=CARTESIAN_POINT('Ctrl Pts',(-68.1464504731771,6.56798700542051,2.5020907248288));
#32815=CARTESIAN_POINT('Ctrl Pts',(-68.1134212114382,6.05307861642555,3.57199531951521));
#32816=CARTESIAN_POINT('Ctrl Pts',(-68.0803919496993,5.31388622430591,4.45391293391699));
#32817=CARTESIAN_POINT('Ctrl Pts',(-68.0473626879604,4.57469383218627,5.33583054831877));
#32818=CARTESIAN_POINT('Ctrl Pts',(-68.0143334262215,3.61121743694198,6.02976118243583));
#32819=CARTESIAN_POINT('Ctrl Pts',(-67.9813041644826,2.54051321418835,6.4513967350567));
#32820=CARTESIAN_POINT('Ctrl Pts',(-67.9482749027437,1.46980899143475,6.87303228767757));
#32821=CARTESIAN_POINT('Ctrl Pts',(-67.9152456410048,0.291876941171729,
7.02237275880227));
#32822=CARTESIAN_POINT('Ctrl Pts',(-67.882216379266,-0.8501717790824,6.88127424103013));
#32823=CARTESIAN_POINT('Ctrl Pts',(-67.8491871175271,-1.99222049933653,
6.74017572325799));
#32824=CARTESIAN_POINT('Ctrl Pts',(-67.8161578557882,-3.09838588958184,
6.30863821658903));
#32825=CARTESIAN_POINT('Ctrl Pts',(-67.7831285940493,-4.0342759816279,5.63909075269439));
#32826=CARTESIAN_POINT('Ctrl Pts',(-67.7500993323104,-4.97016607367399,
4.96954328879973));
#32827=CARTESIAN_POINT('Ctrl Pts',(-67.7170700705715,-5.73578086752079,
4.06198586767938));
#32828=CARTESIAN_POINT('Ctrl Pts',(-67.6840408088326,-6.23810309398541,
3.02668086153105));
#32829=CARTESIAN_POINT('Ctrl Pts',(-67.6540844270905,-6.69369173209929,
2.08769553909514));
#32830=CARTESIAN_POINT('Ctrl Pts',(-67.6241280453483,-6.93269975711327,
1.04362692257891));
#32831=CARTESIAN_POINT('Ctrl Pts',(-67.5941716636062,-6.9334612849287,-0.000104716709421631));
#32832=CARTESIAN_POINT('Origin',(-88.8777445817596,0.,0.));
#32833=CARTESIAN_POINT('',(-67.0027445817596,-6.21958441806809,-0.000118169414145055));
#32834=CARTESIAN_POINT('',(-66.7562554182403,-6.21873914925953,1.11460959661969E-5));
#32835=CARTESIAN_POINT('',(-88.8777445817596,-6.21925,-6.18233832090354E-13));
#32836=CARTESIAN_POINT('',(-66.51072,4.88120307569155,-3.85434375923658));
#32837=CARTESIAN_POINT('Ctrl Pts',(-67.0027445817596,-6.21958441806809,
-0.000118169414144789));
#32838=CARTESIAN_POINT('Ctrl Pts',(-66.9986384919451,-6.21969613078843,
-0.128457828390552));
#32839=CARTESIAN_POINT('Ctrl Pts',(-66.9615031403916,-6.18450232485475,
-1.28909667822277));
#32840=CARTESIAN_POINT('Ctrl Pts',(-66.8913385270993,-5.49220424623203,
-3.44324500874027));
#32841=CARTESIAN_POINT('Ctrl Pts',(-66.7922507418826,-3.17999782273006,
-5.64870137951734));
#32842=CARTESIAN_POINT('Ctrl Pts',(-66.693162956666,-0.0950831417423778,
-6.481612708114));
#32843=CARTESIAN_POINT('Ctrl Pts',(-66.5993193760384,2.84842541282538,-5.77881590697225));
#32844=CARTESIAN_POINT('Ctrl Pts',(-66.5385050571497,4.34230708651471,-4.53542015418599));
#32845=CARTESIAN_POINT('Ctrl Pts',(-66.51072,4.88120307569155,-3.85434375923658));
#32846=CARTESIAN_POINT('',(-66.51072,-2.0540967914958,-5.87024334535347));
#32847=CARTESIAN_POINT('Origin',(-66.51072,0.,0.));
#32848=CARTESIAN_POINT('Ctrl Pts',(-66.7562554182403,-6.21873914925953,
1.11460959660928E-5));
#32849=CARTESIAN_POINT('Ctrl Pts',(-66.7404688023046,-6.2188028846916,-0.493595494752219));
#32850=CARTESIAN_POINT('Ctrl Pts',(-66.6916529246301,-6.0392566751686,-2.01992285710156));
#32851=CARTESIAN_POINT('Ctrl Pts',(-66.6098077852167,-4.80376045256683,
-4.35266662668044));
#32852=CARTESIAN_POINT('Ctrl Pts',(-66.5437492617389,-3.02869324528072,
-5.529215668825));
#32853=CARTESIAN_POINT('Ctrl Pts',(-66.51072,-2.05409679149563,-5.87024334535353));
#32854=CARTESIAN_POINT('Origin',(-88.8777445817596,0.,0.));
#32855=CARTESIAN_POINT('',(-68.2527445817596,-6.21915618180635,0.000159147358266852));
#32856=CARTESIAN_POINT('',(-68.0062554182403,-6.21966379580164,-9.39361602741995E-5));
#32857=CARTESIAN_POINT('',(-88.8777445817596,-6.21925,-6.18233832090354E-13));
#32858=CARTESIAN_POINT('Ctrl Pts',(-68.2527445817596,-6.21915618180635,
0.000159147358266866));
#32859=CARTESIAN_POINT('Ctrl Pts',(-68.2283229661451,-6.21840211326586,
-0.763312613374919));
#32860=CARTESIAN_POINT('Ctrl Pts',(-68.1708720887917,-5.88700259581307,
-2.55998606699028));
#32861=CARTESIAN_POINT('Ctrl Pts',(-68.0803919496993,-4.1980722627264,-4.9392744512594));
#32862=CARTESIAN_POINT('Ctrl Pts',(-67.9813041644827,-1.3283914609729,-6.34473158955201));
#32863=CARTESIAN_POINT('Ctrl Pts',(-67.882216379266,1.864071354745,-6.20850069132352));
#32864=CARTESIAN_POINT('Ctrl Pts',(-67.7831285940493,4.60358884116279,-4.5636840994466));
#32865=CARTESIAN_POINT('Ctrl Pts',(-67.6840408088326,6.22449355341539,-1.80995107740288));
#32866=CARTESIAN_POINT('Ctrl Pts',(-67.584953023616,6.33292650272045,1.38357676830714));
#32867=CARTESIAN_POINT('Ctrl Pts',(-67.4858652383993,4.90253993016824,4.24091322523118));
#32868=CARTESIAN_POINT('Ctrl Pts',(-67.3867774531826,2.2808992426794,6.06776251998367));
#32869=CARTESIAN_POINT('Ctrl Pts',(-67.287689667966,-0.894970436826739,
6.42022345172595));
#32870=CARTESIAN_POINT('Ctrl Pts',(-67.1886018827492,-3.8533741139406,5.21265327802973));
#32871=CARTESIAN_POINT('Ctrl Pts',(-67.0936201873472,-5.79166403763128,
2.84100179801934));
#32872=CARTESIAN_POINT('Ctrl Pts',(-67.031667753684,-6.21879751705943,0.903902489881935));
#32873=CARTESIAN_POINT('Ctrl Pts',(-67.0027445817596,-6.21958441806809,
-0.000118169414144789));
#32874=CARTESIAN_POINT('Ctrl Pts',(-68.0062554182403,-6.21966379580164,
-9.39361602741995E-5));
#32875=CARTESIAN_POINT('Ctrl Pts',(-68.0031825382435,-6.21973387011156,
-0.0961360936374352));
#32876=CARTESIAN_POINT('Ctrl Pts',(-67.9670803965079,-6.19413651603434,
-1.22446285990289));
#32877=CARTESIAN_POINT('Ctrl Pts',(-67.8979489930334,-5.54518383041795,
-3.35725764403967));
#32878=CARTESIAN_POINT('Ctrl Pts',(-67.7988612078167,-3.26761528590833,
-5.59847600248888));
#32879=CARTESIAN_POINT('Ctrl Pts',(-67.6997734226,-0.196058420264034,-6.47933655521552));
#32880=CARTESIAN_POINT('Ctrl Pts',(-67.6006856373834,2.92313831475997,-5.78580232210167));
#32881=CARTESIAN_POINT('Ctrl Pts',(-67.5015978521667,5.33204969326613,-3.6863915925369));
#32882=CARTESIAN_POINT('Ctrl Pts',(-67.4025100669501,6.44534250489529,-0.691237361863573));
#32883=CARTESIAN_POINT('Ctrl Pts',(-67.3034222817333,5.99249846114462,2.47188303450135));
#32884=CARTESIAN_POINT('Ctrl Pts',(-67.2043344965166,4.08355785429189,5.03435879238504));
#32885=CARTESIAN_POINT('Ctrl Pts',(-67.1052467113001,1.18235847344737,6.37356827685746));
#32886=CARTESIAN_POINT('Ctrl Pts',(-67.0061589260833,-2.0061249511844,6.16404616060605));
#32887=CARTESIAN_POINT('Ctrl Pts',(-66.9070711408667,-4.70717390764343,
4.4568144926439));
#32888=CARTESIAN_POINT('Ctrl Pts',(-66.8237699715857,-6.01628953715405,
2.11103777105964));
#32889=CARTESIAN_POINT('Ctrl Pts',(-66.7734980640435,-6.21866953538632,
0.539144074200984));
#32890=CARTESIAN_POINT('Ctrl Pts',(-66.7562554182403,-6.21873914925953,
1.11460959660928E-5));
#32891=CARTESIAN_POINT('Origin',(-88.8777445817596,0.,0.));
#32892=CARTESIAN_POINT('',(-69.5027445817596,-6.21889653883479,-0.000122860255921536));
#32893=CARTESIAN_POINT('',(-69.2562554182403,-6.2190609845808,0.000152389832417943));
#32894=CARTESIAN_POINT('',(-88.8777445817596,-6.21925,-6.18233832090354E-13));
#32895=CARTESIAN_POINT('Ctrl Pts',(-69.5027445817596,-6.21889653883479,
-0.000122860255920947));
#32896=CARTESIAN_POINT('Ctrl Pts',(-69.491036702084,-6.21915819784801,-0.366179991698439));
#32897=CARTESIAN_POINT('Ctrl Pts',(-69.4462995606695,-6.09767174240742,
-1.76475426852759));
#32898=CARTESIAN_POINT('Ctrl Pts',(-69.368533157516,-5.062316570275,-4.04885091949506));
#32899=CARTESIAN_POINT('Ctrl Pts',(-69.2694453722994,-2.5130181320396,-5.97536464946014));
#32900=CARTESIAN_POINT('Ctrl Pts',(-69.1703575870826,0.646911338205425,
-6.44994174752579));
#32901=CARTESIAN_POINT('Ctrl Pts',(-69.0712698018661,3.64964968713308,-5.35726609262518));
#32902=CARTESIAN_POINT('Ctrl Pts',(-68.9721820166493,5.76557017887249,-2.96284379245084));
#32903=CARTESIAN_POINT('Ctrl Pts',(-68.8730942314327,6.48053139238009,0.151511380309847));
#32904=CARTESIAN_POINT('Ctrl Pts',(-68.774006446216,5.62080696329017,3.22905123951376));
#32905=CARTESIAN_POINT('Ctrl Pts',(-68.6749186609993,3.39529885244121,5.52197324591022));
#32906=CARTESIAN_POINT('Ctrl Pts',(-68.5758308757827,0.344776860533978,
6.47312689065817));
#32907=CARTESIAN_POINT('Ctrl Pts',(-68.476743090566,-2.78952146684973,5.85139409129237));
#32908=CARTESIAN_POINT('Ctrl Pts',(-68.3776553053494,-5.24600201399085,
3.80784790870568));
#32909=CARTESIAN_POINT('Ctrl Pts',(-68.3029891357472,-6.13650745964284,
1.5707483996713));
#32910=CARTESIAN_POINT('Ctrl Pts',(-68.2613522278839,-6.21942196091174,
0.269252513090079));
#32911=CARTESIAN_POINT('Ctrl Pts',(-68.2527445817596,-6.21915618180635,
0.000159147358266866));
#32912=CARTESIAN_POINT('Ctrl Pts',(-69.2562554182403,-6.2190609845808,0.00015238983241829));
#32913=CARTESIAN_POINT('Ctrl Pts',(-69.2328670124436,-6.21838688677859,
-0.731051175724831));
#32914=CARTESIAN_POINT('Ctrl Pts',(-69.176449344908,-5.90731157488004,-2.49542371037046));
#32915=CARTESIAN_POINT('Ctrl Pts',(-69.0870024156334,-4.27451566553321,
-4.87326979575939));
#32916=CARTESIAN_POINT('Ctrl Pts',(-68.9879146304167,-1.42707991907126,
-6.32326542080269));
#32917=CARTESIAN_POINT('Ctrl Pts',(-68.8888268452001,1.76711786327968,-6.23678900830517));
#32918=CARTESIAN_POINT('Ctrl Pts',(-68.7897390599834,4.5319287698749,-4.63485321262994));
#32919=CARTESIAN_POINT('Ctrl Pts',(-68.6906512747668,6.19553936809527,-1.90670779478191));
#32920=CARTESIAN_POINT('Ctrl Pts',(-68.5915634895501,6.35371371436876,1.28474305349599));
#32921=CARTESIAN_POINT('Ctrl Pts',(-68.4924757043333,4.96801747972696,4.16401789144663));
#32922=CARTESIAN_POINT('Ctrl Pts',(-68.3933879191168,2.37515699892946,6.03149002309199));
#32923=CARTESIAN_POINT('Ctrl Pts',(-68.2943001338999,-0.794836035946308,
6.43338778381987));
#32924=CARTESIAN_POINT('Ctrl Pts',(-68.1952123486834,-3.77169415073787,
5.27205518392761));
#32925=CARTESIAN_POINT('Ctrl Pts',(-68.0991974434635,-5.76818315324227,
2.9054232627965));
#32926=CARTESIAN_POINT('Ctrl Pts',(-68.0362117999824,-6.21898066701678,
0.936185884645314));
#32927=CARTESIAN_POINT('Ctrl Pts',(-68.0062554182403,-6.21966379580164,
-9.39361602741995E-5));
#32928=CARTESIAN_POINT('Origin',(-88.8777445817596,0.,0.));
#32929=CARTESIAN_POINT('',(-70.7527445817596,-6.2197684298873,3.29288831883953E-5));
#32930=CARTESIAN_POINT('',(-70.5062554182403,-6.2189735833399,-0.000140105245378663));
#32931=CARTESIAN_POINT('',(-88.8777445817596,-6.21925,-6.18233832090354E-13));
#32932=CARTESIAN_POINT('Ctrl Pts',(-70.7527445817596,-6.2197684298873,3.29288831883321E-5));
#32933=CARTESIAN_POINT('Ctrl Pts',(-70.720721176284,-6.2194747868859,-1.00080233535455));
#32934=CARTESIAN_POINT('Ctrl Pts',(-70.6556685090695,-5.71938164108245,
-3.03419205074321));
#32935=CARTESIAN_POINT('Ctrl Pts',(-70.5575865801161,-3.6055588131454,-5.38703893348903));
#32936=CARTESIAN_POINT('Ctrl Pts',(-70.4584987948994,-0.593953827191011,
-6.45503382463191));
#32937=CARTESIAN_POINT('Ctrl Pts',(-70.3594110096827,2.56197428713231,-5.95453865366998));
#32938=CARTESIAN_POINT('Ctrl Pts',(-70.2603232244661,5.09537565443828,-4.00716729949408));
#32939=CARTESIAN_POINT('Ctrl Pts',(-70.1612354392494,6.39066637913534,-1.08610591406471));
#32940=CARTESIAN_POINT('Ctrl Pts',(-70.0621476540327,6.13310750176651,2.09886521667122));
#32941=CARTESIAN_POINT('Ctrl Pts',(-69.9630598688161,4.38528251151797,4.77383913848715));
#32942=CARTESIAN_POINT('Ctrl Pts',(-69.8639720835993,1.57189036458139,6.28883164886079));
#32943=CARTESIAN_POINT('Ctrl Pts',(-69.7648842983828,-1.62345089099596,
6.27571908473456));
#32944=CARTESIAN_POINT('Ctrl Pts',(-69.665796513166,-4.42431449424472,4.73768763026785));
#32945=CARTESIAN_POINT('Ctrl Pts',(-69.578416607625,-5.94621050523724,2.36620931821423));
#32946=CARTESIAN_POINT('Ctrl Pts',(-69.5240659638229,-6.21842002797665,
0.666508858953097));
#32947=CARTESIAN_POINT('Ctrl Pts',(-69.5027445817596,-6.21889653883479,
-0.000122860255920947));
#32948=CARTESIAN_POINT('Ctrl Pts',(-70.5062554182403,-6.2189735833399,-0.000140105245378629));
#32949=CARTESIAN_POINT('Ctrl Pts',(-70.4955807483825,-6.21925045487056,
-0.33388116927637));
#32950=CARTESIAN_POINT('Ctrl Pts',(-70.4518768167858,-6.11114483612411,
-1.70009682182616));
#32951=CARTESIAN_POINT('Ctrl Pts',(-70.3751436234501,-5.12478244935701,
-3.96948957977628));
#32952=CARTESIAN_POINT('Ctrl Pts',(-70.2760558382335,-2.60580814184455,
-5.93548705710717));
#32953=CARTESIAN_POINT('Ctrl Pts',(-70.1769680530168,0.546343974688648,
-6.45923764375577));
#32954=CARTESIAN_POINT('Ctrl Pts',(-70.0778802678002,3.56574154367478,-5.4134766944083));
#32955=CARTESIAN_POINT('Ctrl Pts',(-69.9787924825834,5.71870985338321,-3.05231064769102));
#32956=CARTESIAN_POINT('Ctrl Pts',(-69.8797046973668,6.48210534027158,0.0505275648778713));
#32957=CARTESIAN_POINT('Ctrl Pts',(-69.7806169121501,5.67043273550486,3.14108823010512));
#32958=CARTESIAN_POINT('Ctrl Pts',(-69.6815291269334,3.4809180256302,5.46840492063578));
#32959=CARTESIAN_POINT('Ctrl Pts',(-69.5824413417167,0.445585078619785,
6.46696966243845));
#32960=CARTESIAN_POINT('Ctrl Pts',(-69.4833535565002,-2.69801930222453,
5.89414408731404));
#32961=CARTESIAN_POINT('Ctrl Pts',(-69.3842657712834,-5.18603974998983,
3.88911743056271));
#32962=CARTESIAN_POINT('Ctrl Pts',(-69.3085663918635,-6.12409405569377,
1.63540272655992));
#32963=CARTESIAN_POINT('Ctrl Pts',(-69.2658962741825,-6.21933885216436,
0.301559347672218));
#32964=CARTESIAN_POINT('Ctrl Pts',(-69.2562554182403,-6.2190609845808,0.00015238983241829));
#32965=CARTESIAN_POINT('Origin',(-88.8777445817596,0.,0.));
#32966=CARTESIAN_POINT('',(-72.0027445817596,-6.21878348465591,7.77291339505116E-5));
#32967=CARTESIAN_POINT('',(-71.7562554182403,-6.21972691674719,6.50263875292059E-5));
#32968=CARTESIAN_POINT('',(-88.8777445817596,-6.21925,-6.18233832090354E-13));
#32969=CARTESIAN_POINT('Ctrl Pts',(-72.0027445817596,-6.21878348465591,
7.77291339506408E-5));
#32970=CARTESIAN_POINT('Ctrl Pts',(-71.9834349122229,-6.21851690018761,
-0.603687467000913));
#32971=CARTESIAN_POINT('Ctrl Pts',(-71.9310959809473,-5.98187890039571,
-2.24039980722369));
#32972=CARTESIAN_POINT('Ctrl Pts',(-71.8457277879328,-4.56597889785132,
-4.60131280509741));
#32973=CARTESIAN_POINT('Ctrl Pts',(-71.7466400027161,-1.81305439576657,
-6.22359032905994));
#32974=CARTESIAN_POINT('Ctrl Pts',(-71.6475522174995,1.38041896772984,-6.33361557875979));
#32975=CARTESIAN_POINT('Ctrl Pts',(-71.5484644322828,4.238468305381,-4.90465383592539));
#32976=CARTESIAN_POINT('Ctrl Pts',(-71.4493766470661,6.06662444709443,-2.28392439539779));
#32977=CARTESIAN_POINT('Ctrl Pts',(-71.3502888618495,6.42066900174233,0.89176925044665));
#32978=CARTESIAN_POINT('Ctrl Pts',(-71.2512010766327,5.2145737035411,3.8507744566924));
#32979=CARTESIAN_POINT('Ctrl Pts',(-71.1521132914161,2.7414041723735,5.87409107774727));
#32980=CARTESIAN_POINT('Ctrl Pts',(-71.0530255061994,-0.397891256411005,
6.47007924016768));
#32981=CARTESIAN_POINT('Ctrl Pts',(-70.9539377209828,-3.44050423574074,
5.49392149833132));
#32982=CARTESIAN_POINT('Ctrl Pts',(-70.854849935766,-5.64711900824516,3.18281160810583));
#32983=CARTESIAN_POINT('Ctrl Pts',(-70.787785556025,-6.21188125558683,1.09517235362907));
#32984=CARTESIAN_POINT('Ctrl Pts',(-70.7537504380229,-6.21977765322404,
0.0314691988263317));
#32985=CARTESIAN_POINT('Ctrl Pts',(-70.7527445817596,-6.2197684298873,3.29288831883321E-5));
#32986=CARTESIAN_POINT('Ctrl Pts',(-71.7562554182403,-6.21972691674719,
6.50263875293274E-5));
#32987=CARTESIAN_POINT('Ctrl Pts',(-71.7252652225825,-6.21920548964646,
-0.968497879647463));
#32988=CARTESIAN_POINT('Ctrl Pts',(-71.6612457651859,-5.74408110420307,
-2.96984607376813));
#32989=CARTESIAN_POINT('Ctrl Pts',(-71.5641970460501,-3.68905021568418,
-5.33021117624344));
#32990=CARTESIAN_POINT('Ctrl Pts',(-71.4651092608335,-0.694449915114697,
-6.44499666350474));
#32991=CARTESIAN_POINT('Ctrl Pts',(-71.3660214756168,2.46889276854356,-5.99373098951091));
#32992=CARTESIAN_POINT('Ctrl Pts',(-71.2669336904001,5.03232631507441,-4.0860658995909));
#32993=CARTESIAN_POINT('Ctrl Pts',(-71.1678459051835,6.37296939622566,-1.1855394350089));
#32994=CARTESIAN_POINT('Ctrl Pts',(-71.0687581199668,6.16506301417589,2.00305783951203));
#32995=CARTESIAN_POINT('Ctrl Pts',(-70.9696703347502,4.4591257413993,4.70493786351959));
#32996=CARTESIAN_POINT('Ctrl Pts',(-70.8705825495335,1.66967835836243,6.26357859827801));
#32997=CARTESIAN_POINT('Ctrl Pts',(-70.7714947643168,-1.5254793560455,6.30025042450449));
#32998=CARTESIAN_POINT('Ctrl Pts',(-70.6724069791001,-4.34996523899484,
4.8060425608526));
#32999=CARTESIAN_POINT('Ctrl Pts',(-70.5839938637413,-5.92705381389802,
2.43080553078847));
#33000=CARTESIAN_POINT('Ctrl Pts',(-70.5286100101214,-6.21839376680658,
0.698770997366347));
#33001=CARTESIAN_POINT('Ctrl Pts',(-70.5062554182403,-6.2189735833399,-0.000140105245378629));
#33002=CARTESIAN_POINT('Origin',(-88.8777445817596,0.,0.));
#33003=CARTESIAN_POINT('',(-73.2527445817597,-6.21935292074379,-0.000155149267013152));
#33004=CARTESIAN_POINT('',(-73.0062554182403,-6.21874727498198,5.02444159825033E-5));
#33005=CARTESIAN_POINT('',(-88.8777445817596,-6.21925,-6.18233832090354E-13));
#33006=CARTESIAN_POINT('Ctrl Pts',(-73.2527445817597,-6.21935292074379,
-0.000155149267012482));
#33007=CARTESIAN_POINT('Ctrl Pts',(-73.2461486481618,-6.21956430959384,
-0.206339320810795));
#33008=CARTESIAN_POINT('Ctrl Pts',(-73.2065234528251,-6.15917337788624,
-1.44487133897756));
#33009=CARTESIAN_POINT('Ctrl Pts',(-73.1338689957495,-5.3590851523311,-3.64697808548958));
#33010=CARTESIAN_POINT('Ctrl Pts',(-73.0347812105328,-2.96571815371499,
-5.7640921799276));
#33011=CARTESIAN_POINT('Ctrl Pts',(-72.9356934253162,0.148280150248475,
-6.48060613083523));
#33012=CARTESIAN_POINT('Ctrl Pts',(-72.8366056400995,3.22624828792765,-5.62241627866711));
#33013=CARTESIAN_POINT('Ctrl Pts',(-72.7375178548829,5.52027965393766,-3.3980517018284));
#33014=CARTESIAN_POINT('Ctrl Pts',(-72.6384300696661,6.47295417930641,-0.348004337008301));
#33015=CARTESIAN_POINT('Ctrl Pts',(-72.5393422844495,5.85278422724426,2.78660359852236));
#33016=CARTESIAN_POINT('Ctrl Pts',(-72.4402544992328,3.81046310673336,5.24410275816569));
#33017=CARTESIAN_POINT('Ctrl Pts',(-72.3411667140162,0.842248539758685,
6.42735250497835));
#33018=CARTESIAN_POINT('Ctrl Pts',(-72.2420789287994,-2.33062157207041,
6.04883839375603));
#33019=CARTESIAN_POINT('Ctrl Pts',(-72.1429911435828,-4.93718066622978,
4.20053447729974));
#33020=CARTESIAN_POINT('Ctrl Pts',(-72.0632130279028,-6.06990209169191,
1.89064539902266));
#33021=CARTESIAN_POINT('Ctrl Pts',(-72.0164641739618,-6.21897289391461,
0.429055152133518));
#33022=CARTESIAN_POINT('Ctrl Pts',(-72.0027445817596,-6.21878348465591,
7.77291339506408E-5));
#33023=CARTESIAN_POINT('Ctrl Pts',(-73.0062554182403,-6.21874727498198,
5.02444159830237E-5));
#33024=CARTESIAN_POINT('Ctrl Pts',(-72.9879789585214,-6.21858534952317,
-0.571418576758583));
#33025=CARTESIAN_POINT('Ctrl Pts',(-72.9366732370636,-5.9993684942345,-2.17576897141618));
#33026=CARTESIAN_POINT('Ctrl Pts',(-72.8523382538668,-4.63711226892121,
-4.52961725564207));
#33027=CARTESIAN_POINT('Ctrl Pts',(-72.7532504686503,-1.90979667128091,
-6.19458790813032));
#33028=CARTESIAN_POINT('Ctrl Pts',(-72.6541626834335,1.28157491443408,-6.35435350101671));
#33029=CARTESIAN_POINT('Ctrl Pts',(-72.5550748982169,4.16154030589149,-4.97009305341768));
#33030=CARTESIAN_POINT('Ctrl Pts',(-72.4559871130002,6.03030501425848,-2.37816402129864));
#33031=CARTESIAN_POINT('Ctrl Pts',(-72.3568993277835,6.4337832898522,0.791628231184674));
#33032=CARTESIAN_POINT('Ctrl Pts',(-72.2578115425668,5.27393510953157,3.76906502167849));
#33033=CARTESIAN_POINT('Ctrl Pts',(-72.1587237573503,2.83258863931502,5.83066756706414));
#33034=CARTESIAN_POINT('Ctrl Pts',(-72.0596359721335,-0.297040379296998,
6.47549300750585));
#33035=CARTESIAN_POINT('Ctrl Pts',(-71.9605481869169,-3.35449241237668,
5.54685706797077));
#33036=CARTESIAN_POINT('Ctrl Pts',(-71.8614604017001,-5.59684600365713,
3.27040631856919));
#33037=CARTESIAN_POINT('Ctrl Pts',(-71.7933628121413,-6.20326561309311,
1.15979613005301));
#33038=CARTESIAN_POINT('Ctrl Pts',(-71.7582944843214,-6.21976122515642,
0.0637936904746014));
#33039=CARTESIAN_POINT('Ctrl Pts',(-71.7562554182403,-6.21972691674719,
6.50263875293274E-5));
#33040=CARTESIAN_POINT('Origin',(-88.8777445817596,0.,0.));
#33041=CARTESIAN_POINT('',(-74.5027445817596,-6.21939977619133,0.000150774270671845));
#33042=CARTESIAN_POINT('',(-74.2562554182403,-6.21945322821522,-0.00014406247351606));
#33043=CARTESIAN_POINT('',(-88.8777445817596,-6.21925,-6.18233832090354E-13));
#33044=CARTESIAN_POINT('Ctrl Pts',(-74.5027445817597,-6.21939977619133,
0.000150774270671963));
#33045=CARTESIAN_POINT('Ctrl Pts',(-74.4758331223618,-6.21854665466753,
-0.841063946683904));
#33046=CARTESIAN_POINT('Ctrl Pts',(-74.4158924012251,-5.83566021064195,
-2.71548027997294));
#33047=CARTESIAN_POINT('Ctrl Pts',(-74.3229224183495,-4.00970737006563,
-5.09337703615375));
#33048=CARTESIAN_POINT('Ctrl Pts',(-74.2238346331329,-1.08929218333971,
-6.39012404928824));
#33049=CARTESIAN_POINT('Ctrl Pts',(-74.1247468479162,2.09580697107931,-6.13415323952314));
#33050=CARTESIAN_POINT('Ctrl Pts',(-74.0256590626996,4.77165203085921,-4.38766221607524));
#33051=CARTESIAN_POINT('Ctrl Pts',(-73.9265712774829,6.2880471181749,-1.5750257983885));
#33052=CARTESIAN_POINT('Ctrl Pts',(-73.8274834922662,6.27652776184059,1.62032159796177));
#33053=CARTESIAN_POINT('Ctrl Pts',(-73.7283957070496,4.73989301704688,4.42195171987746));
#33054=CARTESIAN_POINT('Ctrl Pts',(-73.6293079218328,2.05152533100835,6.1491045398666));
#33055=CARTESIAN_POINT('Ctrl Pts',(-73.5302201366162,-1.13533658159241,
6.38210417280031));
#33056=CARTESIAN_POINT('Ctrl Pts',(-73.4311323513995,-4.04632633089381,
5.06433470950454));
#33057=CARTESIAN_POINT('Ctrl Pts',(-73.3386404997806,-5.84578490937601,
2.68563123354285));
#33058=CARTESIAN_POINT('Ctrl Pts',(-73.2791779099007,-6.21850577594525,
0.826131802093192));
#33059=CARTESIAN_POINT('Ctrl Pts',(-73.2527445817597,-6.21935292074379,
-0.000155149267012482));
#33060=CARTESIAN_POINT('Ctrl Pts',(-74.2562554182403,-6.21945322821522,
-0.000144062473516251));
#33061=CARTESIAN_POINT('Ctrl Pts',(-74.2506926944603,-6.2196254798594,-0.17402274329055));
#33062=CARTESIAN_POINT('Ctrl Pts',(-74.2121007089414,-6.17004795161988,
-1.38022658464286));
#33063=CARTESIAN_POINT('Ctrl Pts',(-74.1404794616836,-5.41525391029054,
-3.5630419256968));
#33064=CARTESIAN_POINT('Ctrl Pts',(-74.0413916764669,-3.05516163314319,
-5.71718725183634));
#33065=CARTESIAN_POINT('Ctrl Pts',(-73.9423038912502,0.047295562592674,
-6.48212972771674));
#33066=CARTESIAN_POINT('Ctrl Pts',(-73.8432161060336,3.13826054590585,-5.67199818610696));
#33067=CARTESIAN_POINT('Ctrl Pts',(-73.744128320817,5.4666686453549,-3.48364415506002));
#33068=CARTESIAN_POINT('Ctrl Pts',(-73.6450405356003,6.4667466886019,-0.448809472545249));
#33069=CARTESIAN_POINT('Ctrl Pts',(-73.5459527503835,5.89548859469092,2.6950801299886));
#33070=CARTESIAN_POINT('Ctrl Pts',(-73.446864965167,3.89170272118268,5.18409998043338));
#33071=CARTESIAN_POINT('Ctrl Pts',(-73.3477771799502,0.94228322147271,6.4134503200478));
#33072=CARTESIAN_POINT('Ctrl Pts',(-73.2486893947337,-2.23609896204665,
6.0844148534698));
#33073=CARTESIAN_POINT('Ctrl Pts',(-73.1496016095169,-4.87113790444004,
4.27694496026283));
#33074=CARTESIAN_POINT('Ctrl Pts',(-73.0687902840191,-6.05484369252271,
1.95530053641333));
#33075=CARTESIAN_POINT('Ctrl Pts',(-73.0210082202603,-6.21887798159982,
0.46134124437055));
#33076=CARTESIAN_POINT('Ctrl Pts',(-73.0062554182403,-6.21874727498198,
5.02444159830237E-5));
#33077=CARTESIAN_POINT('Origin',(-88.8777445817596,0.,0.));
#33078=CARTESIAN_POINT('',(-75.7527445817596,-6.21876477465699,-6.52826263097299E-5));
#33079=CARTESIAN_POINT('',(-75.5062554182403,-6.21929810910058,0.000158575904569969));
#33080=CARTESIAN_POINT('',(-88.8777445817596,-6.21925,-6.18233832090354E-13));
#33081=CARTESIAN_POINT('Ctrl Pts',(-75.7527445817597,-6.21876477465699,
-6.52826263093653E-5));
#33082=CARTESIAN_POINT('Ctrl Pts',(-75.7385468583008,-6.21892878036616,
-0.443996499890235));
#33083=CARTESIAN_POINT('Ctrl Pts',(-75.691319873103,-6.06300112700048,-1.92056570481116));
#33084=CARTESIAN_POINT('Ctrl Pts',(-75.6110636261662,-4.90676653851619,
-4.23602230429382));
#33085=CARTESIAN_POINT('Ctrl Pts',(-75.5119758409496,-2.28694894755983,
-6.06548492185348));
#33086=CARTESIAN_POINT('Ctrl Pts',(-75.4128880557329,0.888567775924808,
-6.42111284230117));
#33087=CARTESIAN_POINT('Ctrl Pts',(-75.3138002705162,3.84817397687645,-5.21649306236172));
#33088=CARTESIAN_POINT('Ctrl Pts',(-75.2147124852996,5.87272347573166,-2.7443326699887));
#33089=CARTESIAN_POINT('Ctrl Pts',(-75.1156247000829,6.47027682562396,0.394665207195212));
#33090=CARTESIAN_POINT('Ctrl Pts',(-75.0165369148663,5.49563626053907,3.43776452332399));
#33091=CARTESIAN_POINT('Ctrl Pts',(-74.9174491296495,3.18562688193913,5.64553134745027));
#33092=CARTESIAN_POINT('Ctrl Pts',(-74.8183613444329,0.101551210018007,
6.48150678297269));
#33093=CARTESIAN_POINT('Ctrl Pts',(-74.7192735592163,-3.00720009769922,
5.74255956855258));
#33094=CARTESIAN_POINT('Ctrl Pts',(-74.6201857739996,-5.38524052207403,
3.60824435777137));
#33095=CARTESIAN_POINT('Ctrl Pts',(-74.5480094481807,-6.16427011766636,
1.41495563973138));
#33096=CARTESIAN_POINT('Ctrl Pts',(-74.5088623841007,-6.21959371695011,
0.191384750590594));
#33097=CARTESIAN_POINT('Ctrl Pts',(-74.5027445817597,-6.21939977619133,
0.000150774270671963));
#33098=CARTESIAN_POINT('Ctrl Pts',(-75.5062554182403,-6.21929810910058,
0.000158575904569969));
#33099=CARTESIAN_POINT('Ctrl Pts',(-75.4803771686603,-6.21846650667767,
-0.808797549377969));
#33100=CARTESIAN_POINT('Ctrl Pts',(-75.4214696573415,-5.85738026136393,
-2.65097162487408));
#33101=CARTESIAN_POINT('Ctrl Pts',(-75.3295328842836,-4.08857452377673,
-5.03028836556254));
#33102=CARTESIAN_POINT('Ctrl Pts',(-75.230445099067,-1.18871686815845,-6.37237749074438));
#33103=CARTESIAN_POINT('Ctrl Pts',(-75.1313573138503,1.99998367272066,-6.1660609781319));
#33104=CARTESIAN_POINT('Ctrl Pts',(-75.0322695286336,4.70271394601358,-4.46147108240762));
#33105=CARTESIAN_POINT('Ctrl Pts',(-74.933181743417,6.26274531336161,-1.67280118877204));
#33106=CARTESIAN_POINT('Ctrl Pts',(-74.8340939582003,6.30101024967761,1.52233784379415));
#33107=CARTESIAN_POINT('Ctrl Pts',(-74.7350061729836,4.8082108683866,4.34756839190818));
#33108=CARTESIAN_POINT('Ctrl Pts',(-74.635918387767,2.14707818808318,6.11639582854541));
#33109=CARTESIAN_POINT('Ctrl Pts',(-74.5368306025503,-1.03576683208741,
6.39901787360667));
#33110=CARTESIAN_POINT('Ctrl Pts',(-74.4377428173336,-3.96693385537629,
5.1267610110341));
#33111=CARTESIAN_POINT('Ctrl Pts',(-74.344217755897,-5.82374674154208,2.75012579862636));
#33112=CARTESIAN_POINT('Ctrl Pts',(-74.2837219561992,-6.21860271747436,
0.858400344144813));
#33113=CARTESIAN_POINT('Ctrl Pts',(-74.2562554182403,-6.21945322821522,
-0.000144062473516251));
#33114=CARTESIAN_POINT('Origin',(-88.8777445817596,0.,0.));
#33115=CARTESIAN_POINT('',(-77.0027445817596,-6.21975224382197,-4.80951439556949E-5));
#33116=CARTESIAN_POINT('',(-76.7562554182403,-6.21880928941777,-9.14614924069079E-5));
#33117=CARTESIAN_POINT('',(-88.8777445817596,-6.21925,-6.18233832090354E-13));
#33118=CARTESIAN_POINT('Ctrl Pts',(-77.0027445817596,-6.21975224382197,
-4.80951439554757E-5));
#33119=CARTESIAN_POINT('Ctrl Pts',(-77.0012605942396,-6.21977142923684,
-0.0464278686673888));
#33120=CARTESIAN_POINT('Ctrl Pts',(-76.9667473449807,-6.20795725940526,
-1.12507719611085));
#33121=CARTESIAN_POINT('Ctrl Pts',(-76.899204833983,-5.6240241962828,-3.22344453428357));
#33122=CARTESIAN_POINT('Ctrl Pts',(-76.8001170487663,-3.40080370644699,
-5.51858468959146));
#33123=CARTESIAN_POINT('Ctrl Pts',(-76.7010292635497,-0.351231726960331,
-6.47277985875879));
#33124=CARTESIAN_POINT('Ctrl Pts',(-76.6019414783329,2.78368503741827,-5.85417290814259));
#33125=CARTESIAN_POINT('Ctrl Pts',(-76.5028536931163,5.24220219865931,-3.81307735750908));
#33126=CARTESIAN_POINT('Ctrl Pts',(-76.4037659078996,6.42693175854569,-0.845453131151542));
#33127=CARTESIAN_POINT('Ctrl Pts',(-76.304678122683,6.04999969635994,2.32760531448557));
#33128=CARTESIAN_POINT('Ctrl Pts',(-76.2055903374662,4.20299564736804,4.93508565418903));
#33129=CARTESIAN_POINT('Ctrl Pts',(-76.1065025522496,1.3347178013573,6.34340375640058));
#33130=CARTESIAN_POINT('Ctrl Pts',(-76.0074147670329,-1.85787927581762,
6.21035646500782));
#33131=CARTESIAN_POINT('Ctrl Pts',(-75.9083269818163,-4.59903562318709,
4.56827255783114));
#33132=CARTESIAN_POINT('Ctrl Pts',(-75.8234369200585,-5.99004202451095,
2.21049216915895));
#33133=CARTESIAN_POINT('Ctrl Pts',(-75.7715761200396,-6.21854724120529,
0.58875501210554));
#33134=CARTESIAN_POINT('Ctrl Pts',(-75.7527445817597,-6.21876477465699,
-6.52826263093653E-5));
#33135=CARTESIAN_POINT('Ctrl Pts',(-76.7562554182403,-6.21880928941777,
-9.14614924065957E-5));
#33136=CARTESIAN_POINT('Ctrl Pts',(-76.7430909045993,-6.2190242752516,-0.411708070281631));
#33137=CARTESIAN_POINT('Ctrl Pts',(-76.6968971292193,-6.07776826767591,
-1.85590942897543));
#33138=CARTESIAN_POINT('Ctrl Pts',(-76.6176740921003,-4.97216739135669,
-4.15906168618827));
#33139=CARTESIAN_POINT('Ctrl Pts',(-76.5185863068837,-2.38117045277481,
-6.02911850538885));
#33140=CARTESIAN_POINT('Ctrl Pts',(-76.419498521667,0.788420230289574,-6.43417719818628));
#33141=CARTESIAN_POINT('Ctrl Pts',(-76.3204107364504,3.76643495425477,-5.27581372041868));
#33142=CARTESIAN_POINT('Ctrl Pts',(-76.2213229512337,5.82925450561374,-2.83549547451091));
#33143=CARTESIAN_POINT('Ctrl Pts',(-76.122235166017,6.47564030775746,0.293811643297502));
#33144=CARTESIAN_POINT('Ctrl Pts',(-76.0231473808003,5.54852893786079,3.3517263168271));
#33145=CARTESIAN_POINT('Ctrl Pts',(-75.9240595955837,3.27319651525233,5.59521467414165));
#33146=CARTESIAN_POINT('Ctrl Pts',(-75.824971810367,0.202519506547572,6.47913794625935));
#33147=CARTESIAN_POINT('Ctrl Pts',(-75.7258840251503,-2.91736713328106,
5.78871416523925));
#33148=CARTESIAN_POINT('Ctrl Pts',(-75.6267962399337,-5.32837114284346,
3.69170741545199));
#33149=CARTESIAN_POINT('Ctrl Pts',(-75.553586704297,-6.15311687587124,1.47960248994997));
#33150=CARTESIAN_POINT('Ctrl Pts',(-75.5134064303992,-6.21952790822279,
0.2236997806532));
#33151=CARTESIAN_POINT('Ctrl Pts',(-75.5062554182403,-6.21929810910058,
0.000158575904569969));
#33152=CARTESIAN_POINT('Origin',(-88.8777445817596,0.,0.));
#33153=CARTESIAN_POINT('',(-78.2527445817596,-6.21893077709273,0.000131417006590163));
#33154=CARTESIAN_POINT('',(-78.0062554182403,-6.2197799278902,-1.48610517280989E-5));
#33155=CARTESIAN_POINT('',(-88.8777445817596,-6.21925,-6.18233832090354E-13));
#33156=CARTESIAN_POINT('Ctrl Pts',(-78.2527445817597,-6.21893077709273,
0.000131417006590355));
#33157=CARTESIAN_POINT('Ctrl Pts',(-78.2309450684397,-6.218405642012,-0.681438740356712));
#33158=CARTESIAN_POINT('Ctrl Pts',(-78.1761162933808,-5.93741656761277,
-2.39610387996943));
#33159=CARTESIAN_POINT('Ctrl Pts',(-78.088258256583,-4.39004082983858,-4.76946373697579));
#33160=CARTESIAN_POINT('Ctrl Pts',(-77.9891704713664,-1.57816084063661,
-6.2872610242504));
#33161=CARTESIAN_POINT('Ctrl Pts',(-77.8900826861497,1.61719190210787,-6.27733487857178));
#33162=CARTESIAN_POINT('Ctrl Pts',(-77.790994900933,4.41958784619184,-4.74209722546579));
#33163=CARTESIAN_POINT('Ctrl Pts',(-77.6919071157163,6.14808087920214,-2.05459103686501));
#33164=CARTESIAN_POINT('Ctrl Pts',(-77.5928193304997,6.3826694615111,1.13215430532706));
#33165=CARTESIAN_POINT('Ctrl Pts',(-77.493731545283,5.06635158971623,4.04380073635643));
#33166=CARTESIAN_POINT('Ctrl Pts',(-77.3946437600663,2.51897554913599,5.97285568290681));
#33167=CARTESIAN_POINT('Ctrl Pts',(-77.2955559748497,-0.640479099061789,
6.45058364410864));
#33168=CARTESIAN_POINT('Ctrl Pts',(-77.196468189633,-3.64430557719005,5.36090287974316));
#33169=CARTESIAN_POINT('Ctrl Pts',(-77.0988643919364,-5.73088793552195,
3.00442020811975));
#33170=CARTESIAN_POINT('Ctrl Pts',(-77.0342898559785,-6.21934441749918,
0.985851485745715));
#33171=CARTESIAN_POINT('Ctrl Pts',(-77.0027445817596,-6.21975224382197,
-4.80951439554757E-5));
#33172=CARTESIAN_POINT('Ctrl Pts',(-78.0062554182403,-6.2197799278902,-1.4861051727765E-5));
#33173=CARTESIAN_POINT('Ctrl Pts',(-78.0058046405381,-6.21978187756921,
-0.0141030499939625));
#33174=CARTESIAN_POINT('Ctrl Pts',(-77.9723246010971,-6.21630091181974,
-1.06045623693887));
#33175=CARTESIAN_POINT('Ctrl Pts',(-77.9058152999171,-5.67356222662317,
-3.13543208152));
#33176=CARTESIAN_POINT('Ctrl Pts',(-77.8067275147004,-3.48636941843915,
-5.46493101103411));
#33177=CARTESIAN_POINT('Ctrl Pts',(-77.7076397294838,-0.452033754894525,
-6.46652210710101));
#33178=CARTESIAN_POINT('Ctrl Pts',(-77.608551944267,2.69214028774311,-5.89683163642142));
#33179=CARTESIAN_POINT('Ctrl Pts',(-77.5094641590505,5.18215892208465,-3.89428704430587));
#33180=CARTESIAN_POINT('Ctrl Pts',(-77.4103763738337,6.41297969776877,-0.945480868762339));
#33181=CARTESIAN_POINT('Ctrl Pts',(-77.3112885886171,6.08552902241152,2.23306497768811));
#33182=CARTESIAN_POINT('Ctrl Pts',(-77.2122008034003,4.27937319172577,4.8690048021263));
#33183=CARTESIAN_POINT('Ctrl Pts',(-77.1131130181838,1.43338480467962,6.32183918483408));
#33184=CARTESIAN_POINT('Ctrl Pts',(-77.014025232967,-1.76089762425562,6.2385480870216));
#33185=CARTESIAN_POINT('Ctrl Pts',(-76.9149374477504,-4.52730461534429,
4.63937017245579));
#33186=CARTESIAN_POINT('Ctrl Pts',(-76.8290141761748,-5.9722511339069,2.2751179173021));
#33187=CARTESIAN_POINT('Ctrl Pts',(-76.7761201663381,-6.21848488400865,
0.621022274220235));
#33188=CARTESIAN_POINT('Ctrl Pts',(-76.7562554182403,-6.21880928941777,
-9.14614924065957E-5));
#33189=CARTESIAN_POINT('Origin',(-88.8777445817596,0.,0.));
#33190=CARTESIAN_POINT('',(-79.5027445817596,-6.21911133157867,-0.000156735226100492));
#33191=CARTESIAN_POINT('',(-79.2562554182404,-6.21886011839245,0.000111780172469961));
#33192=CARTESIAN_POINT('',(-88.8777445817596,-6.21925,-6.18233832090354E-13));
#33193=CARTESIAN_POINT('Ctrl Pts',(-79.5027445817596,-6.21911133157867,
-0.00015673522610081));
#33194=CARTESIAN_POINT('Ctrl Pts',(-79.4936588043785,-6.21938423771565,
-0.284203389274524));
#33195=CARTESIAN_POINT('Ctrl Pts',(-79.4515437652585,-6.13082844877969,
-1.60066773865356));
#33196=CARTESIAN_POINT('Ctrl Pts',(-79.3763994643998,-5.21841112433719,
-3.84557254038601));
#33197=CARTESIAN_POINT('Ctrl Pts',(-79.2773116791831,-2.7472604853497,-5.87135441372885));
#33198=CARTESIAN_POINT('Ctrl Pts',(-79.1782238939664,0.391439059863712,
-6.47047280253847));
#33199=CARTESIAN_POINT('Ctrl Pts',(-79.0791361087498,3.43502395626256,-5.49734965650533));
#33200=CARTESIAN_POINT('Ctrl Pts',(-78.980048323533,5.64394228314933,-3.18844136381023));
#33201=CARTESIAN_POINT('Ctrl Pts',(-78.8809605383164,6.48145534358615,-0.104782894956996));
#33202=CARTESIAN_POINT('Ctrl Pts',(-78.7818727530997,5.74405825318873,3.00433646750017));
#33203=CARTESIAN_POINT('Ctrl Pts',(-78.682784967883,3.61092900537051,5.38344077186245));
#33204=CARTESIAN_POINT('Ctrl Pts',(-78.5836971826664,0.600390527212153,
6.45443832109432));
#33205=CARTESIAN_POINT('Ctrl Pts',(-78.4846093974497,-2.55603511449917,
5.9570905079094));
#33206=CARTESIAN_POINT('Ctrl Pts',(-78.3855216122331,-5.09137715163132,
4.01224644380471));
#33207=CARTESIAN_POINT('Ctrl Pts',(-78.3082333403363,-6.10397284759602,
1.73483310960994));
#33208=CARTESIAN_POINT('Ctrl Pts',(-78.2639743301786,-6.21920129390455,
0.351233814784175));
#33209=CARTESIAN_POINT('Ctrl Pts',(-78.2527445817597,-6.21893077709273,
0.000131417006590355));
#33210=CARTESIAN_POINT('Ctrl Pts',(-79.2562554182403,-6.21886011839245,
0.000111780172470065));
#33211=CARTESIAN_POINT('Ctrl Pts',(-79.2354891147382,-6.21844119785085,
-0.649175810843478));
#33212=CARTESIAN_POINT('Ctrl Pts',(-79.181693549497,-5.95626667819782,-2.33150006579333));
#33213=CARTESIAN_POINT('Ctrl Pts',(-79.0948687225172,-4.46381531427285,
-4.7004888593904));
#33214=CARTESIAN_POINT('Ctrl Pts',(-78.9957809373004,-1.67592360331519,
-6.26191047149678));
#33215=CARTESIAN_POINT('Ctrl Pts',(-78.8966931520838,1.5191959530824,-6.30176850838938));
#33216=CARTESIAN_POINT('Ctrl Pts',(-78.797605366867,4.34517046399522,-4.81037798057634));
#33217=CARTESIAN_POINT('Ctrl Pts',(-78.6985175816505,6.11532452902266,-2.15012757340671));
#33218=CARTESIAN_POINT('Ctrl Pts',(-78.5994297964337,6.39953351445713,1.03257613497986));
#33219=CARTESIAN_POINT('Ctrl Pts',(-78.5003420112172,5.12873829817387,3.96437714477757));
#33220=CARTESIAN_POINT('Ctrl Pts',(-78.4012542260003,2.61172574664976,5.93288557967174));
#33221=CARTESIAN_POINT('Ctrl Pts',(-78.3021664407838,-0.539902515628905,
6.45977924938676));
#33222=CARTESIAN_POINT('Ctrl Pts',(-78.2030786555671,-3.5603414219296,5.41702977991466));
#33223=CARTESIAN_POINT('Ctrl Pts',(-78.1044416480526,-5.70585807478664,
3.06874368313118));
#33224=CARTESIAN_POINT('Ctrl Pts',(-78.038833902277,-6.21963902121677,1.01816291553709));
#33225=CARTESIAN_POINT('Ctrl Pts',(-78.0062554182403,-6.2197799278902,-1.4861051727765E-5));
#33226=CARTESIAN_POINT('Origin',(-88.8777445817596,0.,0.));
#33227=CARTESIAN_POINT('',(-80.7527445817596,-6.21962280111477,0.000107712410215426));
#33228=CARTESIAN_POINT('',(-80.5062554182403,-6.21920956565303,-0.00016035455149499));
#33229=CARTESIAN_POINT('',(-88.8777445817596,-6.21925,-6.18233832090354E-13));
#33230=CARTESIAN_POINT('Ctrl Pts',(-80.7527445817596,-6.21962280111477,
0.000107712410215288));
#33231=CARTESIAN_POINT('Ctrl Pts',(-80.7233432785786,-6.2188772365995,-0.91884081869823));
#33232=CARTESIAN_POINT('Ctrl Pts',(-80.6609127136587,-5.78087320937469,
-2.87081814951415));
#33233=CARTESIAN_POINT('Ctrl Pts',(-80.5654528869998,-3.81569066033551,
-5.24030033591639));
#33234=CARTESIAN_POINT('Ctrl Pts',(-80.4663651017831,-0.84865751236067,
-6.42650941434701));
#33235=CARTESIAN_POINT('Ctrl Pts',(-80.3672773165665,2.32458847824698,-6.05115949490496));
#33236=CARTESIAN_POINT('Ctrl Pts',(-80.2681895313497,4.9329894152624,-4.20545577255142));
#33237=CARTESIAN_POINT('Ctrl Pts',(-80.1691017461332,6.34273747384018,-1.33788047445222));
#33238=CARTESIAN_POINT('Ctrl Pts',(-80.0700139609164,6.21128203689244,1.85478254362996));
#33239=CARTESIAN_POINT('Ctrl Pts',(-79.9709261756998,4.57056508211651,4.59675729793451));
#33240=CARTESIAN_POINT('Ctrl Pts',(-79.871838390483,1.81925969290868,6.22177924678583));
#33241=CARTESIAN_POINT('Ctrl Pts',(-79.7727506052665,-1.37410236497632,
6.3349889910357));
#33242=CARTESIAN_POINT('Ctrl Pts',(-79.6736628200496,-4.23357525011125,
4.90887802126133));
#33243=CARTESIAN_POINT('Ctrl Pts',(-79.5836608122142,-5.89647298261668,
2.53011139605932));
#33244=CARTESIAN_POINT('Ctrl Pts',(-79.5266880661174,-6.21839214998882,
0.748383134600084));
#33245=CARTESIAN_POINT('Ctrl Pts',(-79.5027445817596,-6.21911133157867,
-0.00015673522610081));
#33246=CARTESIAN_POINT('Ctrl Pts',(-80.5062554182403,-6.21920956565303,
-0.000160354551495372));
#33247=CARTESIAN_POINT('Ctrl Pts',(-80.498202850677,-6.2194640039143,-0.251894566613715));
#33248=CARTESIAN_POINT('Ctrl Pts',(-80.4571210213749,-6.14295939465773,
-1.53601476073233));
#33249=CARTESIAN_POINT('Ctrl Pts',(-80.3830099303339,-5.27769101971328,
-3.76380395047722));
#33250=CARTESIAN_POINT('Ctrl Pts',(-80.2839221451171,-2.83840160478908,
-5.82783999498278));
#33251=CARTESIAN_POINT('Ctrl Pts',(-80.1848343599005,0.290582834254973,
-6.47578599813385));
#33252=CARTESIAN_POINT('Ctrl Pts',(-80.0857465746839,3.34895938802227,-5.55019942835999));
#33253=CARTESIAN_POINT('Ctrl Pts',(-79.9866587894671,5.59358195362901,-3.27598589820315));
#33254=CARTESIAN_POINT('Ctrl Pts',(-79.8875710042505,6.47903616408986,-0.205749997827326));
#33255=CARTESIAN_POINT('Ctrl Pts',(-79.7884832190337,5.79016805316885,2.91448050143638));
#33256=CARTESIAN_POINT('Ctrl Pts',(-79.6893954338172,3.69436369744359,5.32652978478494));
#33257=CARTESIAN_POINT('Ctrl Pts',(-79.5903076486004,0.700876556055815,
6.44430094970444));
#33258=CARTESIAN_POINT('Ctrl Pts',(-79.4912198633839,-2.46291455937789,
5.99619000285969));
#33259=CARTESIAN_POINT('Ctrl Pts',(-79.392132078167,-5.0282491654969,4.09108213152337));
#33260=CARTESIAN_POINT('Ctrl Pts',(-79.3138105964527,-6.09021294666528,
1.79949079884625));
#33261=CARTESIAN_POINT('Ctrl Pts',(-79.2685183764771,-6.21910750017158,
0.383530360730315));
#33262=CARTESIAN_POINT('Ctrl Pts',(-79.2562554182403,-6.21886011839245,
0.000111780172470065));
#33263=CARTESIAN_POINT('Origin',(-88.8777445817596,0.,0.));
#33264=CARTESIAN_POINT('',(-82.0027445817596,-6.21872329644988,5.01257785865963E-6));
#33265=CARTESIAN_POINT('',(-81.7562554182403,-6.21953636931397,0.000129532949082536));
#33266=CARTESIAN_POINT('',(-88.8777445817596,-6.21925,-6.18233832090354E-13));
#33267=CARTESIAN_POINT('Ctrl Pts',(-82.0027445817597,-6.21872329644988,
5.01257785858605E-6));
#33268=CARTESIAN_POINT('Ctrl Pts',(-81.9860570145175,-6.21870861559184,
-0.521788036686013));
#33269=CARTESIAN_POINT('Ctrl Pts',(-81.9363401855364,-6.02517739221427,
-2.07636300232439));
#33270=CARTESIAN_POINT('Ctrl Pts',(-81.8535940948165,-4.74430025497663,
-4.41722287377553));
#33271=CARTESIAN_POINT('Ctrl Pts',(-81.7545063095999,-2.0576562319405,-6.14705569009534));
#33272=CARTESIAN_POINT('Ctrl Pts',(-81.6554185243831,1.12897174760274,-6.3832331634597));
#33273=CARTESIAN_POINT('Ctrl Pts',(-81.5563307391665,4.04127413651083,-5.06836721040866));
#33274=CARTESIAN_POINT('Ctrl Pts',(-81.4572429539498,5.97159897215335,-2.52195331871032));
#33275=CARTESIAN_POINT('Ctrl Pts',(-81.3581551687331,6.45090218697082,0.637262740250864));
#33276=CARTESIAN_POINT('Ctrl Pts',(-81.2590673835165,5.36271927440909,3.64163216289869));
#33277=CARTESIAN_POINT('Ctrl Pts',(-81.1599795982997,2.97146466365244,5.76113188346196));
#33278=CARTESIAN_POINT('Ctrl Pts',(-81.0608918130833,-0.141817580336693,
6.48075077439986));
#33279=CARTESIAN_POINT('Ctrl Pts',(-80.9618040278663,-3.22063997927572,
5.62563071573915));
#33280=CARTESIAN_POINT('Ctrl Pts',(-80.8627162426499,-5.5168883532987,3.4035548656095));
#33281=CARTESIAN_POINT('Ctrl Pts',(-80.7930297606142,-6.18902423921956,
1.25918599373804));
#33282=CARTESIAN_POINT('Ctrl Pts',(-80.7563725403174,-6.21971479966146,
0.113500889818269));
#33283=CARTESIAN_POINT('Ctrl Pts',(-80.7527445817596,-6.21962280111477,
0.000107712410215288));
#33284=CARTESIAN_POINT('Ctrl Pts',(-81.7562554182403,-6.21953636931396,
0.000129532949082693));
#33285=CARTESIAN_POINT('Ctrl Pts',(-81.7278873248771,-6.21871470310021,
-0.886561297176356));
#33286=CARTESIAN_POINT('Ctrl Pts',(-81.6664899697749,-5.80403033309651,
-2.80637919144345));
#33287=CARTESIAN_POINT('Ctrl Pts',(-81.5720633529339,-3.89687039929076,
-5.18021657542632));
#33288=CARTESIAN_POINT('Ctrl Pts',(-81.4729755677172,-0.948678281001003,
-6.41250748119229));
#33289=CARTESIAN_POINT('Ctrl Pts',(-81.3738877825005,2.23003043817884,-6.08664167846161));
#33290=CARTESIAN_POINT('Ctrl Pts',(-81.274799997284,4.86687048935458,-4.28180035931612));
#33291=CARTESIAN_POINT('Ctrl Pts',(-81.1757122120671,6.32112370930806,-1.43653671335388));
#33292=CARTESIAN_POINT('Ctrl Pts',(-81.0766244268506,6.23942530007697,1.75778684770072));
#33293=CARTESIAN_POINT('Ctrl Pts',(-80.9775366416338,4.64162692262079,4.52499084953681));
#33294=CARTESIAN_POINT('Ctrl Pts',(-80.8784488564173,1.91597299894771,6.19268036834564));
#33295=CARTESIAN_POINT('Ctrl Pts',(-80.7793610712004,-1.27523768085627,
6.35562833514629));
#33296=CARTESIAN_POINT('Ctrl Pts',(-80.6802732859839,-4.15658203252233,
4.97424049319116));
#33297=CARTESIAN_POINT('Ctrl Pts',(-80.5892380683304,-5.87585161207603,
2.59466305334264));
#33298=CARTESIAN_POINT('Ctrl Pts',(-80.5312321124159,-6.21842037306466,
0.780645069160635));
#33299=CARTESIAN_POINT('Ctrl Pts',(-80.5062554182403,-6.21920956565303,
-0.000160354551495372));
#33300=CARTESIAN_POINT('Origin',(-88.8777445817596,0.,0.));
#33301=CARTESIAN_POINT('',(-83.2527445817597,-6.21959518121893,-0.000115596989317509));
#33302=CARTESIAN_POINT('',(-83.0062554182403,-6.21872885219791,-2.48421024784395E-5));
#33303=CARTESIAN_POINT('',(-88.8777445817596,-6.21925,-6.18233832090354E-13));
#33304=CARTESIAN_POINT('Ctrl Pts',(-83.2527445817596,-6.21959518121893,
-0.000115596989317054));
#33305=CARTESIAN_POINT('Ctrl Pts',(-83.2487707504564,-6.21970139409347,
-0.124320751295493));
#33306=CARTESIAN_POINT('Ctrl Pts',(-83.2117676574143,-6.18576408699328,
-1.2808228962477));
#33307=CARTESIAN_POINT('Ctrl Pts',(-83.1417353026332,-5.49906168580417,
-3.43228253523767));
#33308=CARTESIAN_POINT('Ctrl Pts',(-83.0426475174165,-3.19125505301957,
-5.64235181573731));
#33309=CARTESIAN_POINT('Ctrl Pts',(-82.9435597321999,-0.108014553846464,
-6.48140229287878));
#33310=CARTESIAN_POINT('Ctrl Pts',(-82.8444719469832,3.0014720904087,-5.7455555098245));
#33311=CARTESIAN_POINT('Ctrl Pts',(-82.7453841617665,5.38163968330173,-3.61361275527539));
#33312=CARTESIAN_POINT('Ctrl Pts',(-82.6462963765498,6.45413816238201,-0.603608653732817));
#33313=CARTESIAN_POINT('Ctrl Pts',(-82.5472085913332,5.95836421374577,2.5530645746496));
#33314=CARTESIAN_POINT('Ctrl Pts',(-82.4481208061165,4.01478452008011,5.08937600136816));
#33315=CARTESIAN_POINT('Ctrl Pts',(-82.3490330208998,1.0956639086878,6.38903462388301));
#33316=CARTESIAN_POINT('Ctrl Pts',(-82.2499452356833,-2.08968891757316,
6.13624013983718));
#33317=CARTESIAN_POINT('Ctrl Pts',(-82.1508574504665,-4.76727425738086,
4.39241835221678));
#33318=CARTESIAN_POINT('Ctrl Pts',(-82.068457232492,-6.03062208101894,2.05472217656536));
#33319=CARTESIAN_POINT('Ctrl Pts',(-82.0190862762564,-6.21873767302698,
0.510983184401946));
#33320=CARTESIAN_POINT('Ctrl Pts',(-82.0027445817597,-6.21872329644988,
5.01257785858605E-6));
#33321=CARTESIAN_POINT('Ctrl Pts',(-83.0062554182404,-6.21872885219791,
-2.48421024784395E-5));
#33322=CARTESIAN_POINT('Ctrl Pts',(-82.990601060816,-6.21879717894966,-0.489509848776858));
#33323=CARTESIAN_POINT('Ctrl Pts',(-82.9419174416527,-6.04125906635289,
-2.01171468559772));
#33324=CARTESIAN_POINT('Ctrl Pts',(-82.8602045607506,-4.8125438968831,-4.34277145585205));
#33325=CARTESIAN_POINT('Ctrl Pts',(-82.7611167755339,-2.15317642419824,
-6.11425170920097));
#33326=CARTESIAN_POINT('Ctrl Pts',(-82.6620289903173,1.02938518116893,-6.40004756435293));
#33327=CARTESIAN_POINT('Ctrl Pts',(-82.5629412051006,3.96181944861569,-5.13071431028474));
#33328=CARTESIAN_POINT('Ctrl Pts',(-82.4638534198839,5.93158262837659,-2.61468357548884));
#33329=CARTESIAN_POINT('Ctrl Pts',(-82.3647656346672,6.46004764333774,0.536681584365129));
#33330=CARTESIAN_POINT('Ctrl Pts',(-82.2656778494506,5.41880430283928,3.55764003304445));
#33331=CARTESIAN_POINT('Ctrl Pts',(-82.1665900642338,3.06086132475543,5.71413778516117));
#33332=CARTESIAN_POINT('Ctrl Pts',(-82.0675022790172,-0.0408315235521791,
6.4821736681359));
#33333=CARTESIAN_POINT('Ctrl Pts',(-81.9684144938005,-3.13260283765064,
5.67512485666467));
#33334=CARTESIAN_POINT('Ctrl Pts',(-81.8693267085839,-5.46319201810528,
3.48909381509022));
#33335=CARTESIAN_POINT('Ctrl Pts',(-81.7986070167305,-6.17911475814637,
1.32382249712401));
#33336=CARTESIAN_POINT('Ctrl Pts',(-81.760916586616,-6.219671377491,0.145821920640187));
#33337=CARTESIAN_POINT('Ctrl Pts',(-81.7562554182403,-6.21953636931396,
0.000129532949082693));
#33338=CARTESIAN_POINT('Origin',(-88.8777445817596,0.,0.));
#33339=CARTESIAN_POINT('',(-84.5027445817596,-6.21914365535479,0.000158605856680488));
#33340=CARTESIAN_POINT('',(-84.2562554182403,-6.21967289644367,-9.04560928893794E-5));
#33341=CARTESIAN_POINT('',(-88.8777445817596,-6.21925,-6.18233832090354E-13));
#33342=CARTESIAN_POINT('Ctrl Pts',(-84.5027445817596,-6.21914365535479,
0.000158605856680621));
#33343=CARTESIAN_POINT('Ctrl Pts',(-84.4784552246564,-6.21839883607971,
-0.759182867613572));
#33344=CARTESIAN_POINT('Ctrl Pts',(-84.4211366058144,-5.8896347122068,-2.55172269859188));
#33345=CARTESIAN_POINT('Ctrl Pts',(-84.3307887252331,-4.20791485226097,
-4.93089194986176));
#33346=CARTESIAN_POINT('Ctrl Pts',(-84.2317009400167,-1.34104281493249,
-6.34206961449874));
#33347=CARTESIAN_POINT('Ctrl Pts',(-84.1326131547998,1.85168535032901,-6.21220606459603));
#33348=CARTESIAN_POINT('Ctrl Pts',(-84.0335253695833,4.59447782990876,-4.57285647015062));
#33349=CARTESIAN_POINT('Ctrl Pts',(-83.9344375843666,6.22087138538862,-1.82236166344391));
#33350=CARTESIAN_POINT('Ctrl Pts',(-83.8353497991498,6.33567333489668,1.37094355079113));
#33351=CARTESIAN_POINT('Ctrl Pts',(-83.7362620139334,4.91098828363557,4.23112714344313));
#33352=CARTESIAN_POINT('Ctrl Pts',(-83.6371742287164,2.29299634549289,6.06320134792872));
#33353=CARTESIAN_POINT('Ctrl Pts',(-83.5380864435,-0.8821641649706,6.4219957343511));
#33354=CARTESIAN_POINT('Ctrl Pts',(-83.4389986582831,-3.84297014786777,
5.22032788899049));
#33355=CARTESIAN_POINT('Ctrl Pts',(-83.3438847043698,-5.78869223083908,
2.84925049123928));
#33356=CARTESIAN_POINT('Ctrl Pts',(-83.2818000121953,-6.21881858539693,
0.908034232556073));
#33357=CARTESIAN_POINT('Ctrl Pts',(-83.2527445817596,-6.21959518121893,
-0.000115596989317054));
#33358=CARTESIAN_POINT('Ctrl Pts',(-84.2562554182403,-6.21967289644367,
-9.04560928895008E-5));
#33359=CARTESIAN_POINT('Ctrl Pts',(-84.2533147967549,-6.2197379703033,-0.0919985144304947));
#33360=CARTESIAN_POINT('Ctrl Pts',(-84.2173449135305,-6.19533287709085,
-1.21618959255704));
#33361=CARTESIAN_POINT('Ctrl Pts',(-84.1483457685672,-5.55186853905296,
-3.34619162665173));
#33362=CARTESIAN_POINT('Ctrl Pts',(-84.0492579833507,-3.27877446672824,
-5.59194784252432));
#33363=CARTESIAN_POINT('Ctrl Pts',(-83.950170198134,-0.208980437956675,
-6.47893277120133));
#33364=CARTESIAN_POINT('Ctrl Pts',(-83.8510824129173,2.91159314503785,-5.79162050163479));
#33365=CARTESIAN_POINT('Ctrl Pts',(-83.7519946277006,5.32468710252559,-3.6970190609988));
#33366=CARTESIAN_POINT('Ctrl Pts',(-83.652906842484,6.44395068963483,-0.704089615563853));
#33367=CARTESIAN_POINT('Ctrl Pts',(-83.5538190572673,5.9974172736645,2.4599245359849));
#33368=CARTESIAN_POINT('Ctrl Pts',(-83.4547312720506,4.09358872220742,5.02620871538443));
#33369=CARTESIAN_POINT('Ctrl Pts',(-83.3556434868339,1.19507084710563,6.37118892731869));
#33370=CARTESIAN_POINT('Ctrl Pts',(-83.2565557016173,-1.99383384828571,
6.16805230705936));
#33371=CARTESIAN_POINT('Ctrl Pts',(-83.1574679164006,-4.69826260420316,
4.46615843641225));
#33372=CARTESIAN_POINT('Ctrl Pts',(-83.0740344886083,-6.01417371817795,
2.11936688207577));
#33373=CARTESIAN_POINT('Ctrl Pts',(-83.0236303225549,-6.2186530157556,0.543258725776869));
#33374=CARTESIAN_POINT('Ctrl Pts',(-83.0062554182404,-6.21872885219791,
-2.48421024784395E-5));
#33375=CARTESIAN_POINT('Origin',(-88.8777445817596,0.,0.));
#33376=CARTESIAN_POINT('',(-85.7527445817596,-6.21890566139956,-0.00012576145485806));
#33377=CARTESIAN_POINT('',(-85.5062554182403,-6.21904930984993,0.000151106537523982));
#33378=CARTESIAN_POINT('',(-88.8777445817596,-6.21925,-6.18233832090354E-13));
#33379=CARTESIAN_POINT('Ctrl Pts',(-85.7527445817596,-6.21890566139956,
-0.00012576145485773));
#33380=CARTESIAN_POINT('Ctrl Pts',(-85.7411689605953,-6.21917016689645,
-0.362045793825795));
#33381=CARTESIAN_POINT('Ctrl Pts',(-85.696564077692,-6.09942646984245,-1.75647613111435));
#33382=CARTESIAN_POINT('Ctrl Pts',(-85.6189299330499,-5.07038134923681,
-4.03874760456303));
#33383=CARTESIAN_POINT('Ctrl Pts',(-85.5198421478334,-2.52493057070103,
-5.97034024796873));
#33384=CARTESIAN_POINT('Ctrl Pts',(-85.4207543626165,0.634046276949095,
-6.45121938687785));
#33385=CARTESIAN_POINT('Ctrl Pts',(-85.3216665774001,3.63895781668574,-5.36453420729772));
#33386=CARTESIAN_POINT('Ctrl Pts',(-85.2225787921832,5.75964959979071,-2.97433687429733));
#33387=CARTESIAN_POINT('Ctrl Pts',(-85.1234910069667,6.48082067300681,0.138586273355216));
#33388=CARTESIAN_POINT('Ctrl Pts',(-85.0244032217499,5.62723583982488,3.21783460818738));
#33389=CARTESIAN_POINT('Ctrl Pts',(-84.9253154365333,3.40630517705998,5.51519065308138));
#33390=CARTESIAN_POINT('Ctrl Pts',(-84.8262276513165,0.357686244883394,
6.47242638646756));
#33391=CARTESIAN_POINT('Ctrl Pts',(-84.7271398660999,-2.77784584020579,
5.85694590531591));
#33392=CARTESIAN_POINT('Ctrl Pts',(-84.6280520808834,-5.23839717022127,
3.81830301365183));
#33393=CARTESIAN_POINT('Ctrl Pts',(-84.5532536527698,-6.13494781882954,
1.57902449778438));
#33394=CARTESIAN_POINT('Ctrl Pts',(-84.5114844863953,-6.2194116595431,0.273388236258902));
#33395=CARTESIAN_POINT('Ctrl Pts',(-84.5027445817596,-6.21914365535479,
0.000158605856680621));
#33396=CARTESIAN_POINT('Ctrl Pts',(-85.5062554182403,-6.21904930984993,
0.000151106537523774));
#33397=CARTESIAN_POINT('Ctrl Pts',(-85.4829992709549,-6.21838659122049,
-0.726921510317828));
#33398=CARTESIAN_POINT('Ctrl Pts',(-85.4267138619306,-5.90986944813889,
-2.48715788437484));
#33399=CARTESIAN_POINT('Ctrl Pts',(-85.3373991911673,-4.28422646215156,
-4.86473497443532));
#33400=CARTESIAN_POINT('Ctrl Pts',(-85.2383114059508,-1.43968826503564,
-6.32040665848384));
#33401=CARTESIAN_POINT('Ctrl Pts',(-85.139223620734,1.75467563421941,-6.24030096387333));
#33402=CARTESIAN_POINT('Ctrl Pts',(-85.0401358355174,4.52267595876155,-4.64388251792204));
#33403=CARTESIAN_POINT('Ctrl Pts',(-84.9410480503007,6.19172428905613,-1.919060449145));
#33404=CARTESIAN_POINT('Ctrl Pts',(-84.8419602650839,6.35626338222264,1.27206858835509));
#33405=CARTESIAN_POINT('Ctrl Pts',(-84.7428724798673,4.9763123584096,4.15410134539831));
#33406=CARTESIAN_POINT('Ctrl Pts',(-84.6437846946507,2.38718153906689,6.02674099139694));
#33407=CARTESIAN_POINT('Ctrl Pts',(-84.544696909434,-0.782003641280745,
6.43496021602791));
#33408=CARTESIAN_POINT('Ctrl Pts',(-84.4456091242173,-3.76117201100048,
5.27956700696203));
#33409=CARTESIAN_POINT('Ctrl Pts',(-84.3494619604861,-5.76513369117889,
2.91366710550249));
#33410=CARTESIAN_POINT('Ctrl Pts',(-84.2863440584938,-6.2190070562591,0.940319085696299));
#33411=CARTESIAN_POINT('Ctrl Pts',(-84.2562554182403,-6.21967289644367,
-9.04560928895008E-5));
#33412=CARTESIAN_POINT('Origin',(28.1999754182402,0.,0.));
#33413=CARTESIAN_POINT('',(108.82497541824,-6.21455514838355,-0.00757742687950716));
#33414=CARTESIAN_POINT('',(109.067,-6.21925,5.68729293530136E-12));
#33415=CARTESIAN_POINT('',(28.1999754182402,-6.21925,5.68729293530136E-12));
#33416=CARTESIAN_POINT('',(109.067,-2.15736603634146,-5.83308171961789));
#33417=CARTESIAN_POINT('Ctrl Pts',(108.82497541824,-6.21455514838355,-0.00757742687950716));
#33418=CARTESIAN_POINT('Ctrl Pts',(108.844499925929,-6.21989172346176,-0.619498065585236));
#33419=CARTESIAN_POINT('Ctrl Pts',(108.864024433619,-6.13743667878425,-1.2297196011537));
#33420=CARTESIAN_POINT('Ctrl Pts',(108.883548941308,-5.96152933675784,-1.81073897317348));
#33421=CARTESIAN_POINT('Ctrl Pts',(108.944699294205,-5.41059119207356,-3.63047958865122));
#33422=CARTESIAN_POINT('Ctrl Pts',(109.005849647103,-3.94295198716987,-5.16376759627442));
#33423=CARTESIAN_POINT('Ctrl Pts',(109.067,-2.15756780909074,-5.83789702209062));
#33424=CARTESIAN_POINT('Origin',(109.067,0.,0.));
#33425=CARTESIAN_POINT('Origin',(28.1999754182402,0.,0.));
#33426=CARTESIAN_POINT('',(107.57497541824,-6.21197113448905,0.00272930593023462));
#33427=CARTESIAN_POINT('',(107.821464581759,-6.21681811402912,-0.00341565526005089));
#33428=CARTESIAN_POINT('',(28.1999754182402,-6.21925,5.68729293530136E-12));
#33429=CARTESIAN_POINT('Ctrl Pts',(107.57497541824,-6.21197113448905,0.00272930593023461));
#33430=CARTESIAN_POINT('Ctrl Pts',(107.614143383712,-6.20682472272673,-1.22554755889008));
#33431=CARTESIAN_POINT('Ctrl Pts',(107.719481883998,-5.25859683548935,-4.53616070271995));
#33432=CARTESIAN_POINT('Ctrl Pts',(107.890990919097,0.136997792198854,-7.35133649303282));
#33433=CARTESIAN_POINT('Ctrl Pts',(108.056417256132,5.21425114731496,-4.45398626681165));
#33434=CARTESIAN_POINT('Ctrl Pts',(108.18875832576,6.46158639258335,-0.360283155660035));
#33435=CARTESIAN_POINT('Ctrl Pts',(108.288014127981,5.8651082250223,2.77856311405613));
#33436=CARTESIAN_POINT('Ctrl Pts',(108.387269930202,3.81258651774621,5.23074243008551));
#33437=CARTESIAN_POINT('Ctrl Pts',(108.519610999831,-0.144983932043383,
6.8528582990123));
#33438=CARTESIAN_POINT('Ctrl Pts',(108.665512829176,-4.95903172843287,5.01362006060166));
#33439=CARTESIAN_POINT('Ctrl Pts',(108.778329391115,-6.20180552981113,1.45436297979792));
#33440=CARTESIAN_POINT('Ctrl Pts',(108.82497541824,-6.21455514838355,-0.00757742687950737));
#33441=CARTESIAN_POINT('',(109.067,-6.21768400249992,0.139557183823105));
#33442=CARTESIAN_POINT('Origin',(109.067,0.,0.));
#33443=CARTESIAN_POINT('Ctrl Pts',(107.821464581759,-6.21681811402912,-0.00341565526005082));
#33444=CARTESIAN_POINT('Ctrl Pts',(107.839619845622,-6.21808736455384,-0.570723268463156));
#33445=CARTESIAN_POINT('Ctrl Pts',(107.890860376892,-6.0060659270755,-2.16948211616312));
#33446=CARTESIAN_POINT('Ctrl Pts',(107.975186175568,-4.63696157612732,-4.51609008620458));
#33447=CARTESIAN_POINT('Ctrl Pts',(108.107527245197,-1.00805461892616,-6.77986084607601));
#33448=CARTESIAN_POINT('Ctrl Pts',(108.272953582231,4.72291868063634,-5.64086832996922));
#33449=CARTESIAN_POINT('Ctrl Pts',(108.471465186674,7.29544819300465,0.934110138162679));
#33450=CARTESIAN_POINT('Ctrl Pts',(108.636891523709,3.86681832161873,5.66141617959935));
#33451=CARTESIAN_POINT('Ctrl Pts',(108.769232593337,-0.340764604699964,
6.46373036659584));
#33452=CARTESIAN_POINT('Ctrl Pts',(108.868488395558,-3.38799745293929,5.53147877557648));
#33453=CARTESIAN_POINT('Ctrl Pts',(108.967744197779,-5.62418538167471,3.22542302469746));
#33454=CARTESIAN_POINT('Ctrl Pts',(109.033914732593,-6.19447498791001,1.17358721206399));
#33455=CARTESIAN_POINT('Ctrl Pts',(109.067,-6.21768400249992,0.139557183822751));
#33456=CARTESIAN_POINT('Origin',(28.1999754182402,0.,0.));
#33457=CARTESIAN_POINT('',(106.32497541824,-6.22618423365076,0.00404232319106064));
#33458=CARTESIAN_POINT('',(106.57146458176,-6.21560315594324,0.00241033447495986));
#33459=CARTESIAN_POINT('',(28.1999754182402,-6.21925,5.68729293530136E-12));
#33460=CARTESIAN_POINT('Ctrl Pts',(106.32497541824,-6.22618423365075,0.004042323191061));
#33461=CARTESIAN_POINT('Ctrl Pts',(106.383786841494,-6.21175399018336,-1.82954563581619));
#33462=CARTESIAN_POINT('Ctrl Pts',(106.508768799563,-4.38464470241311,-5.75083267620402));
#33463=CARTESIAN_POINT('Ctrl Pts',(106.666836025037,1.10798790665508,-6.76730712296029));
#33464=CARTESIAN_POINT('Ctrl Pts',(106.799177094666,4.70262135634261,-4.44608868040009));
#33465=CARTESIAN_POINT('Ctrl Pts',(106.898432896887,6.2736721784315,-1.66275690292686));
#33466=CARTESIAN_POINT('Ctrl Pts',(106.997688699108,6.28738997577458,1.53331465981352));
#33467=CARTESIAN_POINT('Ctrl Pts',(107.130029768736,4.31428373900651,5.33021287136194));
#33468=CARTESIAN_POINT('Ctrl Pts',(107.295456105771,-1.20636992374352,7.25309034469861));
#33469=CARTESIAN_POINT('Ctrl Pts',(107.454799744741,-5.65798516834366,3.76690557215357));
#33470=CARTESIAN_POINT('Ctrl Pts',(107.547972848898,-6.21551909361338,0.849508831356341));
#33471=CARTESIAN_POINT('Ctrl Pts',(107.57497541824,-6.21197113448905,0.00272930593023461));
#33472=CARTESIAN_POINT('Ctrl Pts',(106.57146458176,-6.21560315594324,0.00241033447496005));
#33473=CARTESIAN_POINT('Ctrl Pts',(106.576178035998,-6.21571381863042,-0.145160143453014));
#33474=CARTESIAN_POINT('Ctrl Pts',(106.613976757643,-6.1753255886943,-1.32900497305834));
#33475=CARTESIAN_POINT('Ctrl Pts',(106.717946014101,-5.14823859197666,-4.5298844173743));
#33476=CARTESIAN_POINT('Ctrl Pts',(106.883372351137,-0.0289675534008062,
-7.35267358327051));
#33477=CARTESIAN_POINT('Ctrl Pts',(107.081883955579,6.1675620574163,-4.00271286495399));
#33478=CARTESIAN_POINT('Ctrl Pts',(107.280395560021,6.70875004256005,3.00890426696354));
#33479=CARTESIAN_POINT('Ctrl Pts',(107.478907164463,1.09964973772579,7.26991658020799));
#33480=CARTESIAN_POINT('Ctrl Pts',(107.644333501498,-4.39210610522649,5.26648010085043));
#33481=CARTESIAN_POINT('Ctrl Pts',(107.758519307264,-6.04627559345864,1.96530621919418));
#33482=CARTESIAN_POINT('Ctrl Pts',(107.806534578215,-6.21577434430061,0.463110457495906));
#33483=CARTESIAN_POINT('Ctrl Pts',(107.821464581759,-6.21681811402912,-0.00341565526005082));
#33484=CARTESIAN_POINT('Origin',(28.1999754182402,0.,0.));
#33485=CARTESIAN_POINT('',(105.07497541824,-6.22210088067886,-0.00776764447856886));
#33486=CARTESIAN_POINT('',(105.321464581759,-6.21925,5.80383180751043E-12));
#33487=CARTESIAN_POINT('',(28.1999754182402,-6.21925,5.68729293530136E-12));
#33488=CARTESIAN_POINT('Ctrl Pts',(105.07497541824,-6.22210088067886,-0.00776764447856897));
#33489=CARTESIAN_POINT('Ctrl Pts',(105.087259764463,-6.22564393247865,-0.391088311636573));
#33490=CARTESIAN_POINT('Ctrl Pts',(105.165714645499,-6.01911196292566,-2.83449884888709));
#33491=CARTESIAN_POINT('Ctrl Pts',(105.277254793943,-3.52167204419261,-5.88403957747914));
#33492=CARTESIAN_POINT('Ctrl Pts',(105.409595863571,0.722150160936881,-6.43123931018474));
#33493=CARTESIAN_POINT('Ctrl Pts',(105.508851665792,3.71862112089202,-5.3193600409715));
#33494=CARTESIAN_POINT('Ctrl Pts',(105.608107468013,5.79200698135239,-2.88703913835982));
#33495=CARTESIAN_POINT('Ctrl Pts',(105.740448537641,6.73563905550354,1.2865699056858));
#33496=CARTESIAN_POINT('Ctrl Pts',(105.905874874676,3.76008989159166,6.31860060108252));
#33497=CARTESIAN_POINT('Ctrl Pts',(106.104386479118,-3.27915422052681,6.58083808626542));
#33498=CARTESIAN_POINT('Ctrl Pts',(106.244086660306,-6.11378249632262,2.52412807553831));
#33499=CARTESIAN_POINT('Ctrl Pts',(106.31761630668,-6.22798989938095,0.233480374486457));
#33500=CARTESIAN_POINT('Ctrl Pts',(106.32497541824,-6.22618423365075,0.004042323191061));
#33501=CARTESIAN_POINT('Ctrl Pts',(105.321464581759,-6.22149027562554,0.00277977264042391));
#33502=CARTESIAN_POINT('Ctrl Pts',(105.378906761187,-6.205339920575,-1.79044338804944));
#33503=CARTESIAN_POINT('Ctrl Pts',(105.502519475428,-4.46474788533615,-5.66066214127837));
#33504=CARTESIAN_POINT('Ctrl Pts',(105.692302724484,2.12728060596421,-7.03810766777042));
#33505=CARTESIAN_POINT('Ctrl Pts',(105.890814328926,7.06620582008108,-2.03199906838922));
#33506=CARTESIAN_POINT('Ctrl Pts',(106.089325933368,5.53238437901881,4.84311030515874));
#33507=CARTESIAN_POINT('Ctrl Pts',(106.254752270403,0.0443617744349961,
6.85726730780797));
#33508=CARTESIAN_POINT('Ctrl Pts',(106.387093340032,-3.88907072626489,5.1727633873222));
#33509=CARTESIAN_POINT('Ctrl Pts',(106.481635688015,-5.80953565783217,2.81060433023539));
#33510=CARTESIAN_POINT('Ctrl Pts',(106.543092768591,-6.21493704125813,0.890685008966381));
#33511=CARTESIAN_POINT('Ctrl Pts',(106.57146458176,-6.21560315594324,0.00241033447496005));
#33512=CARTESIAN_POINT('Origin',(28.1999754182402,0.,0.));
#33513=CARTESIAN_POINT('',(103.82497541824,-6.2174167363618,0.000391862094605458));
#33514=CARTESIAN_POINT('',(104.07146458176,-6.21925,5.31621332200516E-12));
#33515=CARTESIAN_POINT('',(28.1999754182402,-6.21925,5.68729293530136E-12));
#33516=CARTESIAN_POINT('Ctrl Pts',(103.82497541824,-6.20679593735384,0.00266206938908144));
#33517=CARTESIAN_POINT('Ctrl Pts',(103.856903222245,-6.20668924563014,-0.998325940866833));
#33518=CARTESIAN_POINT('Ctrl Pts',(103.921916293657,-5.74038997171335,-3.03807828006894));
#33519=CARTESIAN_POINT('Ctrl Pts',(104.020014632476,-3.59946059997928,-5.37831045715732));
#33520=CARTESIAN_POINT('Ctrl Pts',(104.119270434697,-0.593085485580851,
-6.46312492323568));
#33521=CARTESIAN_POINT('Ctrl Pts',(104.218526236918,2.56051311720067,-5.94357742119504));
#33522=CARTESIAN_POINT('Ctrl Pts',(104.350867306546,5.97511638043491,-3.364829852218));
#33523=CARTESIAN_POINT('Ctrl Pts',(104.516293643581,6.95030565375228,2.39921649231612));
#33524=CARTESIAN_POINT('Ctrl Pts',(104.714805248023,1.74297217383987,7.14299183158766));
#33525=CARTESIAN_POINT('Ctrl Pts',(104.901032506243,-4.63366916893313,5.45146242636149));
#33526=CARTESIAN_POINT('Ctrl Pts',(105.021089229649,-6.20655902326007,1.67369666688253));
#33527=CARTESIAN_POINT('Ctrl Pts',(105.07497541824,-6.22210088067886,-0.00776764447856897));
#33528=CARTESIAN_POINT('Ctrl Pts',(104.07146458176,-6.21925,5.31621332200516E-12));
#33529=CARTESIAN_POINT('Ctrl Pts',(104.130264333233,-6.21925000000157,-1.83816020915209));
#33530=CARTESIAN_POINT('Ctrl Pts',(104.189064084707,-5.35502977485331,-3.6580814134549));
#33531=CARTESIAN_POINT('Ctrl Pts',(104.247863836181,-3.93049712176249,-4.81977830800513));
#33532=CARTESIAN_POINT('Ctrl Pts',(104.306663587654,-2.50596446867168,-5.98147520255536));
#33533=CARTESIAN_POINT('Ctrl Pts',(104.365463339128,-0.549389021424183,
-6.46189408921008));
#33534=CARTESIAN_POINT('Ctrl Pts',(104.424263090602,1.25118869866398,-6.09209302316007));
#33535=CARTESIAN_POINT('Ctrl Pts',(104.483062842075,3.05176641875214,-5.72229195711005));
#33536=CARTESIAN_POINT('Ctrl Pts',(104.541862593549,4.66061422074842,-4.50960958425308));
#33537=CARTESIAN_POINT('Ctrl Pts',(104.600662345023,5.51197192302482,-2.88049233331493));
#33538=CARTESIAN_POINT('Ctrl Pts',(104.659462096496,6.36332962530122,-1.25137508237678));
#33539=CARTESIAN_POINT('Ctrl Pts',(104.71826184797,6.44030216377344,0.761847462635921));
#33540=CARTESIAN_POINT('Ctrl Pts',(104.777061599444,5.71582172177643,2.45121451679953));
#33541=CARTESIAN_POINT('Ctrl Pts',(104.835861350918,4.99134127977942,4.14058157096314));
#33542=CARTESIAN_POINT('Ctrl Pts',(104.894661102391,3.47978506146911,5.47256790209185));
#33543=CARTESIAN_POINT('Ctrl Pts',(104.953460853865,1.71270012776144,5.97877318811025));
#33544=CARTESIAN_POINT('Ctrl Pts',(105.012260605339,-0.0543848059462324,
6.48497847412864));
#33545=CARTESIAN_POINT('Ctrl Pts',(105.071060356812,-2.04193092336917,6.15535714814489));
#33546=CARTESIAN_POINT('Ctrl Pts',(105.129860108286,-3.55100669662017,5.10582236305365));
#33547=CARTESIAN_POINT('Ctrl Pts',(105.18865985976,-5.06008246987117,4.05628757796241));
#33548=CARTESIAN_POINT('Ctrl Pts',(105.247459611233,-6.06074051980635,2.30766719190768));
#33549=CARTESIAN_POINT('Ctrl Pts',(105.306259362707,-6.20109393743633,0.474873184745606));
#33550=CARTESIAN_POINT('Ctrl Pts',(105.311327769058,-6.21319208641554,0.31689046283348));
#33551=CARTESIAN_POINT('Ctrl Pts',(105.316396175409,-6.21924999999985,0.158445276462653));
#33552=CARTESIAN_POINT('Ctrl Pts',(105.321464581759,-6.21925,5.80383131895764E-12));
#33553=CARTESIAN_POINT('Origin',(28.1999754182402,0.,0.));
#33554=CARTESIAN_POINT('',(102.57497541824,-6.21925,5.30358233294917E-12));
#33555=CARTESIAN_POINT('',(102.82146458176,-6.20834130759024,0.000316658844899398));
#33556=CARTESIAN_POINT('',(28.1999754182402,-6.21925,5.68729293530136E-12));
#33557=CARTESIAN_POINT('Ctrl Pts',(102.57497541824,-6.21925,5.30358233294917E-12));
#33558=CARTESIAN_POINT('Ctrl Pts',(102.633775169714,-6.21925000000157,-1.83816020915211));
#33559=CARTESIAN_POINT('Ctrl Pts',(102.692574921188,-5.3550297748533,-3.65808141345491));
#33560=CARTESIAN_POINT('Ctrl Pts',(102.751374672661,-3.93049712176248,-4.81977830800514));
#33561=CARTESIAN_POINT('Ctrl Pts',(102.810174424135,-2.50596446867166,-5.98147520255537));
#33562=CARTESIAN_POINT('Ctrl Pts',(102.868974175609,-0.549389021424171,
-6.46189408921008));
#33563=CARTESIAN_POINT('Ctrl Pts',(102.927773927082,1.25118869866399,-6.09209302316006));
#33564=CARTESIAN_POINT('Ctrl Pts',(102.986573678556,3.05176641875215,-5.72229195711004));
#33565=CARTESIAN_POINT('Ctrl Pts',(103.04537343003,4.66061422074843,-4.50960958425307));
#33566=CARTESIAN_POINT('Ctrl Pts',(103.104173181503,5.51197192302482,-2.88049233331492));
#33567=CARTESIAN_POINT('Ctrl Pts',(103.162972932977,6.36332962530122,-1.25137508237677));
#33568=CARTESIAN_POINT('Ctrl Pts',(103.221772684451,6.44030216377344,0.761847462635935));
#33569=CARTESIAN_POINT('Ctrl Pts',(103.280572435925,5.71582172177642,2.45121451679954));
#33570=CARTESIAN_POINT('Ctrl Pts',(103.339372187398,4.99134127977941,4.14058157096315));
#33571=CARTESIAN_POINT('Ctrl Pts',(103.398171938872,3.4797850614691,5.47256790209186));
#33572=CARTESIAN_POINT('Ctrl Pts',(103.456971690346,1.71270012776143,5.97877318811025));
#33573=CARTESIAN_POINT('Ctrl Pts',(103.515771441819,-0.0543848059462451,
6.48497847412864));
#33574=CARTESIAN_POINT('Ctrl Pts',(103.574571193293,-2.04193092336918,6.15535714814488));
#33575=CARTESIAN_POINT('Ctrl Pts',(103.633370944767,-3.55100669662018,5.10582236305364));
#33576=CARTESIAN_POINT('Ctrl Pts',(103.69217069624,-5.06008246987118,4.0562875779624));
#33577=CARTESIAN_POINT('Ctrl Pts',(103.750970447714,-6.06074051980636,2.30766719190766));
#33578=CARTESIAN_POINT('Ctrl Pts',(103.809770199188,-6.20109393743633,0.474873184745594));
#33579=CARTESIAN_POINT('Ctrl Pts',(103.814838605539,-6.21319208641554,0.316890462833468));
#33580=CARTESIAN_POINT('Ctrl Pts',(103.819907011889,-6.21924999999985,0.15844527646264));
#33581=CARTESIAN_POINT('Ctrl Pts',(103.82497541824,-6.21925,5.79120032990165E-12));
#33582=CARTESIAN_POINT('Ctrl Pts',(102.82146458176,-6.20834130759024,0.000316658844898982));
#33583=CARTESIAN_POINT('Ctrl Pts',(102.852023141938,-6.21030615967812,-0.959220914400505));
#33584=CARTESIAN_POINT('Ctrl Pts',(102.94875223693,-5.55144391813371,-3.99518424091588));
#33585=CARTESIAN_POINT('Ctrl Pts',(103.111651866737,-0.82496606132839,-7.30614229910194));
#33586=CARTESIAN_POINT('Ctrl Pts',(103.310163471179,5.69801405622591,-4.64710923843941));
#33587=CARTESIAN_POINT('Ctrl Pts',(103.475589808214,6.76861424179842,1.09998042754471));
#33588=CARTESIAN_POINT('Ctrl Pts',(103.607930877842,4.45164816401902,4.69735761978553));
#33589=CARTESIAN_POINT('Ctrl Pts',(103.707186680063,1.67018130387269,6.27170061297181));
#33590=CARTESIAN_POINT('Ctrl Pts',(103.806442482284,-1.52587995074471,6.2891995008118));
#33591=CARTESIAN_POINT('Ctrl Pts',(103.927868449516,-5.01174531446683,4.48295294983669));
#33592=CARTESIAN_POINT('Ctrl Pts',(104.016209149341,-6.20768450607271,1.71559912667801));
#33593=CARTESIAN_POINT('Ctrl Pts',(104.071464581759,-6.22368981997608,-0.00517086289489384));
#33594=CARTESIAN_POINT('Origin',(28.1999754182402,0.,0.));
#33595=CARTESIAN_POINT('',(101.32497541824,-6.22105475706665,-0.00162676184122019));
#33596=CARTESIAN_POINT('',(101.57146458176,-6.21989505726344,0.0051066519576129));
#33597=CARTESIAN_POINT('',(28.1999754182402,-6.21925,5.68729293530136E-12));
#33598=CARTESIAN_POINT('Ctrl Pts',(101.32497541824,-6.22105475706665,-0.00162676184122041));
#33599=CARTESIAN_POINT('Ctrl Pts',(101.330019602996,-6.22143817055166,-0.158868376741796));
#33600=CARTESIAN_POINT('Ctrl Pts',(101.368149055159,-6.17819176943028,-1.34717661173896));
#33601=CARTESIAN_POINT('Ctrl Pts',(101.439363774729,-5.43325591434297,-3.51597357120765));
#33602=CARTESIAN_POINT('Ctrl Pts',(101.571704844356,-2.3211098600259,-6.45263858533859));
#33603=CARTESIAN_POINT('Ctrl Pts',(101.737131181392,3.52484809098738,-6.45278501071125));
#33604=CARTESIAN_POINT('Ctrl Pts',(101.935642785834,7.33364606630008,-0.527180871479639));
#33605=CARTESIAN_POINT('Ctrl Pts',(102.134154390276,4.42207903767292,5.87413834375616));
#33606=CARTESIAN_POINT('Ctrl Pts',(102.332665994718,-2.54733029566822,6.89739782988979));
#33607=CARTESIAN_POINT('Ctrl Pts',(102.479606337373,-5.95970016665688,2.98335614725549));
#33608=CARTESIAN_POINT('Ctrl Pts',(102.560376145214,-6.22546141667382,0.459170652905071));
#33609=CARTESIAN_POINT('Ctrl Pts',(102.57497541824,-6.22306105720208,0.00238369616239718));
#33610=CARTESIAN_POINT('Ctrl Pts',(101.57146458176,-6.21989505726344,0.00510665195761345));
#33611=CARTESIAN_POINT('Ctrl Pts',(101.62166659972,-6.2061803997074,-1.56410508432724));
#33612=CARTESIAN_POINT('Ctrl Pts',(101.738039152495,-4.80701918903245,-5.22328206966102));
#33613=CARTESIAN_POINT('Ctrl Pts',(101.920582240084,1.3526844941182,-7.22725626488847));
#33614=CARTESIAN_POINT('Ctrl Pts',(102.086008577119,5.87986878794746,-3.52863128306579));
#33615=CARTESIAN_POINT('Ctrl Pts',(102.218349646747,6.43208922602856,0.714540532497019));
#33616=CARTESIAN_POINT('Ctrl Pts',(102.317605448968,5.32375599492072,3.71232491487952));
#33617=CARTESIAN_POINT('Ctrl Pts',(102.416861251189,2.89388995296144,5.78858712677963));
#33618=CARTESIAN_POINT('Ctrl Pts',(102.549202320817,-1.27859977470671,6.73715654497048));
#33619=CARTESIAN_POINT('Ctrl Pts',(102.684070097674,-5.38395033335684,4.31612449633043));
#33620=CARTESIAN_POINT('Ctrl Pts',(102.785852607124,-6.20605153142578,1.11853124490405));
#33621=CARTESIAN_POINT('Ctrl Pts',(102.82146458176,-6.20834130759024,0.000316658844898982));
#33622=CARTESIAN_POINT('Origin',(28.1999754182402,0.,0.));
#33623=CARTESIAN_POINT('',(100.07497541824,-6.21925,5.38891630971761E-12));
#33624=CARTESIAN_POINT('',(100.32146458176,-6.22909731479716,-0.0014603442074157));
#33625=CARTESIAN_POINT('',(28.1999754182402,-6.21925,5.68729293530136E-12));
#33626=CARTESIAN_POINT('Ctrl Pts',(100.07497541824,-6.21823345339706,-0.000850643466643111));
#33627=CARTESIAN_POINT('Ctrl Pts',(100.099663060778,-6.22121061960845,-0.774526207076587));
#33628=CARTESIAN_POINT('Ctrl Pts',(100.190521238131,-5.71106097194565,-3.62193451684539));
#33629=CARTESIAN_POINT('Ctrl Pts',(100.347549950297,-1.47265859680333,-7.20376742519206));
#33630=CARTESIAN_POINT('Ctrl Pts',(100.546061554739,5.26119106866268,-5.13616129381046));
#33631=CARTESIAN_POINT('Ctrl Pts',(100.744573159181,7.16905691026357,1.63245438356331));
#33632=CARTESIAN_POINT('Ctrl Pts',(100.943084763623,2.50626464765636,6.91242547698743));
#33633=CARTESIAN_POINT('Ctrl Pts',(101.108511100658,-3.27215427013865,6.02636724135885));
#33634=CARTESIAN_POINT('Ctrl Pts',(101.235807985531,-5.8030391565124,2.78060935378298));
#33635=CARTESIAN_POINT('Ctrl Pts',(101.296934335589,-6.21892332656926,0.872493702243004));
#33636=CARTESIAN_POINT('Ctrl Pts',(101.32497541824,-6.22105475706665,-0.00162676184122041));
#33637=CARTESIAN_POINT('Ctrl Pts',(100.32146458176,-6.22909731479716,-0.00146034420741566));
#33638=CARTESIAN_POINT('Ctrl Pts',(100.325139522689,-6.22952837035362,-0.115891893155128));
#33639=CARTESIAN_POINT('Ctrl Pts',(100.394984998432,-6.17349008821943,-2.29036018435994));
#33640=CARTESIAN_POINT('Ctrl Pts',(100.531001008989,-3.63164551501983,-6.39328861480798));
#33641=CARTESIAN_POINT('Ctrl Pts',(100.696427346024,2.21350682387351,-6.49033768273847));
#33642=CARTESIAN_POINT('Ctrl Pts',(100.828768415652,5.37404798958258,-3.60582143066423));
#33643=CARTESIAN_POINT('Ctrl Pts',(100.928024217873,6.46241869027549,-0.600731919134315));
#33644=CARTESIAN_POINT('Ctrl Pts',(101.027280020095,5.94660273312621,2.55347917918856));
#33645=CARTESIAN_POINT('Ctrl Pts',(101.159621089723,3.3718969584413,5.97113109862479));
#33646=CARTESIAN_POINT('Ctrl Pts',(101.325047426758,-2.39099155665315,6.95313942295208));
#33647=CARTESIAN_POINT('Ctrl Pts',(101.473357013239,-5.93970404826024,3.06689542039316));
#33648=CARTESIAN_POINT('Ctrl Pts',(101.555496064906,-6.22425748628952,0.504249616225492));
#33649=CARTESIAN_POINT('Ctrl Pts',(101.57146458176,-6.21989505726344,0.00510665195761345));
#33650=CARTESIAN_POINT('Origin',(28.1999754182402,0.,0.));
#33651=CARTESIAN_POINT('',(98.8249754182402,-6.21788518063575,0.00023803869261306));
#33652=CARTESIAN_POINT('',(99.0714645817595,-6.21907165140323,-0.00016453540808593));
#33653=CARTESIAN_POINT('',(28.1999754182402,-6.21925,5.68729293530136E-12));
#33654=CARTESIAN_POINT('Ctrl Pts',(98.8249754182402,-6.21925,5.25482207309205E-12));
#33655=CARTESIAN_POINT('Ctrl Pts',(98.8837751697139,-6.21925000000155,-1.83816020915227));
#33656=CARTESIAN_POINT('Ctrl Pts',(98.9425749211876,-5.35502977485315,-3.65808141345518));
#33657=CARTESIAN_POINT('Ctrl Pts',(99.0013746726613,-3.93049712176217,-4.81977830800539));
#33658=CARTESIAN_POINT('Ctrl Pts',(99.060174424135,-2.50596446867118,-5.9814752025556));
#33659=CARTESIAN_POINT('Ctrl Pts',(99.1189741756087,-0.549389021423501,
-6.46189408921017));
#33660=CARTESIAN_POINT('Ctrl Pts',(99.1777739270824,1.25118869866473,-6.09209302315991));
#33661=CARTESIAN_POINT('Ctrl Pts',(99.2365736785561,3.05176641875296,-5.72229195710965));
#33662=CARTESIAN_POINT('Ctrl Pts',(99.2953734300298,4.66061422074918,-4.50960958425234));
#33663=CARTESIAN_POINT('Ctrl Pts',(99.3541731815035,5.51197192302534,-2.88049233331393));
#33664=CARTESIAN_POINT('Ctrl Pts',(99.4129729329772,6.3633296253015,-1.25137508237553));
#33665=CARTESIAN_POINT('Ctrl Pts',(99.4717726844509,6.4403021637733,0.761847462637341));
#33666=CARTESIAN_POINT('Ctrl Pts',(99.5305724359246,5.71582172177585,2.45121451680089));
#33667=CARTESIAN_POINT('Ctrl Pts',(99.5893721873983,4.99134127977839,4.14058157096443));
#33668=CARTESIAN_POINT('Ctrl Pts',(99.648171938872,3.47978506146762,5.47256790209284));
#33669=CARTESIAN_POINT('Ctrl Pts',(99.7069716903457,1.71270012775968,5.97877318811075));
#33670=CARTESIAN_POINT('Ctrl Pts',(99.7657714418194,-0.0543848059482521,
6.48497847412865));
#33671=CARTESIAN_POINT('Ctrl Pts',(99.8245711932931,-2.04193092337123,6.15535714814424));
#33672=CARTESIAN_POINT('Ctrl Pts',(99.8833709447668,-3.55100669662196,5.1058223630524));
#33673=CARTESIAN_POINT('Ctrl Pts',(99.9421706962405,-5.06008246987269,4.05628757796056));
#33674=CARTESIAN_POINT('Ctrl Pts',(100.000970447714,-6.06074051980728,2.30766719190532));
#33675=CARTESIAN_POINT('Ctrl Pts',(100.059770199188,-6.20109393743652,0.474873184743078));
#33676=CARTESIAN_POINT('Ctrl Pts',(100.064838605539,-6.21319208641561,0.316890462831652));
#33677=CARTESIAN_POINT('Ctrl Pts',(100.069907011889,-6.21924999999986,0.158445276461531));
#33678=CARTESIAN_POINT('Ctrl Pts',(100.07497541824,-6.21925,5.38891663729445E-12));
#33679=CARTESIAN_POINT('Ctrl Pts',(99.0714645817595,-6.21191492285883,-0.00676697184800665));
#33680=CARTESIAN_POINT('Ctrl Pts',(99.0947829804711,-6.2167521851182,-0.737717910543499));
#33681=CARTESIAN_POINT('Ctrl Pts',(99.1842719139968,-5.76013513448276,-3.5356653242606));
#33682=CARTESIAN_POINT('Ctrl Pts',(99.3068461149296,-2.49850315059143,-6.3860455449202));
#33683=CARTESIAN_POINT('Ctrl Pts',(99.4391871845576,1.77733710574879,-6.22281389700046));
#33684=CARTESIAN_POINT('Ctrl Pts',(99.5384429867787,4.54827162108827,-4.63000641769442));
#33685=CARTESIAN_POINT('Ctrl Pts',(99.6376987889997,6.19017426763678,-1.8878777821833));
#33686=CARTESIAN_POINT('Ctrl Pts',(99.7700398586277,6.4295287824728,2.38437734653381));
#33687=CARTESIAN_POINT('Ctrl Pts',(99.9354661956629,2.66165501182151,6.85409228541916));
#33688=CARTESIAN_POINT('Ctrl Pts',(100.130302859176,-4.19448567590115,5.96364365419648));
#33689=CARTESIAN_POINT('Ctrl Pts',(100.258968987875,-6.22176683696992,1.94454851646174));
#33690=CARTESIAN_POINT('Ctrl Pts',(100.32146458176,-6.22909731479716,-0.00146034420741566));
#33691=CARTESIAN_POINT('Origin',(28.1999754182402,0.,0.));
#33692=CARTESIAN_POINT('',(97.5749754182402,-6.22946104778866,0.003031573280016));
#33693=CARTESIAN_POINT('',(97.8214645817595,-6.21908492321965,0.000146043508555585));
#33694=CARTESIAN_POINT('',(28.1999754182402,-6.21925,5.68729293530136E-12));
#33695=CARTESIAN_POINT('Ctrl Pts',(97.5749754182402,-6.22946104778865,0.00303157328001538));
#33696=CARTESIAN_POINT('Ctrl Pts',(97.6389499763434,-6.22390252582942,-1.98595495917002));
#33697=CARTESIAN_POINT('Ctrl Pts',(97.7690950692605,-4.10935756144167,-6.05247427775012));
#33698=CARTESIAN_POINT('Ctrl Pts',(97.9654106969916,2.80531182390014,-6.79636004547279));
#33699=CARTESIAN_POINT('Ctrl Pts',(98.1639223014338,7.23361860234148,-1.31823760182156));
#33700=CARTESIAN_POINT('Ctrl Pts',(98.3293486384688,5.39619172482621,4.2314548992311));
#33701=CARTESIAN_POINT('Ctrl Pts',(98.4616897080969,1.63023388960724,6.26296075744928));
#33702=CARTESIAN_POINT('Ctrl Pts',(98.5609455103179,-1.56567653366841,6.29860231789631));
#33703=CARTESIAN_POINT('Ctrl Pts',(98.6602013125392,-4.37293411252434,4.77072187742011));
#33704=CARTESIAN_POINT('Ctrl Pts',(98.7482112818464,-5.95333417220565,2.40432899867917));
#33705=CARTESIAN_POINT('Ctrl Pts',(98.8031359837468,-6.21472755727631,0.685712634539138));
#33706=CARTESIAN_POINT('Ctrl Pts',(98.8249754182402,-6.21007513781392,0.00160019136293106));
#33707=CARTESIAN_POINT('Ctrl Pts',(97.8214645817595,-6.21925,4.99926393374325E-12));
#33708=CARTESIAN_POINT('Ctrl Pts',(97.8802643332332,-6.21925000000148,-1.83816020915241));
#33709=CARTESIAN_POINT('Ctrl Pts',(97.9390640847069,-5.35502977485312,-3.65808141345517));
#33710=CARTESIAN_POINT('Ctrl Pts',(97.9978638361806,-3.93049712176224,-4.81977830800533));
#33711=CARTESIAN_POINT('Ctrl Pts',(98.0566635876543,-2.50596446867137,-5.98147520255549));
#33712=CARTESIAN_POINT('Ctrl Pts',(98.115463339128,-0.549389021423854,-6.46189408921011));
#33713=CARTESIAN_POINT('Ctrl Pts',(98.1742630906017,1.25118869866429,-6.09209302316));
#33714=CARTESIAN_POINT('Ctrl Pts',(98.2330628420754,3.05176641875243,-5.72229195710989));
#33715=CARTESIAN_POINT('Ctrl Pts',(98.2918625935491,4.66061422074865,-4.50960958425284));
#33716=CARTESIAN_POINT('Ctrl Pts',(98.3506623450228,5.51197192302497,-2.88049233331465));
#33717=CARTESIAN_POINT('Ctrl Pts',(98.4094620964965,6.36332962530128,-1.25137508237646));
#33718=CARTESIAN_POINT('Ctrl Pts',(98.4682618479702,6.4403021637734,0.761847462636249));
#33719=CARTESIAN_POINT('Ctrl Pts',(98.5270615994439,5.7158217217763,2.45121451679982));
#33720=CARTESIAN_POINT('Ctrl Pts',(98.5858613509176,4.99134127977921,4.14058157096339));
#33721=CARTESIAN_POINT('Ctrl Pts',(98.6446611023913,3.47978506146883,5.47256790209203));
#33722=CARTESIAN_POINT('Ctrl Pts',(98.703460853865,1.71270012776114,5.97877318811033));
#33723=CARTESIAN_POINT('Ctrl Pts',(98.7622606053387,-0.0543848059465626,
6.48497847412864));
#33724=CARTESIAN_POINT('Ctrl Pts',(98.8210603568124,-2.04193092336948,6.15535714814478));
#33725=CARTESIAN_POINT('Ctrl Pts',(98.8798601082861,-3.55100669662043,5.10582236305346));
#33726=CARTESIAN_POINT('Ctrl Pts',(98.9386598597598,-5.06008246987137,4.05628757796215));
#33727=CARTESIAN_POINT('Ctrl Pts',(98.9974596112335,-6.06074051980647,2.30766719190737));
#33728=CARTESIAN_POINT('Ctrl Pts',(99.0562593627072,-6.20109393743635,0.47487318474529));
#33729=CARTESIAN_POINT('Ctrl Pts',(99.061327769058,-6.21319208641557,0.316890462832929));
#33730=CARTESIAN_POINT('Ctrl Pts',(99.0663961754087,-6.21924999999988,0.158445276461865));
#33731=CARTESIAN_POINT('Ctrl Pts',(99.0714645817595,-6.21925,4.77983506519556E-12));
#33732=CARTESIAN_POINT('Origin',(28.1999754182402,0.,0.));
#33733=CARTESIAN_POINT('',(96.3249754182403,-6.21661354691106,-0.00511547088340806));
#33734=CARTESIAN_POINT('',(96.5714645817595,-6.22727089829113,0.000782417097775698));
#33735=CARTESIAN_POINT('',(28.1999754182402,-6.21925,5.68729293530136E-12));
#33736=CARTESIAN_POINT('Ctrl Pts',(96.3249754182403,-6.21661354691106,-0.00511547088340718));
#33737=CARTESIAN_POINT('Ctrl Pts',(96.3424228993118,-6.22171682457446,-0.551217455118361));
#33738=CARTESIAN_POINT('Ctrl Pts',(96.4260409151973,-5.90739062850722,-3.16292774537146));
#33739=CARTESIAN_POINT('Ctrl Pts',(96.5758294658966,-2.24400282214668,-7.00176660787908));
#33740=CARTESIAN_POINT('Ctrl Pts',(96.7743410703392,4.67420254334854,-5.67580999001474));
#33741=CARTESIAN_POINT('Ctrl Pts',(96.9397674073738,6.85281755654995,-0.250972572108975));
#33742=CARTESIAN_POINT('Ctrl Pts',(97.0721084770024,5.28760290966167,3.73143343152621));
#33743=CARTESIAN_POINT('Ctrl Pts',(97.171364279223,2.86956225427671,5.82145571450295));
#33744=CARTESIAN_POINT('Ctrl Pts',(97.2706200814443,-0.260798927335446,
6.46639960903085));
#33745=CARTESIAN_POINT('Ctrl Pts',(97.4029611510722,-4.37268362577514,5.28239847078841));
#33746=CARTESIAN_POINT('Ctrl Pts',(97.5044129300043,-6.19766708457246,2.19647310644682));
#33747=CARTESIAN_POINT('Ctrl Pts',(97.5727794415293,-6.22965184839958,0.0713050906459493));
#33748=CARTESIAN_POINT('Ctrl Pts',(97.5749754182402,-6.22946104778865,0.00303157328001538));
#33749=CARTESIAN_POINT('Ctrl Pts',(96.5714645817595,-6.22727089829113,0.000782417097776149));
#33750=CARTESIAN_POINT('Ctrl Pts',(96.600984628629,-6.22650045475056,-0.92035981733023));
#33751=CARTESIAN_POINT('Ctrl Pts',(96.6635899429056,-5.76619445014441,-2.87893556911145));
#33752=CARTESIAN_POINT('Ctrl Pts',(96.7592805245889,-3.80654732511578,-5.25679861025155));
#33753=CARTESIAN_POINT('Ctrl Pts',(96.8585363268103,-0.828976761999734,
-6.41834382938761));
#33754=CARTESIAN_POINT('Ctrl Pts',(96.990877396438,3.4233566459321,-5.94177793005278));
#33755=CARTESIAN_POINT('Ctrl Pts',(97.1563037334735,7.20202000654271,-1.48118070617854));
#33756=CARTESIAN_POINT('Ctrl Pts',(97.3548153379154,5.14238247907462,5.25511053508099));
#33757=CARTESIAN_POINT('Ctrl Pts',(97.5533269423575,-1.62397116860792,7.17098333149248));
#33758=CARTESIAN_POINT('Ctrl Pts',(97.7088766903056,-5.76557152816693,3.52220956672017));
#33759=CARTESIAN_POINT('Ctrl Pts',(97.7982559034396,-6.2172889394232,0.732667319618331));
#33760=CARTESIAN_POINT('Ctrl Pts',(97.8214645817595,-6.21180884511622,0.0065831931557591));
#33761=CARTESIAN_POINT('Origin',(28.1999754182402,0.,0.));
#33762=CARTESIAN_POINT('',(95.0749754182402,-6.21121305788863,0.0018572188690421));
#33763=CARTESIAN_POINT('',(95.3214645817595,-6.21743435837855,-0.00353071204778788));
#33764=CARTESIAN_POINT('',(28.1999754182402,-6.21925,5.68729293530136E-12));
#33765=CARTESIAN_POINT('Ctrl Pts',(95.0749754182402,-6.21121305788863,0.00185721886904223));
#33766=CARTESIAN_POINT('Ctrl Pts',(95.1120663570942,-6.2079342228646,-1.16163168635908));
#33767=CARTESIAN_POINT('Ctrl Pts',(95.2153278307623,-5.33382860132951,-4.40534107097937));
#33768=CARTESIAN_POINT('Ctrl Pts',(95.384759839244,-0.0932801621545284,
-7.35216208134352));
#33769=CARTESIAN_POINT('Ctrl Pts',(95.5501861762794,5.07221142391009,-4.61484203049959));
#33770=CARTESIAN_POINT('Ctrl Pts',(95.6825272459072,6.44713844549368,-0.562801784655363));
#33771=CARTESIAN_POINT('Ctrl Pts',(95.7817830481286,5.94923618490345,2.59428660392868));
#33772=CARTESIAN_POINT('Ctrl Pts',(95.8810388503493,3.97453618501874,5.10738701276399));
#33773=CARTESIAN_POINT('Ctrl Pts',(96.0133799199776,0.069653856197323,6.85705797231051));
#33774=CARTESIAN_POINT('Ctrl Pts',(96.161358775941,-4.86882509062783,5.13720229160962));
#33775=CARTESIAN_POINT('Ctrl Pts',(96.2762523644977,-6.2023623624084,1.51990445707891));
#33776=CARTESIAN_POINT('Ctrl Pts',(96.3249754182403,-6.21661354691106,-0.00511547088340718));
#33777=CARTESIAN_POINT('Ctrl Pts',(95.3214645817595,-6.21743435837855,-0.00353071204778815));
#33778=CARTESIAN_POINT('Ctrl Pts',(95.3375428190044,-6.2188023314762,-0.505805742142214));
#33779=CARTESIAN_POINT('Ctrl Pts',(95.3867063236564,-6.03922426887351,-2.03954346570472));
#33780=CARTESIAN_POINT('Ctrl Pts',(95.4689550957154,-4.77589237691392,-4.36728657043583));
#33781=CARTESIAN_POINT('Ctrl Pts',(95.6012961653434,-1.22034872738306,-6.74795114674706));
#33782=CARTESIAN_POINT('Ctrl Pts',(95.7667225023786,4.544895881605,-5.77987109582617));
#33783=CARTESIAN_POINT('Ctrl Pts',(95.9652341068206,7.31967546924895,0.694719599470295));
#33784=CARTESIAN_POINT('Ctrl Pts',(96.1637457112627,3.388114636821,6.52540906800271));
#33785=CARTESIAN_POINT('Ctrl Pts',(96.3622573157049,-3.65451648904094,6.38024276108088));
#33786=CARTESIAN_POINT('Ctrl Pts',(96.4981636058704,-6.16747960465473,2.28738448867254));
#33787=CARTESIAN_POINT('Ctrl Pts',(96.567899361222,-6.22736394696229,0.112031400768883));
#33788=CARTESIAN_POINT('Ctrl Pts',(96.5714645817595,-6.22727089829113,0.000782417097776149));
#33789=CARTESIAN_POINT('Origin',(28.1999754182402,0.,0.));
#33790=CARTESIAN_POINT('',(93.8249754182403,-6.22441105920928,0.00468493321960073));
#33791=CARTESIAN_POINT('',(94.0714645817596,-6.21573536891404,0.00197485669535868));
#33792=CARTESIAN_POINT('',(28.1999754182402,-6.21925,5.68729293530136E-12));
#33793=CARTESIAN_POINT('Ctrl Pts',(93.8249754182403,-6.22441105920928,0.00468493321960094));
#33794=CARTESIAN_POINT('Ctrl Pts',(93.8817098148766,-6.20866265984911,-1.76545450189424));
#33795=CARTESIAN_POINT('Ctrl Pts',(94.0046147463269,-4.49086526416891,-5.62631371215349));
#33796=CARTESIAN_POINT('Ctrl Pts',(94.1606049451846,0.895521517553394,-6.7986864103964));
#33797=CARTESIAN_POINT('Ctrl Pts',(94.2929460148125,4.56108251734731,-4.59117264477413));
#33798=CARTESIAN_POINT('Ctrl Pts',(94.3922018170336,6.21852484226242,-1.85840871534061));
#33799=CARTESIAN_POINT('Ctrl Pts',(94.4914576192548,6.33232305163478,1.33567389504654));
#33800=CARTESIAN_POINT('Ctrl Pts',(94.6237986888826,4.47908725340983,5.19248236122677));
#33801=CARTESIAN_POINT('Ctrl Pts',(94.7892250259181,-0.978642878797454,
7.28733466877817));
#33802=CARTESIAN_POINT('Ctrl Pts',(94.9506456915058,-5.59666748377655,3.89861203888041));
#33803=CARTESIAN_POINT('Ctrl Pts',(95.04589582228,-6.21378369105847,0.914041927951374));
#33804=CARTESIAN_POINT('Ctrl Pts',(95.0749754182402,-6.21121305788863,0.00185721886904223));
#33805=CARTESIAN_POINT('Ctrl Pts',(94.0714645817595,-6.21573536891404,0.00197485669535951));
#33806=CARTESIAN_POINT('Ctrl Pts',(94.0741010093799,-6.21584226203414,-0.0805910237340283));
#33807=CARTESIAN_POINT('Ctrl Pts',(94.1098227044073,-6.1954099144712,-1.19952608424165));
#33808=CARTESIAN_POINT('Ctrl Pts',(94.2117149342486,-5.2875683157848,-4.36643069350914));
#33809=CARTESIAN_POINT('Ctrl Pts',(94.3771412712839,-0.259211159662201,
-7.34818331519461));
#33810=CARTESIAN_POINT('Ctrl Pts',(94.5756528757259,6.03919547739302,-4.19385291621541));
#33811=CARTESIAN_POINT('Ctrl Pts',(94.7741644801679,6.79967439427966,2.79726874447026));
#33812=CARTESIAN_POINT('Ctrl Pts',(94.9726760846102,1.32679513771092,7.23205386605656));
#33813=CARTESIAN_POINT('Ctrl Pts',(95.1381024216451,-4.22506743128341,5.40119439535534));
#33814=CARTESIAN_POINT('Ctrl Pts',(95.2543652540283,-6.01367690893417,2.09488009192008));
#33815=CARTESIAN_POINT('Ctrl Pts',(95.3044575515974,-6.21598736146102,0.527759283015377));
#33816=CARTESIAN_POINT('Ctrl Pts',(95.3214645817595,-6.21743435837855,-0.00353071204778815));
#33817=CARTESIAN_POINT('Origin',(28.1999754182402,0.,0.));
#33818=CARTESIAN_POINT('',(92.5749754182402,-6.22408856974339,-0.00719918589093503));
#33819=CARTESIAN_POINT('',(92.8214645817595,-6.21925,4.46288405536732E-12));
#33820=CARTESIAN_POINT('',(28.1999754182402,-6.21925,5.68729293530136E-12));
#33821=CARTESIAN_POINT('Ctrl Pts',(92.5749754182402,-6.22408856974339,-0.00719918589093541));
#33822=CARTESIAN_POINT('Ctrl Pts',(92.585182737845,-6.2268665635629,-0.325414501277245));
#33823=CARTESIAN_POINT('Ctrl Pts',(92.6615605922639,-6.06021962183329,-2.70283095786737));
#33824=CARTESIAN_POINT('Ctrl Pts',(92.7710237140898,-3.7042076507531,-5.7708700709176));
#33825=CARTESIAN_POINT('Ctrl Pts',(92.9033647837178,0.520397198382932,-6.45069970934075));
#33826=CARTESIAN_POINT('Ctrl Pts',(93.0026205859388,3.55021779910258,-5.43320234723718));
#33827=CARTESIAN_POINT('Ctrl Pts',(93.10187638816,5.69875659207993,-3.06700395963218));
#33828=CARTESIAN_POINT('Ctrl Pts',(93.2342174577878,6.77262535525563,1.0750076709765));
#33829=CARTESIAN_POINT('Ctrl Pts',(93.3996437948232,3.95611714926058,6.19775165365016));
#33830=CARTESIAN_POINT('Ctrl Pts',(93.5981553992651,-3.07146236840367,6.6802996352329));
#33831=CARTESIAN_POINT('Ctrl Pts',(93.739932607071,-6.07575174174706,2.65538258240216));
#33832=CARTESIAN_POINT('Ctrl Pts',(93.8155392800626,-6.22703035334564,0.29909681196911));
#33833=CARTESIAN_POINT('Ctrl Pts',(93.8249754182403,-6.22441105920928,0.00468493321960094));
#33834=CARTESIAN_POINT('Ctrl Pts',(92.8214645817596,-6.2195957732021,0.00304117013771654));
#33835=CARTESIAN_POINT('Ctrl Pts',(92.8768297345694,-6.20322707436264,-1.72625245001619));
#33836=CARTESIAN_POINT('Ctrl Pts',(92.9983654221932,-4.56818868445748,-5.53539594499472));
#33837=CARTESIAN_POINT('Ctrl Pts',(93.1860716446312,1.90583395511156,-7.10127321207659));
#33838=CARTESIAN_POINT('Ctrl Pts',(93.3845832490731,6.99910671440612,-2.25228539429799));
#33839=CARTESIAN_POINT('Ctrl Pts',(93.5830948535154,5.68133630187344,4.66748393505667));
#33840=CARTESIAN_POINT('Ctrl Pts',(93.7485211905503,0.259080310101639,6.85251582181516));
#33841=CARTESIAN_POINT('Ctrl Pts',(93.8808622601785,-3.72517479045193,5.29201405560826));
#33842=CARTESIAN_POINT('Ctrl Pts',(93.9774816347792,-5.76246549727055,2.94061004980632));
#33843=CARTESIAN_POINT('Ctrl Pts',(94.0410157419728,-6.21450083038052,0.955551296889638));
#33844=CARTESIAN_POINT('Ctrl Pts',(94.0714645817595,-6.21573536891404,0.00197485669535951));
#33845=CARTESIAN_POINT('Origin',(28.1999754182402,0.,0.));
#33846=CARTESIAN_POINT('',(91.3249754182403,-6.21873749421801,7.04867538213377E-5));
#33847=CARTESIAN_POINT('',(91.5714645817596,-6.21925,3.97526767998117E-12));
#33848=CARTESIAN_POINT('',(28.1999754182402,-6.21925,5.68729293530136E-12));
#33849=CARTESIAN_POINT('Ctrl Pts',(91.3249754182402,-6.20685969906364,0.00170408232238357));
#33850=CARTESIAN_POINT('Ctrl Pts',(91.3548261956275,-6.20822254272067,-0.934201698018358));
#33851=CARTESIAN_POINT('Ctrl Pts',(91.4177622404217,-5.78895833438908,-2.90776862535172));
#33852=CARTESIAN_POINT('Ctrl Pts',(91.513783552623,-3.76612079172275,-5.26295298918085));
#33853=CARTESIAN_POINT('Ctrl Pts',(91.613039354844,-0.795191902178077,-6.44138215026858));
#33854=CARTESIAN_POINT('Ctrl Pts',(91.7122951570653,2.37312999160159,-6.02084662046249));
#33855=CARTESIAN_POINT('Ctrl Pts',(91.844636226693,5.86681383167074,-3.55029451733617));
#33856=CARTESIAN_POINT('Ctrl Pts',(92.0100625637283,7.0220299791157,2.18038607393216));
#33857=CARTESIAN_POINT('Ctrl Pts',(92.2085741681705,1.9658051306551,7.08490610278661));
#33858=CARTESIAN_POINT('Ctrl Pts',(92.3968784530076,-4.53235594076636,5.57726581121151));
#33859=CARTESIAN_POINT('Ctrl Pts',(92.519012203031,-6.20885778712949,1.73746570825861));
#33860=CARTESIAN_POINT('Ctrl Pts',(92.5749754182402,-6.22408856974339,-0.00719918589093541));
#33861=CARTESIAN_POINT('Ctrl Pts',(91.5714645817595,-6.21925,4.32879111273125E-12));
#33862=CARTESIAN_POINT('Ctrl Pts',(91.6302643332332,-6.21925000000128,-1.83816020915308));
#33863=CARTESIAN_POINT('Ctrl Pts',(91.6890640847069,-5.35502977485273,-3.65808141345575));
#33864=CARTESIAN_POINT('Ctrl Pts',(91.7478638361806,-3.93049712176173,-4.81977830800575));
#33865=CARTESIAN_POINT('Ctrl Pts',(91.8066635876543,-2.50596446867072,-5.98147520255576));
#33866=CARTESIAN_POINT('Ctrl Pts',(91.865463339128,-0.549389021423158,-6.46189408921017));
#33867=CARTESIAN_POINT('Ctrl Pts',(91.9242630906017,1.25118869866495,-6.09209302315987));
#33868=CARTESIAN_POINT('Ctrl Pts',(91.9830628420754,3.05176641875305,-5.72229195710956));
#33869=CARTESIAN_POINT('Ctrl Pts',(92.0418625935491,4.66061422074914,-4.50960958425234));
#33870=CARTESIAN_POINT('Ctrl Pts',(92.1006623450228,5.51197192302528,-2.88049233331405));
#33871=CARTESIAN_POINT('Ctrl Pts',(92.1594620964965,6.36332962530141,-1.25137508237577));
#33872=CARTESIAN_POINT('Ctrl Pts',(92.2182618479702,6.44030216377332,0.761847462636944));
#33873=CARTESIAN_POINT('Ctrl Pts',(92.2770615994439,5.71582172177604,2.45121451680044));
#33874=CARTESIAN_POINT('Ctrl Pts',(92.3358613509176,4.99134127977876,4.14058157096393));
#33875=CARTESIAN_POINT('Ctrl Pts',(92.3946611023913,3.47978506146824,5.4725679020924));
#33876=CARTESIAN_POINT('Ctrl Pts',(92.453460853865,1.71270012776049,5.97877318811052));
#33877=CARTESIAN_POINT('Ctrl Pts',(92.5122606053387,-0.0543848059472618,
6.48497847412863));
#33878=CARTESIAN_POINT('Ctrl Pts',(92.5710603568124,-2.04193092337015,6.15535714814456));
#33879=CARTESIAN_POINT('Ctrl Pts',(92.6298601082861,-3.55100669662098,5.10582236305308));
#33880=CARTESIAN_POINT('Ctrl Pts',(92.6886598597598,-5.06008246987181,4.0562875779616));
#33881=CARTESIAN_POINT('Ctrl Pts',(92.7474596112335,-6.06074051980672,2.30766719190671));
#33882=CARTESIAN_POINT('Ctrl Pts',(92.8062593627072,-6.2010939374364,0.474873184744622));
#33883=CARTESIAN_POINT('Ctrl Pts',(92.811327769058,-6.2131920864156,0.316890462832376));
#33884=CARTESIAN_POINT('Ctrl Pts',(92.8163961754088,-6.21924999999989,0.15844527646143));
#33885=CARTESIAN_POINT('Ctrl Pts',(92.8214645817595,-6.21925,4.46288567693365E-12));
#33886=CARTESIAN_POINT('Origin',(28.1999754182402,0.,0.));
#33887=CARTESIAN_POINT('',(90.0749754182402,-6.21925,3.96263669092518E-12));
#33888=CARTESIAN_POINT('',(90.3214645817596,-6.2089008876497,-0.000864123173838216));
#33889=CARTESIAN_POINT('',(28.1999754182402,-6.21925,5.68729293530136E-12));
#33890=CARTESIAN_POINT('Ctrl Pts',(90.0749754182402,-6.21925,4.31616012367526E-12));
#33891=CARTESIAN_POINT('Ctrl Pts',(90.1337751697139,-6.21925000000128,-1.83816020915309));
#33892=CARTESIAN_POINT('Ctrl Pts',(90.1925749211876,-5.35502977485272,-3.65808141345576));
#33893=CARTESIAN_POINT('Ctrl Pts',(90.2513746726613,-3.93049712176172,-4.81977830800576));
#33894=CARTESIAN_POINT('Ctrl Pts',(90.310174424135,-2.50596446867071,-5.98147520255577));
#33895=CARTESIAN_POINT('Ctrl Pts',(90.3689741756087,-0.549389021423145,
-6.46189408921017));
#33896=CARTESIAN_POINT('Ctrl Pts',(90.4277739270824,1.25118869866496,-6.09209302315986));
#33897=CARTESIAN_POINT('Ctrl Pts',(90.4865736785561,3.05176641875306,-5.72229195710956));
#33898=CARTESIAN_POINT('Ctrl Pts',(90.5453734300298,4.66061422074915,-4.50960958425233));
#33899=CARTESIAN_POINT('Ctrl Pts',(90.6041731815035,5.51197192302528,-2.88049233331404));
#33900=CARTESIAN_POINT('Ctrl Pts',(90.6629729329772,6.36332962530142,-1.25137508237576));
#33901=CARTESIAN_POINT('Ctrl Pts',(90.7217726844509,6.44030216377332,0.761847462636957));
#33902=CARTESIAN_POINT('Ctrl Pts',(90.7805724359246,5.71582172177603,2.45121451680045));
#33903=CARTESIAN_POINT('Ctrl Pts',(90.8393721873983,4.99134127977875,4.14058157096394));
#33904=CARTESIAN_POINT('Ctrl Pts',(90.898171938872,3.47978506146823,5.47256790209241));
#33905=CARTESIAN_POINT('Ctrl Pts',(90.9569716903457,1.71270012776048,5.97877318811052));
#33906=CARTESIAN_POINT('Ctrl Pts',(91.0157714418194,-0.0543848059472749,
6.48497847412863));
#33907=CARTESIAN_POINT('Ctrl Pts',(91.0745711932931,-2.04193092337016,6.15535714814456));
#33908=CARTESIAN_POINT('Ctrl Pts',(91.1333709447668,-3.55100669662099,5.10582236305308));
#33909=CARTESIAN_POINT('Ctrl Pts',(91.1921706962405,-5.06008246987182,4.05628757796159));
#33910=CARTESIAN_POINT('Ctrl Pts',(91.2509704477142,-6.06074051980672,2.3076671919067));
#33911=CARTESIAN_POINT('Ctrl Pts',(91.3097701991879,-6.2010939374364,0.474873184744609));
#33912=CARTESIAN_POINT('Ctrl Pts',(91.3148386055387,-6.21319208641561,0.316890462832246));
#33913=CARTESIAN_POINT('Ctrl Pts',(91.3199070118895,-6.2192499999999,0.158445276461182));
#33914=CARTESIAN_POINT('Ctrl Pts',(91.3249754182402,-6.21925,4.09673125512758E-12));
#33915=CARTESIAN_POINT('Ctrl Pts',(90.3214645817596,-6.2089008876497,-0.000864123173838147));
#33916=CARTESIAN_POINT('Ctrl Pts',(90.3499461153202,-6.2120955723698,-0.895010566629414));
#33917=CARTESIAN_POINT('Ctrl Pts',(90.444598183695,-5.61492052568028,-3.86345977911135));
#33918=CARTESIAN_POINT('Ctrl Pts',(90.6054207868836,-1.05335843212328,-7.27672455920159));
#33919=CARTESIAN_POINT('Ctrl Pts',(90.8039323913257,5.54969193399755,-4.82326734659396));
#33920=CARTESIAN_POINT('Ctrl Pts',(90.9693587283609,6.79974118846012,0.887477022389232));
#33921=CARTESIAN_POINT('Ctrl Pts',(91.1016997979888,4.59656587779412,4.55564727731113));
#33922=CARTESIAN_POINT('Ctrl Pts',(91.20095560021,1.86576486459037,6.21632171280966));
#33923=CARTESIAN_POINT('Ctrl Pts',(91.300211402431,-1.32818086979205,6.33389892256676));
#33924=CARTESIAN_POINT('Ctrl Pts',(91.4237143962808,-4.92946548902491,4.60868661393506));
#33925=CARTESIAN_POINT('Ctrl Pts',(91.5141321227237,-6.21048370270169,1.78002491689768));
#33926=CARTESIAN_POINT('Ctrl Pts',(91.5714645817596,-6.22556524348756,-0.00419006153428332));
#33927=CARTESIAN_POINT('Origin',(28.1999754182402,0.,0.));
#33928=CARTESIAN_POINT('',(88.8249754182402,-6.22149727412722,-0.000986937928962441));
#33929=CARTESIAN_POINT('',(89.0714645817595,-6.21806379781386,0.00504561100484663));
#33930=CARTESIAN_POINT('',(28.1999754182402,-6.21925,5.68729293530136E-12));
#33931=CARTESIAN_POINT('Ctrl Pts',(88.8249754182402,-6.22149727412722,-0.00098693792896223));
#33932=CARTESIAN_POINT('Ctrl Pts',(88.8279425763783,-6.22164967457631,-0.0934599545148036));
#33933=CARTESIAN_POINT('Ctrl Pts',(88.8639950019234,-6.19761435895859,-1.21694528678682));
#33934=CARTESIAN_POINT('Ctrl Pts',(88.9331326948756,-5.54069632003458,-3.34410291009848));
#33935=CARTESIAN_POINT('Ctrl Pts',(89.0654737645036,-2.52204036811142,-6.37678665762986));
#33936=CARTESIAN_POINT('Ctrl Pts',(89.2309001015388,3.32104580709813,-6.56000329315107));
#33937=CARTESIAN_POINT('Ctrl Pts',(89.4294117059809,7.31354018950449,-0.7565805928752));
#33938=CARTESIAN_POINT('Ctrl Pts',(89.6279233104229,4.60386296928326,5.73277681905332));
#33939=CARTESIAN_POINT('Ctrl Pts',(89.8264349148652,-2.33008407920169,6.97378639211496));
#33940=CARTESIAN_POINT('Ctrl Pts',(89.9754522841373,-5.91329462628883,3.11473712707665));
#33941=CARTESIAN_POINT('Ctrl Pts',(90.0582991185959,-6.22469949224009,0.524291360883706));
#33942=CARTESIAN_POINT('Ctrl Pts',(90.0749754182403,-6.22196066299615,0.00227071514955785));
#33943=CARTESIAN_POINT('Ctrl Pts',(89.0714645817595,-6.21806379781386,0.0050456110048467));
#33944=CARTESIAN_POINT('Ctrl Pts',(89.1195895731026,-6.20545924076061,-1.50037252384037));
#33945=CARTESIAN_POINT('Ctrl Pts',(89.2338850992598,-4.89889388900873,-5.09517050824349));
#33946=CARTESIAN_POINT('Ctrl Pts',(89.4143511602309,1.12569445119592,-7.26607187285839));
#33947=CARTESIAN_POINT('Ctrl Pts',(89.5797774972661,5.76648339708804,-3.71103286517617));
#33948=CARTESIAN_POINT('Ctrl Pts',(89.7121185668941,6.45131090248977,0.512764686372355));
#33949=CARTESIAN_POINT('Ctrl Pts',(89.8113743691151,5.43739898593206,3.54378701883646));
#33950=CARTESIAN_POINT('Ctrl Pts',(89.9106301713363,3.07374429895899,5.69512387650968));
#33951=CARTESIAN_POINT('Ctrl Pts',(90.0429712409643,-1.06699388433329,6.77389251066956));
#33952=CARTESIAN_POINT('Ctrl Pts',(90.1799160444387,-5.31050817540945,4.44732299061749));
#33953=CARTESIAN_POINT('Ctrl Pts',(90.2837755805062,-6.20467343001778,1.18234064901073));
#33954=CARTESIAN_POINT('Ctrl Pts',(90.3214645817596,-6.2089008876497,-0.000864123173838147));
#33955=CARTESIAN_POINT('Origin',(28.1999754182402,0.,0.));
#33956=CARTESIAN_POINT('',(87.5749754182402,-6.21925,4.04797289438319E-12));
#33957=CARTESIAN_POINT('',(87.8214645817596,-6.22964168097674,-0.000350078226707407));
#33958=CARTESIAN_POINT('',(28.1999754182402,-6.21925,5.68729293530136E-12));
#33959=CARTESIAN_POINT('Ctrl Pts',(87.5749754182403,-6.21906914730504,-0.00133611460555415));
#33960=CARTESIAN_POINT('Ctrl Pts',(87.5975860341608,-6.22215116111062,-0.70980238469718));
#33961=CARTESIAN_POINT('Ctrl Pts',(87.6863671848953,-5.76713295026162,-3.49042167931515));
#33962=CARTESIAN_POINT('Ctrl Pts',(87.8413188704441,-1.69752736119953,-7.15411694879083));
#33963=CARTESIAN_POINT('Ctrl Pts',(88.0398304748858,5.0977681804467,-5.29840012413548));
#33964=CARTESIAN_POINT('Ctrl Pts',(88.2383420793283,7.21666225322758,1.40714967926411));
#33965=CARTESIAN_POINT('Ctrl Pts',(88.4368536837702,2.72150289496444,6.83054979131966));
#33966=CARTESIAN_POINT('Ctrl Pts',(88.6022800208054,-3.0818294938239,6.125881378733));
#33967=CARTESIAN_POINT('Ctrl Pts',(88.7316539322954,-5.75604940176151,2.90933191124067));
#33968=CARTESIAN_POINT('Ctrl Pts',(88.7948573089713,-6.2199503348794,0.93765950029407));
#33969=CARTESIAN_POINT('Ctrl Pts',(88.8249754182402,-6.22149727412722,-0.00098693792896223));
#33970=CARTESIAN_POINT('Ctrl Pts',(87.8214645817596,-6.22964168097674,-0.000350078226707528));
#33971=CARTESIAN_POINT('Ctrl Pts',(87.8230624960711,-6.22971496116889,-0.0500951023154418));
#33972=CARTESIAN_POINT('Ctrl Pts',(87.8908309451966,-6.20535244691635,-2.15974806597762));
#33973=CARTESIAN_POINT('Ctrl Pts',(88.0247699291361,-3.8300746758159,-6.27642545057859));
#33974=CARTESIAN_POINT('Ctrl Pts',(88.1901962661713,2.00917170803365,-6.55647197377879));
#33975=CARTESIAN_POINT('Ctrl Pts',(88.3225373357994,5.25849341829804,-3.77234502052638));
#33976=CARTESIAN_POINT('Ctrl Pts',(88.4217931380204,6.44043681020296,-0.802812469304661));
#33977=CARTESIAN_POINT('Ctrl Pts',(88.5210489402415,6.02365017597241,2.36600476366407));
#33978=CARTESIAN_POINT('Ctrl Pts',(88.6533900098694,3.55723335538306,5.86260919306929));
#33979=CARTESIAN_POINT('Ctrl Pts',(88.8188163469047,-2.17207643043537,7.02460478883646));
#33980=CARTESIAN_POINT('Ctrl Pts',(88.9692029600036,-5.89212743611744,3.19855472586929));
#33981=CARTESIAN_POINT('Ctrl Pts',(89.0534190382886,-6.22279015881442,0.56953586100025));
#33982=CARTESIAN_POINT('Ctrl Pts',(89.0714645817595,-6.21806379781386,0.0050456110048467));
#33983=CARTESIAN_POINT('Origin',(28.1999754182402,0.,0.));
#33984=CARTESIAN_POINT('',(86.3249754182403,-6.21883554189359,3.4186727807411E-5));
#33985=CARTESIAN_POINT('',(86.5714645817596,-6.21915084886221,-0.00012899831342565));
#33986=CARTESIAN_POINT('',(28.1999754182402,-6.21925,5.68729293530136E-12));
#33987=CARTESIAN_POINT('Ctrl Pts',(86.3249754182403,-6.21925,3.56035299831798E-12));
#33988=CARTESIAN_POINT('Ctrl Pts',(86.383775169714,-6.21925000000105,-1.83816020915385));
#33989=CARTESIAN_POINT('Ctrl Pts',(86.4425749211877,-5.35502977485227,-3.65808141345641));
#33990=CARTESIAN_POINT('Ctrl Pts',(86.5013746726614,-3.93049712176113,-4.81977830800624));
#33991=CARTESIAN_POINT('Ctrl Pts',(86.5601744241351,-2.50596446866999,-5.98147520255607));
#33992=CARTESIAN_POINT('Ctrl Pts',(86.6189741756087,-0.549389021422359,
-6.46189408921024));
#33993=CARTESIAN_POINT('Ctrl Pts',(86.6777739270824,1.2511886986657,-6.09209302315971));
#33994=CARTESIAN_POINT('Ctrl Pts',(86.7365736785561,3.05176641875376,-5.72229195710919));
#33995=CARTESIAN_POINT('Ctrl Pts',(86.7953734300298,4.66061422074969,-4.50960958425176));
#33996=CARTESIAN_POINT('Ctrl Pts',(86.8541731815035,5.51197192302563,-2.88049233331337));
#33997=CARTESIAN_POINT('Ctrl Pts',(86.9129729329772,6.36332962530157,-1.25137508237498));
#33998=CARTESIAN_POINT('Ctrl Pts',(86.9717726844509,6.44030216377322,0.76184746263774));
#33999=CARTESIAN_POINT('Ctrl Pts',(87.0305724359246,5.71582172177574,2.45121451680114));
#34000=CARTESIAN_POINT('Ctrl Pts',(87.0893721873983,4.99134127977825,4.14058157096455));
#34001=CARTESIAN_POINT('Ctrl Pts',(87.148171938872,3.47978506146757,5.47256790209283));
#34002=CARTESIAN_POINT('Ctrl Pts',(87.2069716903457,1.71270012775975,5.97877318811073));
#34003=CARTESIAN_POINT('Ctrl Pts',(87.2657714418194,-0.0543848059480628,
6.48497847412862));
#34004=CARTESIAN_POINT('Ctrl Pts',(87.3245711932931,-2.04193092337091,6.15535714814431));
#34005=CARTESIAN_POINT('Ctrl Pts',(87.3833709447668,-3.55100669662161,5.10582236305264));
#34006=CARTESIAN_POINT('Ctrl Pts',(87.4421706962405,-5.06008246987231,4.05628757796098));
#34007=CARTESIAN_POINT('Ctrl Pts',(87.5009704477142,-6.060740519807,2.30766719190597));
#34008=CARTESIAN_POINT('Ctrl Pts',(87.5597701991879,-6.20109393743646,0.474873184743856));
#34009=CARTESIAN_POINT('Ctrl Pts',(87.5648386055387,-6.21319208641563,0.316890462831726));
#34010=CARTESIAN_POINT('Ctrl Pts',(87.5699070118895,-6.2192499999999,0.158445276460897));
#34011=CARTESIAN_POINT('Ctrl Pts',(87.5749754182402,-6.21925,4.04797099527046E-12));
#34012=CARTESIAN_POINT('Ctrl Pts',(86.5714645817596,-6.21353584576935,-0.00743426924668888));
#34013=CARTESIAN_POINT('Ctrl Pts',(86.5927059538535,-6.21863854140484,-0.672800635959472));
#34014=CARTESIAN_POINT('Ctrl Pts',(86.6801178607615,-5.81430299723871,-3.40355548725215));
#34015=CARTESIAN_POINT('Ctrl Pts',(86.8006150350767,-2.69726124705009,-6.30467108265544));
#34016=CARTESIAN_POINT('Ctrl Pts',(86.9329561047044,1.58159360772959,-6.2754204356491));
#34017=CARTESIAN_POINT('Ctrl Pts',(87.0322119069257,4.40104898481893,-4.77016792160538));
#34018=CARTESIAN_POINT('Ctrl Pts',(87.1314677091467,6.1280180343697,-2.08080151735183));
#34019=CARTESIAN_POINT('Ctrl Pts',(87.2638087787747,6.501043828168,2.18186269951808));
#34020=CARTESIAN_POINT('Ctrl Pts',(87.4292351158099,2.87499030196175,6.76737905120017));
#34021=CARTESIAN_POINT('Ctrl Pts',(87.6261488059404,-4.07902303115758,6.0848730030111));
#34022=CARTESIAN_POINT('Ctrl Pts',(87.756891961257,-6.22668038699246,2.00987446213666));
#34023=CARTESIAN_POINT('Ctrl Pts',(87.8214645817596,-6.22964168097674,-0.000350078226707528));
#34024=CARTESIAN_POINT('Origin',(28.1999754182402,0.,0.));
#34025=CARTESIAN_POINT('',(85.0749754182403,-6.22858364363872,0.00435858369765019));
#34026=CARTESIAN_POINT('',(85.3214645817596,-6.21849213708592,0.0005147991858583));
#34027=CARTESIAN_POINT('',(28.1999754182402,-6.21925,5.68729293530136E-12));
#34028=CARTESIAN_POINT('Ctrl Pts',(85.0749754182403,-6.22858364363872,0.00435858369765025));
#34029=CARTESIAN_POINT('Ctrl Pts',(85.1368729497257,-6.21898881198671,-1.92103273188814));
#34030=CARTESIAN_POINT('Ctrl Pts',(85.2649410160251,-4.22400447196293,-5.93097583593628));
#34031=CARTESIAN_POINT('Ctrl Pts',(85.4591796171386,2.59110314784578,-6.88087703525041));
#34032=CARTESIAN_POINT('Ctrl Pts',(85.6576912215807,7.18878928721451,-1.54411691365224));
#34033=CARTESIAN_POINT('Ctrl Pts',(85.8231175586158,5.52605610955549,4.0603940165154));
#34034=CARTESIAN_POINT('Ctrl Pts',(85.9554586282439,1.82556334808452,6.2088371251229));
#34035=CARTESIAN_POINT('Ctrl Pts',(86.0547144304649,-1.36766347836997,6.34454338601461));
#34036=CARTESIAN_POINT('Ctrl Pts',(86.1539702326861,-4.22139086822476,4.90532354914965));
#34037=CARTESIAN_POINT('Ctrl Pts',(86.2440572286111,-5.91414893595505,2.5349313646869));
#34038=CARTESIAN_POINT('Ctrl Pts',(86.3010589571292,-6.21301106946328,0.75031761569158));
#34039=CARTESIAN_POINT('Ctrl Pts',(86.3249754182402,-6.20882463865616,0.000859939640229165));
#34040=CARTESIAN_POINT('Ctrl Pts',(85.3214645817596,-6.21925,3.65831829171925E-12));
#34041=CARTESIAN_POINT('Ctrl Pts',(85.3802643332333,-6.21925000000108,-1.83816020915375));
#34042=CARTESIAN_POINT('Ctrl Pts',(85.439064084707,-5.35502977485233,-3.65808141345632));
#34043=CARTESIAN_POINT('Ctrl Pts',(85.4978638361806,-3.93049712176121,-4.81977830800618));
#34044=CARTESIAN_POINT('Ctrl Pts',(85.5566635876543,-2.50596446867008,-5.98147520255603));
#34045=CARTESIAN_POINT('Ctrl Pts',(85.615463339128,-0.549389021422461,-6.46189408921023));
#34046=CARTESIAN_POINT('Ctrl Pts',(85.6742630906017,1.2511886986656,-6.09209302315973));
#34047=CARTESIAN_POINT('Ctrl Pts',(85.7330628420754,3.05176641875367,-5.72229195710924));
#34048=CARTESIAN_POINT('Ctrl Pts',(85.7918625935491,4.66061422074962,-4.50960958425183));
#34049=CARTESIAN_POINT('Ctrl Pts',(85.8506623450228,5.51197192302559,-2.88049233331346));
#34050=CARTESIAN_POINT('Ctrl Pts',(85.9094620964965,6.36332962530155,-1.25137508237509));
#34051=CARTESIAN_POINT('Ctrl Pts',(85.9682618479702,6.44030216377323,0.761847462637638));
#34052=CARTESIAN_POINT('Ctrl Pts',(86.0270615994439,5.71582172177577,2.45121451680105));
#34053=CARTESIAN_POINT('Ctrl Pts',(86.0858613509176,4.99134127977831,4.14058157096447));
#34054=CARTESIAN_POINT('Ctrl Pts',(86.1446611023913,3.47978506146765,5.47256790209278));
#34055=CARTESIAN_POINT('Ctrl Pts',(86.203460853865,1.71270012775985,5.9787731881107));
#34056=CARTESIAN_POINT('Ctrl Pts',(86.2622606053387,-0.0543848059479607,
6.48497847412862));
#34057=CARTESIAN_POINT('Ctrl Pts',(86.3210603568124,-2.04193092337081,6.15535714814434));
#34058=CARTESIAN_POINT('Ctrl Pts',(86.3798601082861,-3.55100669662153,5.1058223630527));
#34059=CARTESIAN_POINT('Ctrl Pts',(86.4386598597598,-5.06008246987225,4.05628757796106));
#34060=CARTESIAN_POINT('Ctrl Pts',(86.4974596112335,-6.06074051980697,2.30766719190606));
#34061=CARTESIAN_POINT('Ctrl Pts',(86.5562593627072,-6.20109393743645,0.474873184743953));
#34062=CARTESIAN_POINT('Ctrl Pts',(86.561327769058,-6.21319208641564,0.316890462831589));
#34063=CARTESIAN_POINT('Ctrl Pts',(86.5663961754088,-6.21924999999991,0.158445276460524));
#34064=CARTESIAN_POINT('Ctrl Pts',(86.5714645817596,-6.21925,3.43888942317157E-12));
#34065=CARTESIAN_POINT('Origin',(28.1999754182402,0.,0.));
#34066=CARTESIAN_POINT('',(83.8249754182403,-6.21863967025274,-0.0053269228922874));
#34067=CARTESIAN_POINT('',(84.0714645817596,-6.22691982511773,0.00134582525012354));
#34068=CARTESIAN_POINT('',(28.1999754182402,-6.21925,5.68729293530136E-12));
#34069=CARTESIAN_POINT('Ctrl Pts',(83.8249754182403,-6.21863967025274,-0.00532692289228712));
#34070=CARTESIAN_POINT('Ctrl Pts',(83.8403458726941,-6.22330610280407,-0.48602639124095));
#34071=CARTESIAN_POINT('Ctrl Pts',(83.921886861962,-5.95443652093343,-3.03117788366071));
#34072=CARTESIAN_POINT('Ctrl Pts',(84.0695983860438,-2.46216747788131,-6.92806001762949));
#34073=CARTESIAN_POINT('Ctrl Pts',(84.2681099904858,4.49416806949842,-5.81940218769057));
#34074=CARTESIAN_POINT('Ctrl Pts',(84.4335363275211,6.84159716243557,-0.465450279045067));
#34075=CARTESIAN_POINT('Ctrl Pts',(84.565877397149,5.4018620288319,3.56401832285386));
#34076=CARTESIAN_POINT('Ctrl Pts',(84.6651331993702,3.05045783488768,5.72873818258966));
#34077=CARTESIAN_POINT('Ctrl Pts',(84.7643890015912,-0.0581711681516334,
6.47139522045821));
#34078=CARTESIAN_POINT('Ctrl Pts',(84.8967300712192,-4.20511699218411,5.41674134303595));
#34079=CARTESIAN_POINT('Ctrl Pts',(85.000258876769,-6.16516640887946,2.32750288322991));
#34080=CARTESIAN_POINT('Ctrl Pts',(85.0707024149117,-6.22924600846334,0.137275087845278));
#34081=CARTESIAN_POINT('Ctrl Pts',(85.0749754182403,-6.22858364363872,0.00435858369765025));
#34082=CARTESIAN_POINT('Ctrl Pts',(84.0714645817596,-6.22691982511773,0.00134582525012326));
#34083=CARTESIAN_POINT('Ctrl Pts',(84.0989076020114,-6.22489235382799,-0.855356492542834));
#34084=CARTESIAN_POINT('Ctrl Pts',(84.1594358896702,-5.81262401081619,-2.74987092752364));
#34085=CARTESIAN_POINT('Ctrl Pts',(84.253049444736,-3.96930072085848,-5.13501567227216));
#34086=CARTESIAN_POINT('Ctrl Pts',(84.3523052469571,-1.02956513266701,-6.38923591846239));
#34087=CARTESIAN_POINT('Ctrl Pts',(84.4846463165852,3.23560668510475,-6.04606856350603));
#34088=CARTESIAN_POINT('Ctrl Pts',(84.6500726536202,7.15210351133029,-1.70599056920427));
#34089=CARTESIAN_POINT('Ctrl Pts',(84.8485842580625,5.30442784199376,5.09149580831549));
#34090=CARTESIAN_POINT('Ctrl Pts',(85.0470958625043,-1.39861029772509,7.21832207179135));
#34091=CARTESIAN_POINT('Ctrl Pts',(85.2047226370703,-5.7092439301469,3.65406932462159));
#34092=CARTESIAN_POINT('Ctrl Pts',(85.296178876822,-6.21531076597404,0.797672369212536));
#34093=CARTESIAN_POINT('Ctrl Pts',(85.3214645817596,-6.21024711481797,0.00611545682707264));
#34094=CARTESIAN_POINT('Origin',(28.1999754182402,0.,0.));
#34095=CARTESIAN_POINT('',(82.5749754182402,-6.21075901980729,0.000909742482199126));
#34096=CARTESIAN_POINT('',(82.8214645817596,-6.21810878279376,-0.00339757865050971));
#34097=CARTESIAN_POINT('',(28.1999754182402,-6.21925,5.68729293530136E-12));
#34098=CARTESIAN_POINT('Ctrl Pts',(82.5749754182403,-6.21075901980729,0.000909742482198966));
#34099=CARTESIAN_POINT('Ctrl Pts',(82.6099893304765,-6.20925005302336,-1.09762679373399));
#34100=CARTESIAN_POINT('Ctrl Pts',(82.7111737775268,-5.40608907411339,-4.27426631199952));
#34101=CARTESIAN_POINT('Ctrl Pts',(82.8785287593912,-0.323472535169768,
-7.34563502891261));
#34102=CARTESIAN_POINT('Ctrl Pts',(83.0439550964262,4.92520670119462,-4.77141851505581));
#34103=CARTESIAN_POINT('Ctrl Pts',(83.1762961660544,6.42635186854234,-0.7644224263167));
#34104=CARTESIAN_POINT('Ctrl Pts',(83.2755519682753,6.02756024934152,2.40670970572829));
#34105=CARTESIAN_POINT('Ctrl Pts',(83.3748077704965,4.13252826027979,4.98041666551734));
#34106=CARTESIAN_POINT('Ctrl Pts',(83.5071488401245,0.284353283747686,6.85151362148041));
#34107=CARTESIAN_POINT('Ctrl Pts',(83.6572047227057,-4.77560033766816,5.26519608353924));
#34108=CARTESIAN_POINT('Ctrl Pts',(83.7741753378801,-6.20321688953303,1.58340759986397));
#34109=CARTESIAN_POINT('Ctrl Pts',(83.8249754182403,-6.21863967025274,-0.00532692289228712));
#34110=CARTESIAN_POINT('Ctrl Pts',(82.8214645817596,-6.21810878279376,-0.00339757865050951));
#34111=CARTESIAN_POINT('Ctrl Pts',(82.8354657923868,-6.21944953262559,-0.4405939671335));
#34112=CARTESIAN_POINT('Ctrl Pts',(82.882552270421,-6.07008559218604,-1.90917328702513));
#34113=CARTESIAN_POINT('Ctrl Pts',(82.9627240158624,-4.91031465598665,-4.2155841781865));
#34114=CARTESIAN_POINT('Ctrl Pts',(83.0950650854904,-1.43106703177257,-6.70642548947526));
#34115=CARTESIAN_POINT('Ctrl Pts',(83.2604914225255,4.36166608043273,-5.91936292702175));
#34116=CARTESIAN_POINT('Ctrl Pts',(83.4590030269676,7.33784111646791,0.465158087628112));
#34117=CARTESIAN_POINT('Ctrl Pts',(83.6575146314097,3.59080068386597,6.41610744499814));
#34118=CARTESIAN_POINT('Ctrl Pts',(83.8560262358518,-3.45292231992367,6.49155727938758));
#34119=CARTESIAN_POINT('Ctrl Pts',(83.9940095526351,-6.13316871367438,2.4180846706705));
#34120=CARTESIAN_POINT('Ctrl Pts',(84.0658223346043,-6.22733667042163,0.177482641499614));
#34121=CARTESIAN_POINT('Ctrl Pts',(84.0714645817596,-6.22691982511773,0.00134582525012326));
#34122=CARTESIAN_POINT('Origin',(28.1999754182402,0.,0.));
#34123=CARTESIAN_POINT('',(81.3249754182402,-6.22245972074542,0.00511829929418269));
#34124=CARTESIAN_POINT('',(81.5714645817596,-6.21597937799738,0.00149266041878204));
#34125=CARTESIAN_POINT('',(28.1999754182402,-6.21925,5.68729293530136E-12));
#34126=CARTESIAN_POINT('Ctrl Pts',(81.3249754182402,-6.22245972074542,0.00511829929418263));
#34127=CARTESIAN_POINT('Ctrl Pts',(81.379632788259,-6.2062119306234,-1.7015911957153));
#34128=CARTESIAN_POINT('Ctrl Pts',(81.5004606930918,-4.59365834777172,-5.50076823327935));
#34129=CARTESIAN_POINT('Ctrl Pts',(81.6543738653314,0.682176659571807,-6.82339583348686));
#34130=CARTESIAN_POINT('Ctrl Pts',(81.7867149349596,4.41506970477836,-4.73175437719689));
#34131=CARTESIAN_POINT('Ctrl Pts',(81.8859707371805,6.1572775488005,-2.05223472198617));
#34132=CARTESIAN_POINT('Ctrl Pts',(81.9852265394016,6.37104488690502,1.13671765765088));
#34133=CARTESIAN_POINT('Ctrl Pts',(82.1175676090297,4.63949668876505,5.04966990705815));
#34134=CARTESIAN_POINT('Ctrl Pts',(82.2829939460648,-0.749954889722087,
7.3144074348083));
#34135=CARTESIAN_POINT('Ctrl Pts',(82.4464916382707,-5.53259199941689,4.03024244694824));
#34136=CARTESIAN_POINT('Ctrl Pts',(82.5438187956625,-6.21210175204047,0.978426565390665));
#34137=CARTESIAN_POINT('Ctrl Pts',(82.5749754182403,-6.21075901980729,0.000909742482198966));
#34138=CARTESIAN_POINT('Ctrl Pts',(81.5714645817596,-6.21597937799738,0.00149266041878201));
#34139=CARTESIAN_POINT('Ctrl Pts',(81.5720239827622,-6.216009963232,-0.0160310956563993));
#34140=CARTESIAN_POINT('Ctrl Pts',(81.6056686511719,-6.21346008847608,-1.07002792270585));
#34141=CARTESIAN_POINT('Ctrl Pts',(81.7054838543957,-5.42171283747731,-4.19870522938243));
#34142=CARTESIAN_POINT('Ctrl Pts',(81.8709101914306,-0.48919755281723,-7.33646196836831));
#34143=CARTESIAN_POINT('Ctrl Pts',(82.069421795873,5.90490006067872,-4.38091766304837));
#34144=CARTESIAN_POINT('Ctrl Pts',(82.2679334003147,6.88393788382687,2.58296022203711));
#34145=CARTESIAN_POINT('Ctrl Pts',(82.4664450047572,1.55262125162276,7.18695733311437));
#34146=CARTESIAN_POINT('Ctrl Pts',(82.6318713417919,-4.05385301920155,5.53085629844241));
#34147=CARTESIAN_POINT('Ctrl Pts',(82.7502112007931,-5.97891224336876,2.22413772225872));
#34148=CARTESIAN_POINT('Ctrl Pts',(82.8023805249798,-6.21628130182804,0.592513798148406));
#34149=CARTESIAN_POINT('Ctrl Pts',(82.8214645817596,-6.21810878279376,-0.00339757865050951));
#34150=CARTESIAN_POINT('Origin',(28.1999754182402,0.,0.));
#34151=CARTESIAN_POINT('',(80.0749754182403,-6.22591546342771,-0.00639606690001471));
#34152=CARTESIAN_POINT('',(80.3214645817596,-6.21925,3.12193847162856E-12));
#34153=CARTESIAN_POINT('',(28.1999754182402,-6.21925,5.68729293530136E-12));
#34154=CARTESIAN_POINT('Ctrl Pts',(80.0749754182403,-6.22591546342771,-0.00639606690001581));
#34155=CARTESIAN_POINT('Ctrl Pts',(80.0831057112274,-6.22789577682199,-0.259639247857812));
#34156=CARTESIAN_POINT('Ctrl Pts',(80.1574065390285,-6.09902881688988,-2.57131173126798));
#34157=CARTESIAN_POINT('Ctrl Pts',(80.2647926342366,-3.88310974879154,-5.65203984187573));
#34158=CARTESIAN_POINT('Ctrl Pts',(80.3971337038648,0.318133770830362,-6.46383252320411));
#34159=CARTESIAN_POINT('Ctrl Pts',(80.4963895060858,3.37833202016725,-5.5417151612656));
#34160=CARTESIAN_POINT('Ctrl Pts',(80.5956453083068,5.59991621302585,-3.24396029434143));
#34161=CARTESIAN_POINT('Ctrl Pts',(80.7279863779349,6.80296829521341,0.862390903031537));
#34162=CARTESIAN_POINT('Ctrl Pts',(80.89341271497,4.14826379333761,6.07082333459648));
#34163=CARTESIAN_POINT('Ctrl Pts',(81.0919243194122,-2.86075767029707,6.77320823899939));
#34164=CARTESIAN_POINT('Ctrl Pts',(81.2357785538355,-6.035454250839,2.78678910832403));
#34165=CARTESIAN_POINT('Ctrl Pts',(81.3134622534449,-6.22588219579629,0.364623845702632));
#34166=CARTESIAN_POINT('Ctrl Pts',(81.3249754182402,-6.22245972074542,0.00511829929418263));
#34167=CARTESIAN_POINT('Ctrl Pts',(80.3214645817596,-6.21763963428012,0.00313466642206932));
#34168=CARTESIAN_POINT('Ctrl Pts',(80.3747527079517,-6.20169098464531,-1.66223637650542));
#34169=CARTESIAN_POINT('Ctrl Pts',(80.4942113689577,-4.66823370288436,-5.40918680826147));
#34170=CARTESIAN_POINT('Ctrl Pts',(80.6798405647781,1.68251786406567,-7.15747287344582));
#34171=CARTESIAN_POINT('Ctrl Pts',(80.8783521692202,6.92514205415142,-2.4703626913545));
#34172=CARTESIAN_POINT('Ctrl Pts',(81.0768637736622,5.82471539119074,4.48727969605447));
#34173=CARTESIAN_POINT('Ctrl Pts',(81.2422901106974,0.473544591506288,6.84104167617517));
#34174=CARTESIAN_POINT('Ctrl Pts',(81.3746311803253,-3.55762461323784,5.40607501755736));
#34175=CARTESIAN_POINT('Ctrl Pts',(81.473327581544,-5.71290909288839,3.07047161723339));
#34176=CARTESIAN_POINT('Ctrl Pts',(81.5389387153552,-6.21420102713517,1.0203956411079));
#34177=CARTESIAN_POINT('Ctrl Pts',(81.5714645817596,-6.21597937799738,0.00149266041878201));
#34178=CARTESIAN_POINT('Origin',(28.1999754182402,0.,0.));
#34179=CARTESIAN_POINT('',(78.8249754182403,-6.21868393922028,3.57448842112454E-5));
#34180=CARTESIAN_POINT('',(79.0714645817596,-6.21925,2.63432203795717E-12));
#34181=CARTESIAN_POINT('',(28.1999754182402,-6.21925,5.68729293530136E-12));
#34182=CARTESIAN_POINT('Ctrl Pts',(78.8249754182403,-6.20725553121229,0.000757411355485488));
#34183=CARTESIAN_POINT('Ctrl Pts',(78.8527491690098,-6.20985090167876,-0.869958336885441));
#34184=CARTESIAN_POINT('Ctrl Pts',(78.9136081871864,-5.83503896856034,-2.77734718629318));
#34185=CARTESIAN_POINT('Ctrl Pts',(79.0075524727701,-3.92908674363906,-5.14243301805027));
#34186=CARTESIAN_POINT('Ctrl Pts',(79.106808274991,-0.996518304073061,-6.41332093667049));
#34187=CARTESIAN_POINT('Ctrl Pts',(79.2060640772121,2.18341903006714,-6.09220988831756));
#34188=CARTESIAN_POINT('Ctrl Pts',(79.33840514684,5.75275644429788,-3.73227664943248));
#34189=CARTESIAN_POINT('Ctrl Pts',(79.5038314838753,7.08686629844,1.95941688444093));
#34190=CARTESIAN_POINT('Ctrl Pts',(79.7023430883174,2.18670980208234,7.01987069243372));
#34191=CARTESIAN_POINT('Ctrl Pts',(79.8927243997723,-4.42763839203692,5.7020875320387));
#34192=CARTESIAN_POINT('Ctrl Pts',(80.0169351764133,-6.21177847371782,1.80144720358636));
#34193=CARTESIAN_POINT('Ctrl Pts',(80.0749754182403,-6.22591546342771,-0.00639606690001581));
#34194=CARTESIAN_POINT('Ctrl Pts',(79.0714645817596,-6.21925,2.98784547070725E-12));
#34195=CARTESIAN_POINT('Ctrl Pts',(79.1302643332333,-6.21925000000088,-1.83816020915454));
#34196=CARTESIAN_POINT('Ctrl Pts',(79.189064084707,-5.35502977485182,-3.65808141345713));
#34197=CARTESIAN_POINT('Ctrl Pts',(79.2478638361807,-3.93049712176041,-4.81977830800682));
#34198=CARTESIAN_POINT('Ctrl Pts',(79.3066635876544,-2.505964468669,-5.98147520255652));
#34199=CARTESIAN_POINT('Ctrl Pts',(79.3654633391281,-0.549389021421145,
-6.46189408921037));
#34200=CARTESIAN_POINT('Ctrl Pts',(79.4242630906018,1.25118869866695,-6.09209302315946));
#34201=CARTESIAN_POINT('Ctrl Pts',(79.4830628420755,3.05176641875505,-5.72229195710854));
#34202=CARTESIAN_POINT('Ctrl Pts',(79.5418625935492,4.66061422075082,-4.50960958425064));
#34203=CARTESIAN_POINT('Ctrl Pts',(79.6006623450229,5.51197192302639,-2.88049233331193));
#34204=CARTESIAN_POINT('Ctrl Pts',(79.6594620964966,6.36332962530195,-1.25137508237321));
#34205=CARTESIAN_POINT('Ctrl Pts',(79.7182618479703,6.44030216377303,0.761847462639688));
#34206=CARTESIAN_POINT('Ctrl Pts',(79.777061599444,5.71582172177495,2.45121451680297));
#34207=CARTESIAN_POINT('Ctrl Pts',(79.8358613509177,4.99134127977688,4.14058157096625));
#34208=CARTESIAN_POINT('Ctrl Pts',(79.8946611023914,3.47978506146562,5.47256790209411));
#34209=CARTESIAN_POINT('Ctrl Pts',(79.9534608538651,1.7127001277575,5.97877318811137));
#34210=CARTESIAN_POINT('Ctrl Pts',(80.0122606053388,-0.0543848059506163,
6.48497847412863));
#34211=CARTESIAN_POINT('Ctrl Pts',(80.0710603568125,-2.04193092337348,6.15535714814349));
#34212=CARTESIAN_POINT('Ctrl Pts',(80.1298601082862,-3.55100669662382,5.10582236305111));
#34213=CARTESIAN_POINT('Ctrl Pts',(80.1886598597599,-5.06008246987417,4.05628757795872));
#34214=CARTESIAN_POINT('Ctrl Pts',(80.2474596112336,-6.06074051980812,2.30766719190311));
#34215=CARTESIAN_POINT('Ctrl Pts',(80.3062593627073,-6.20109393743669,0.474873184740817));
#34216=CARTESIAN_POINT('Ctrl Pts',(80.3113277690581,-6.21319208641573,0.316890462829387));
#34217=CARTESIAN_POINT('Ctrl Pts',(80.3163961754088,-6.21924999999992,0.158445276459264));
#34218=CARTESIAN_POINT('Ctrl Pts',(80.3214645817596,-6.21925,3.12194003490965E-12));
#34219=CARTESIAN_POINT('Origin',(28.1999754182402,0.,0.));
#34220=CARTESIAN_POINT('',(77.5749754182403,-6.21925,2.62169104890118E-12));
#34221=CARTESIAN_POINT('',(77.8214645817596,-6.20978691806976,-0.00197117650404144));
#34222=CARTESIAN_POINT('',(28.1999754182402,-6.21925,5.68729293530136E-12));
#34223=CARTESIAN_POINT('Ctrl Pts',(77.5749754182403,-6.21925,2.97521448165126E-12));
#34224=CARTESIAN_POINT('Ctrl Pts',(77.633775169714,-6.21925000000088,-1.83816020915432));
#34225=CARTESIAN_POINT('Ctrl Pts',(77.6925749211877,-5.35502977485205,-3.65808141345668));
#34226=CARTESIAN_POINT('Ctrl Pts',(77.7513746726614,-3.93049712176095,-4.81977830800639));
#34227=CARTESIAN_POINT('Ctrl Pts',(77.8101744241351,-2.50596446866985,-5.98147520255609));
#34228=CARTESIAN_POINT('Ctrl Pts',(77.8689741756087,-0.549389021422371,
-6.4618940892102));
#34229=CARTESIAN_POINT('Ctrl Pts',(77.9277739270824,1.25118869866558,-6.09209302315974));
#34230=CARTESIAN_POINT('Ctrl Pts',(77.9865736785561,3.05176641875353,-5.72229195710927));
#34231=CARTESIAN_POINT('Ctrl Pts',(78.0453734300298,4.6606142207494,-4.50960958425201));
#34232=CARTESIAN_POINT('Ctrl Pts',(78.1041731815035,5.51197192302541,-2.88049233331379));
#34233=CARTESIAN_POINT('Ctrl Pts',(78.1629729329772,6.36332962530142,-1.25137508237558));
#34234=CARTESIAN_POINT('Ctrl Pts',(78.2217726844509,6.44030216377328,0.76184746263699));
#34235=CARTESIAN_POINT('Ctrl Pts',(78.2805724359246,5.71582172177606,2.45121451680038));
#34236=CARTESIAN_POINT('Ctrl Pts',(78.3393721873983,4.99134127977885,4.14058157096377));
#34237=CARTESIAN_POINT('Ctrl Pts',(78.398171938872,3.4797850614685,5.47256790209221));
#34238=CARTESIAN_POINT('Ctrl Pts',(78.4569716903457,1.71270012776089,5.9787731881104));
#34239=CARTESIAN_POINT('Ctrl Pts',(78.5157714418194,-0.0543848059467164,
6.4849784741286));
#34240=CARTESIAN_POINT('Ctrl Pts',(78.5745711932931,-2.04193092336948,6.15535714814475));
#34241=CARTESIAN_POINT('Ctrl Pts',(78.6333709447668,-3.55100669662035,5.10582236305352));
#34242=CARTESIAN_POINT('Ctrl Pts',(78.6921706962405,-5.06008246987121,4.0562875779623));
#34243=CARTESIAN_POINT('Ctrl Pts',(78.7509704477142,-6.06074051980631,2.30766719190769));
#34244=CARTESIAN_POINT('Ctrl Pts',(78.8097701991879,-6.20109393743632,0.47487318474574));
#34245=CARTESIAN_POINT('Ctrl Pts',(78.8148386055387,-6.2131920864156,0.316890462832674));
#34246=CARTESIAN_POINT('Ctrl Pts',(78.8199070118895,-6.21924999999992,0.158445276460901));
#34247=CARTESIAN_POINT('Ctrl Pts',(78.8249754182403,-6.21925,3.10930904585366E-12));
#34248=CARTESIAN_POINT('Ctrl Pts',(77.8214645817596,-6.20978691806976,-0.00197117650404123));
#34249=CARTESIAN_POINT('Ctrl Pts',(77.8478690887026,-6.21394152490341,-0.830640096174487));
#34250=CARTESIAN_POINT('Ctrl Pts',(77.9404441304595,-5.67565032115918,-3.73163537846471));
#34251=CARTESIAN_POINT('Ctrl Pts',(78.0991897070306,-1.28071754910471,-7.24016897982555));
#34252=CARTESIAN_POINT('Ctrl Pts',(78.2977013114727,5.39592604241165,-4.99469424527876));
#34253=CARTESIAN_POINT('Ctrl Pts',(78.4631276485078,6.82419817520737,0.674103078769445));
#34254=CARTESIAN_POINT('Ctrl Pts',(78.5954687181358,4.73697475670672,4.40946823761063));
#34255=CARTESIAN_POINT('Ctrl Pts',(78.6947245203569,2.0595182708145,6.1548451369039));
#34256=CARTESIAN_POINT('Ctrl Pts',(78.793980322578,-1.12917895789654,6.37238533558803));
#34257=CARTESIAN_POINT('Ctrl Pts',(78.9195603430456,-4.8441674685037,4.73369282734356));
#34258=CARTESIAN_POINT('Ctrl Pts',(79.012055096106,-6.21390045877809,1.84473924277232));
#34259=CARTESIAN_POINT('Ctrl Pts',(79.0714645817595,-6.22720257754346,-0.00302929506990259));
#34260=CARTESIAN_POINT('Origin',(28.1999754182402,0.,0.));
#34261=CARTESIAN_POINT('',(76.3249754182403,-6.22173704813553,-0.000300768587064016));
#34262=CARTESIAN_POINT('',(76.5714645817596,-6.21633441253698,0.00478628877724901));
#34263=CARTESIAN_POINT('',(28.1999754182402,-6.21925,5.68729293530136E-12));
#34264=CARTESIAN_POINT('Ctrl Pts',(76.3249754182403,-6.22173704813553,-0.000300768587063625));
#34265=CARTESIAN_POINT('Ctrl Pts',(76.3258655497607,-6.22175262900424,-0.0280386865486988));
#34266=CARTESIAN_POINT('Ctrl Pts',(76.3598409486881,-6.2149600094303,-1.08675627772139));
#34267=CARTESIAN_POINT('Ctrl Pts',(76.4269016150225,-5.64270178030442,-3.1689519723282));
#34268=CARTESIAN_POINT('Ctrl Pts',(76.5592426846506,-2.72049697200563,-6.29467965193754));
#34269=CARTESIAN_POINT('Ctrl Pts',(76.7246690216857,3.1139858635671,-6.66078677788813));
#34270=CARTESIAN_POINT('Ctrl Pts',(76.9231806261278,7.28626036027289,-0.985238173931595));
#34271=CARTESIAN_POINT('Ctrl Pts',(77.1216922305699,4.78113090820971,5.58579193450243));
#34272=CARTESIAN_POINT('Ctrl Pts',(77.3202038350121,-2.11055225112471,7.0433342710871));
#34273=CARTESIAN_POINT('Ctrl Pts',(77.4712982309021,-5.86445747246485,3.2461908392673));
#34274=CARTESIAN_POINT('Ctrl Pts',(77.5562220919782,-6.22385504227548,0.589316613379467));
#34275=CARTESIAN_POINT('Ctrl Pts',(77.5749754182403,-6.22088517383465,0.00203704096300435));
#34276=CARTESIAN_POINT('Ctrl Pts',(76.5714645817596,-6.21633441253698,0.00478628877724929));
#34277=CARTESIAN_POINT('Ctrl Pts',(76.6175125464849,-6.20517767444331,-1.43667693955316));
#34278=CARTESIAN_POINT('Ctrl Pts',(76.7297310460244,-4.98752806823633,-4.96640378610114));
#34279=CARTESIAN_POINT('Ctrl Pts',(76.9081200803781,0.897600199059924,-7.29776009071585));
#34280=CARTESIAN_POINT('Ctrl Pts',(77.0735464174129,5.64744158313445,-3.88979424396703));
#34281=CARTESIAN_POINT('Ctrl Pts',(77.2058874870412,6.46420439911098,0.31048586229469));
#34282=CARTESIAN_POINT('Ctrl Pts',(77.3051432892621,5.54570835728657,3.37177297323113));
#34283=CARTESIAN_POINT('Ctrl Pts',(77.4043990914832,3.2505835667813,5.59607420068252));
#34284=CARTESIAN_POINT('Ctrl Pts',(77.5367401611112,-0.854341364942577,
6.80398387178119));
#34285=CARTESIAN_POINT('Ctrl Pts',(77.6757619912035,-5.23406692997655,4.57819005869191));
#34286=CARTESIAN_POINT('Ctrl Pts',(77.7816985538885,-6.20352994794352,1.24603059178104));
#34287=CARTESIAN_POINT('Ctrl Pts',(77.8214645817596,-6.20978691806976,-0.00197117650404123));
#34288=CARTESIAN_POINT('Origin',(28.1999754182402,0.,0.));
#34289=CARTESIAN_POINT('',(75.0749754182403,-6.21925,2.53026332525108E-12));
#34290=CARTESIAN_POINT('',(75.3214645817596,-6.22966011066701,0.000792207867037114));
#34291=CARTESIAN_POINT('',(28.1999754182402,-6.21925,5.68729293530136E-12));
#34292=CARTESIAN_POINT('Ctrl Pts',(75.0749754182403,-6.22001023982655,-0.00175185933932603));
#34293=CARTESIAN_POINT('Ctrl Pts',(75.0955090075431,-6.22308363120507,-0.644970145081011));
#34294=CARTESIAN_POINT('Ctrl Pts',(75.18221313166,-5.82062366491697,-3.35890160914945));
#34295=CARTESIAN_POINT('Ctrl Pts',(75.3350877905908,-1.92073099598895,-7.09744889988669));
#34296=CARTESIAN_POINT('Ctrl Pts',(75.533599395033,4.92934482030065,-5.45544168096722));
#34297=CARTESIAN_POINT('Ctrl Pts',(75.7321109994751,7.25718867309859,1.18046468258034));
#34298=CARTESIAN_POINT('Ctrl Pts',(75.9306226039172,2.93407158228261,6.74197392506965));
#34299=CARTESIAN_POINT('Ctrl Pts',(76.0960489409524,-2.88848170832391,6.21938655461771));
#34300=CARTESIAN_POINT('Ctrl Pts',(76.22749987906,-5.70664773980729,3.03788962666509));
#34301=CARTESIAN_POINT('Ctrl Pts',(76.2927802823537,-6.22117350423921,1.00295101784076));
#34302=CARTESIAN_POINT('Ctrl Pts',(76.3249754182403,-6.22173704813553,-0.000300768587063625));
#34303=CARTESIAN_POINT('Ctrl Pts',(75.3214645817596,-6.22966011066701,0.000792207867037168));
#34304=CARTESIAN_POINT('Ctrl Pts',(75.3871560042675,-6.22706287267145,-2.04425958841946));
#34305=CARTESIAN_POINT('Ctrl Pts',(75.5190179615893,-4.00786877131307,-6.15474593912649));
#34306=CARTESIAN_POINT('Ctrl Pts',(75.6839651863182,1.80286576781962,-6.61617493105383));
#34307=CARTESIAN_POINT('Ctrl Pts',(75.8163062559463,5.13778071835795,-3.93516826512113));
#34308=CARTESIAN_POINT('Ctrl Pts',(75.9155620581673,6.41213741680385,-1.0041055296563));
#34309=CARTESIAN_POINT('Ctrl Pts',(76.0148178603885,6.09478893729921,2.1762095014379));
#34310=CARTESIAN_POINT('Ctrl Pts',(76.1471589300164,3.73908041305424,5.74833657329857));
#34311=CARTESIAN_POINT('Ctrl Pts',(76.3125852670516,-1.95103068448381,7.08917962300208));
#34312=CARTESIAN_POINT('Ctrl Pts',(76.4650489067683,-5.84208075630458,3.330294435224));
#34313=CARTESIAN_POINT('Ctrl Pts',(76.5513420116709,-6.22120981247244,0.634693495648045));
#34314=CARTESIAN_POINT('Ctrl Pts',(76.5714645817596,-6.21633441253698,0.00478628877724929));
#34315=CARTESIAN_POINT('Origin',(28.1999754182402,0.,0.));
#34316=CARTESIAN_POINT('',(73.8249754182403,-6.21908946014578,2.83535676061311E-7));
#34317=CARTESIAN_POINT('',(74.0714645817596,-6.21923049956772,-3.95732063914942E-5));
#34318=CARTESIAN_POINT('',(28.1999754182402,-6.21925,5.68729293530136E-12));
#34319=CARTESIAN_POINT('Ctrl Pts',(73.8249754182403,-6.21925,2.57293078904406E-12));
#34320=CARTESIAN_POINT('Ctrl Pts',(73.883775169714,-6.21925000000076,-1.83816020915484));
#34321=CARTESIAN_POINT('Ctrl Pts',(73.9425749211877,-5.35502977485169,-3.65808141345726));
#34322=CARTESIAN_POINT('Ctrl Pts',(74.0013746726614,-3.93049712176036,-4.81977830800686));
#34323=CARTESIAN_POINT('Ctrl Pts',(74.0601744241351,-2.50596446866904,-5.98147520255647));
#34324=CARTESIAN_POINT('Ctrl Pts',(74.1189741756088,-0.549389021421334,
-6.46189408921033));
#34325=CARTESIAN_POINT('Ctrl Pts',(74.1777739270825,1.25118869866667,-6.09209302315951));
#34326=CARTESIAN_POINT('Ctrl Pts',(74.2365736785562,3.05176641875466,-5.7222919571087));
#34327=CARTESIAN_POINT('Ctrl Pts',(74.2953734300299,4.66061422075041,-4.50960958425102));
#34328=CARTESIAN_POINT('Ctrl Pts',(74.3541731815036,5.51197192302609,-2.8804923333125));
#34329=CARTESIAN_POINT('Ctrl Pts',(74.4129729329773,6.36332962530177,-1.25137508237398));
#34330=CARTESIAN_POINT('Ctrl Pts',(74.471772684451,6.4403021637731,0.761847462638762));
#34331=CARTESIAN_POINT('Ctrl Pts',(74.5305724359247,5.71582172177535,2.45121451680205));
#34332=CARTESIAN_POINT('Ctrl Pts',(74.5893721873984,4.99134127977759,4.14058157096534));
#34333=CARTESIAN_POINT('Ctrl Pts',(74.648171938872,3.4797850614667,5.47256790209339));
#34334=CARTESIAN_POINT('Ctrl Pts',(74.7069716903457,1.7127001277588,5.978773188111));
#34335=CARTESIAN_POINT('Ctrl Pts',(74.7657714418194,-0.0543848059490926,
6.48497847412861));
#34336=CARTESIAN_POINT('Ctrl Pts',(74.8245711932931,-2.04193092337188,6.15535714814398));
#34337=CARTESIAN_POINT('Ctrl Pts',(74.8833709447668,-3.55100669662242,5.10582236305208));
#34338=CARTESIAN_POINT('Ctrl Pts',(74.9421706962405,-5.06008246987296,4.05628757796018));
#34339=CARTESIAN_POINT('Ctrl Pts',(75.0009704477142,-6.06074051980737,2.307667191905));
#34340=CARTESIAN_POINT('Ctrl Pts',(75.0597701991879,-6.20109393743654,0.474873184742871));
#34341=CARTESIAN_POINT('Ctrl Pts',(75.0648386055387,-6.21319208641569,0.316890462830563));
#34342=CARTESIAN_POINT('Ctrl Pts',(75.0699070118895,-6.21924999999994,0.158445276459556));
#34343=CARTESIAN_POINT('Ctrl Pts',(75.0749754182403,-6.21925,2.53026363687142E-12));
#34344=CARTESIAN_POINT('Ctrl Pts',(74.0714645817596,-6.21535782541014,-0.00789858458239298));
#34345=CARTESIAN_POINT('Ctrl Pts',(74.0906289272359,-6.22045708227677,-0.607720104182565));
#34346=CARTESIAN_POINT('Ctrl Pts',(74.1759638075261,-5.86589957661036,-3.27147217734002));
#34347=CARTESIAN_POINT('Ctrl Pts',(74.2943839552234,-2.89337352700839,-6.21711227638719));
#34348=CARTESIAN_POINT('Ctrl Pts',(74.4267250248515,1.38429868618496,-6.32187133024273));
#34349=CARTESIAN_POINT('Ctrl Pts',(74.5259808270725,4.24950930786462,-4.9056503007122));
#34350=CARTESIAN_POINT('Ctrl Pts',(74.6252366292937,6.05985073959253,-2.27168416620927));
#34351=CARTESIAN_POINT('Ctrl Pts',(74.7575776989216,6.5661819132465,1.9772078337143));
#34352=CARTESIAN_POINT('Ctrl Pts',(74.9230040359569,3.08550547279318,6.67402760129288));
#34353=CARTESIAN_POINT('Ctrl Pts',(75.1215156403989,-3.94304652828918,6.20585758518567));
#34354=CARTESIAN_POINT('Ctrl Pts',(75.2543358223332,-6.22415247288678,2.09056984967631));
#34355=CARTESIAN_POINT('Ctrl Pts',(75.3209854694534,-6.22967905330272,0.0157075414827555));
#34356=CARTESIAN_POINT('Ctrl Pts',(75.3214645817596,-6.22966011066701,0.000792207867037168));
#34357=CARTESIAN_POINT('Origin',(28.1999754182402,0.,0.));
#34358=CARTESIAN_POINT('',(72.5749754182403,-6.22725864519176,0.00554552405307109));
#34359=CARTESIAN_POINT('',(72.8214645817596,-6.217957588601,0.000688194671020262));
#34360=CARTESIAN_POINT('',(28.1999754182402,-6.21925,5.68729293530136E-12));
#34361=CARTESIAN_POINT('Ctrl Pts',(72.5749754182403,-6.22725864519176,0.00554552405307093));
#34362=CARTESIAN_POINT('Ctrl Pts',(72.634795923108,-6.21476230695049,-1.85648529413867));
#34363=CARTESIAN_POINT('Ctrl Pts',(72.7607869627898,-4.33519792882598,-5.80824127579764));
#34364=CARTESIAN_POINT('Ctrl Pts',(72.9529485372856,2.37438354046372,-6.95863454231163));
#34365=CARTESIAN_POINT('Ctrl Pts',(73.1514601417277,7.13688992541174,-1.76848755210188));
#34366=CARTESIAN_POINT('Ctrl Pts',(73.3168864787627,5.65050896588544,3.88535316654217));
#34367=CARTESIAN_POINT('Ctrl Pts',(73.4492275483909,2.01909789486699,6.14862180311659));
#34368=CARTESIAN_POINT('Ctrl Pts',(73.5484833506118,-1.16830659219089,6.38426173854624));
#34369=CARTESIAN_POINT('Ctrl Pts',(73.647739152833,-4.06570784309721,5.0351131850683));
#34370=CARTESIAN_POINT('Ctrl Pts',(73.7399031753757,-5.87258511218837,2.66549161737149));
#34371=CARTESIAN_POINT('Ctrl Pts',(73.7989819305115,-6.2112958543,0.814794971644609));
#34372=CARTESIAN_POINT('Ctrl Pts',(73.8249754182403,-6.2078499707538,2.01338545920832E-5));
#34373=CARTESIAN_POINT('Ctrl Pts',(72.8214645817596,-6.21925,1.96384921694517E-12));
#34374=CARTESIAN_POINT('Ctrl Pts',(72.8802643332333,-6.21925000000058,-1.83816020915533));
#34375=CARTESIAN_POINT('Ctrl Pts',(72.939064084707,-5.35502977485145,-3.65808141345755));
#34376=CARTESIAN_POINT('Ctrl Pts',(72.9978638361807,-3.93049712176017,-4.81977830800702));
#34377=CARTESIAN_POINT('Ctrl Pts',(73.0566635876544,-2.50596446866888,-5.9814752025565));
#34378=CARTESIAN_POINT('Ctrl Pts',(73.1154633391281,-0.54938902142132,-6.46189408921029));
#34379=CARTESIAN_POINT('Ctrl Pts',(73.1742630906018,1.25118869866657,-6.09209302315953));
#34380=CARTESIAN_POINT('Ctrl Pts',(73.2330628420755,3.05176641875446,-5.72229195710877));
#34381=CARTESIAN_POINT('Ctrl Pts',(73.2918625935492,4.66061422075014,-4.50960958425125));
#34382=CARTESIAN_POINT('Ctrl Pts',(73.3506623450229,5.51197192302588,-2.8804923333129));
#34383=CARTESIAN_POINT('Ctrl Pts',(73.4094620964966,6.36332962530162,-1.25137508237454));
#34384=CARTESIAN_POINT('Ctrl Pts',(73.4682618479702,6.44030216377315,0.761847462638037));
#34385=CARTESIAN_POINT('Ctrl Pts',(73.5270615994439,5.71582172177566,2.45121451680131));
#34386=CARTESIAN_POINT('Ctrl Pts',(73.5858613509176,4.99134127977817,4.14058157096459));
#34387=CARTESIAN_POINT('Ctrl Pts',(73.6446611023913,3.4797850614676,5.47256790209277));
#34388=CARTESIAN_POINT('Ctrl Pts',(73.703460853865,1.71270012775992,5.97877318811068));
#34389=CARTESIAN_POINT('Ctrl Pts',(73.7622606053387,-0.0543848059477714,
6.48497847412859));
#34390=CARTESIAN_POINT('Ctrl Pts',(73.8210603568124,-2.04193092337049,6.15535714814441));
#34391=CARTESIAN_POINT('Ctrl Pts',(73.8798601082861,-3.55100669662118,5.10582236305294));
#34392=CARTESIAN_POINT('Ctrl Pts',(73.9386598597598,-5.06008246987187,4.05628757796147));
#34393=CARTESIAN_POINT('Ctrl Pts',(73.9974596112335,-6.06074051980669,2.3076671919067));
#34394=CARTESIAN_POINT('Ctrl Pts',(74.0562593627072,-6.20109393743639,0.474873184744731));
#34395=CARTESIAN_POINT('Ctrl Pts',(74.061327769058,-6.21319208641565,0.316890462831781));
#34396=CARTESIAN_POINT('Ctrl Pts',(74.0663961754088,-6.21924999999994,0.158445276460126));
#34397=CARTESIAN_POINT('Ctrl Pts',(74.0714645817596,-6.21925,2.45146721389765E-12));
#34398=CARTESIAN_POINT('Origin',(28.1999754182402,0.,0.));
#34399=CARTESIAN_POINT('',(71.3249754182403,-6.22194821980233,-0.00360940077133112));
#34400=CARTESIAN_POINT('',(71.5714645817596,-6.22570420439633,0.00188724029056356));
#34401=CARTESIAN_POINT('',(28.1999754182402,-6.21925,5.68729293530136E-12));
#34402=CARTESIAN_POINT('Ctrl Pts',(71.3249754182403,-6.22194821980233,-0.00360940077133092));
#34403=CARTESIAN_POINT('Ctrl Pts',(71.3382688460764,-6.22445124236017,-0.418740319735753));
#34404=CARTESIAN_POINT('Ctrl Pts',(71.4177328087265,-5.98942607440445,-2.89665130682511));
#34405=CARTESIAN_POINT('Ctrl Pts',(71.563367306191,-2.68617674612466,-6.85019204663737));
#34406=CARTESIAN_POINT('Ctrl Pts',(71.7618789106327,4.31461801077602,-5.95570943739811));
#34407=CARTESIAN_POINT('Ctrl Pts',(71.9273052476681,6.82127674849029,-0.680243620698351));
#34408=CARTESIAN_POINT('Ctrl Pts',(72.059646317296,5.51192719551105,3.39346452184477));
#34409=CARTESIAN_POINT('Ctrl Pts',(72.1589021195172,3.22776268544752,5.63020767552143));
#34410=CARTESIAN_POINT('Ctrl Pts',(72.2581579217381,0.144787652460555,6.47013157578351));
#34411=CARTESIAN_POINT('Ctrl Pts',(72.3904989913663,-4.03362152721484,5.54570745472594));
#34412=CARTESIAN_POINT('Ctrl Pts',(72.4961048235336,-6.13049964680174,2.45871254298357));
#34413=CARTESIAN_POINT('Ctrl Pts',(72.568625388294,-6.22858514890861,0.20320268998025));
#34414=CARTESIAN_POINT('Ctrl Pts',(72.5749754182403,-6.22725864519176,0.00554552405307093));
#34415=CARTESIAN_POINT('Ctrl Pts',(71.5714645817596,-6.22570420439633,0.00188724029056342));
#34416=CARTESIAN_POINT('Ctrl Pts',(71.5968305753937,-6.22320179469496,-0.79041573268228));
#34417=CARTESIAN_POINT('Ctrl Pts',(71.6552818364349,-5.85767767178159,-2.62081709736886));
#34418=CARTESIAN_POINT('Ctrl Pts',(71.7468183648829,-4.12753807040063,-5.00810542026236));
#34419=CARTESIAN_POINT('Ctrl Pts',(71.8460741671042,-1.22942858196295,-6.35390206362266));
#34420=CARTESIAN_POINT('Ctrl Pts',(71.978415236732,3.04488676341186,-6.14439894507291));
#34421=CARTESIAN_POINT('Ctrl Pts',(72.1438415737674,7.09505541724423,-1.92914383180871));
#34422=CARTESIAN_POINT('Ctrl Pts',(72.3423531782092,5.46132883333844,4.92289529580099));
#34423=CARTESIAN_POINT('Ctrl Pts',(72.5408647826516,-1.17190946057312,7.25857562521031));
#34424=CARTESIAN_POINT('Ctrl Pts',(72.7005685838348,-5.65024837779282,3.78590359445975));
#34425=CARTESIAN_POINT('Ctrl Pts',(72.7941018502042,-6.21330002205454,0.862522468085002));
#34426=CARTESIAN_POINT('Ctrl Pts',(72.8214645817596,-6.20893906029042,0.0054904605059336));
#34427=CARTESIAN_POINT('Origin',(28.1999754182402,0.,0.));
#34428=CARTESIAN_POINT('',(70.0749754182403,-6.21806317550423,-0.000299885513699476));
#34429=CARTESIAN_POINT('',(70.3214645817596,-6.22327189076832,-0.00449888440332335));
#34430=CARTESIAN_POINT('',(28.1999754182402,-6.21925,5.68729293530136E-12));
#34431=CARTESIAN_POINT('Ctrl Pts',(70.0749754182403,-6.20699959075668,-0.00309542000869176));
#34432=CARTESIAN_POINT('Ctrl Pts',(70.1079123038589,-6.20822260668311,-1.03541925636434));
#34433=CARTESIAN_POINT('Ctrl Pts',(70.2070197242914,-5.47881021611929,-4.13832027487605));
#34434=CARTESIAN_POINT('Ctrl Pts',(70.3722976795382,-0.557063823628739,
-7.3341557210225));
#34435=CARTESIAN_POINT('Ctrl Pts',(70.5708092839802,5.85298547448848,-4.44184497426088));
#34436=CARTESIAN_POINT('Ctrl Pts',(70.7693208884224,6.91261030511504,2.50813707913662));
#34437=CARTESIAN_POINT('Ctrl Pts',(70.9678324928645,1.6305555301296,7.17107975691506));
#34438=CARTESIAN_POINT('Ctrl Pts',(71.1332588298994,-3.99925385407112,5.57258592607248));
#34439=CARTESIAN_POINT('Ctrl Pts',(71.2523064716916,-5.96060023780131,2.26929551249555));
#34440=CARTESIAN_POINT('Ctrl Pts',(71.3051835786694,-6.21822160981746,0.614455755210577));
#34441=CARTESIAN_POINT('Ctrl Pts',(71.3249754182403,-6.22194821980233,-0.00360940077133092));
#34442=CARTESIAN_POINT('Ctrl Pts',(70.3214645817596,-6.22327189076832,-0.00449888440332329));
#34443=CARTESIAN_POINT('Ctrl Pts',(70.3333887657692,-6.22667288846678,-0.376563255007046));
#34444=CARTESIAN_POINT('Ctrl Pts',(70.4114834845927,-6.02678452208852,-2.81004110988959));
#34445=CARTESIAN_POINT('Ctrl Pts',(70.5557487382304,-2.81181884640884,-6.79534921779986));
#34446=CARTESIAN_POINT('Ctrl Pts',(70.7211750752654,3.00649289900833,-6.16512333542295));
#34447=CARTESIAN_POINT('Ctrl Pts',(70.8535161448936,5.77263950695759,-2.91134114312552));
#34448=CARTESIAN_POINT('Ctrl Pts',(70.9858572145215,6.74314937401964,1.2444879873417));
#34449=CARTESIAN_POINT('Ctrl Pts',(71.1512835515567,3.79854938863639,6.30172191780343));
#34450=CARTESIAN_POINT('Ctrl Pts',(71.3497951559988,-3.25302923561936,6.59577169661227));
#34451=CARTESIAN_POINT('Ctrl Pts',(71.4898554993997,-6.09535851688912,2.54913226163309));
#34452=CARTESIAN_POINT('Ctrl Pts',(71.5637453079867,-6.22646572731775,0.242997588565489));
#34453=CARTESIAN_POINT('Ctrl Pts',(71.5714645817596,-6.22570420439633,0.00188724029056342));
#34454=CARTESIAN_POINT('Origin',(28.1999754182402,0.,0.));
#34455=CARTESIAN_POINT('',(68.8249754182403,-6.21925,1.68302909948438E-12));
#34456=CARTESIAN_POINT('',(69.0714645817596,-6.21743748979354,0.000366195279979008));
#34457=CARTESIAN_POINT('',(28.1999754182402,-6.21925,5.68729293530136E-12));
#34458=CARTESIAN_POINT('Ctrl Pts',(68.8249754182403,-6.21925,2.03655253223446E-12));
#34459=CARTESIAN_POINT('Ctrl Pts',(68.883775169714,-6.2192500000006,-1.83816020915543));
#34460=CARTESIAN_POINT('Ctrl Pts',(68.9425749211877,-5.35502977485132,-3.65808141345784));
#34461=CARTESIAN_POINT('Ctrl Pts',(69.0013746726614,-3.93049712175981,-4.81977830800731));
#34462=CARTESIAN_POINT('Ctrl Pts',(69.0601744241351,-2.5059644686683,-5.98147520255679));
#34463=CARTESIAN_POINT('Ctrl Pts',(69.1189741756088,-0.549389021420466,
-6.46189408921042));
#34464=CARTESIAN_POINT('Ctrl Pts',(69.1777739270825,1.25118869866754,-6.09209302315934));
#34465=CARTESIAN_POINT('Ctrl Pts',(69.2365736785562,3.05176641875554,-5.72229195710825));
#34466=CARTESIAN_POINT('Ctrl Pts',(69.2953734300299,4.66061422075116,-4.50960958425027));
#34467=CARTESIAN_POINT('Ctrl Pts',(69.3541731815036,5.51197192302658,-2.88049233331155));
#34468=CARTESIAN_POINT('Ctrl Pts',(69.4129729329773,6.36332962530201,-1.25137508237283));
#34469=CARTESIAN_POINT('Ctrl Pts',(69.471772684451,6.44030216377297,0.761847462639996));
#34470=CARTESIAN_POINT('Ctrl Pts',(69.5305724359247,5.71582172177486,2.45121451680319));
#34471=CARTESIAN_POINT('Ctrl Pts',(69.5893721873984,4.99134127977674,4.14058157096639));
#34472=CARTESIAN_POINT('Ctrl Pts',(69.6481719388721,3.47978506146551,5.47256790209417));
#34473=CARTESIAN_POINT('Ctrl Pts',(69.7069716903458,1.71270012775744,5.97877318811139));
#34474=CARTESIAN_POINT('Ctrl Pts',(69.7657714418195,-0.0543848059506302,
6.48497847412862));
#34475=CARTESIAN_POINT('Ctrl Pts',(69.8245711932932,-2.04193092337342,6.1553571481435));
#34476=CARTESIAN_POINT('Ctrl Pts',(69.8833709447669,-3.55100669662373,5.10582236305117));
#34477=CARTESIAN_POINT('Ctrl Pts',(69.9421706962406,-5.06008246987404,4.05628757795884));
#34478=CARTESIAN_POINT('Ctrl Pts',(70.0009704477143,-6.06074051980802,2.30766719190333));
#34479=CARTESIAN_POINT('Ctrl Pts',(70.059770199188,-6.20109393743667,0.474873184741103));
#34480=CARTESIAN_POINT('Ctrl Pts',(70.0648386055388,-6.21319208641575,0.316890462829203));
#34481=CARTESIAN_POINT('Ctrl Pts',(70.0699070118895,-6.21924999999995,0.158445276458607));
#34482=CARTESIAN_POINT('Ctrl Pts',(70.0749754182403,-6.21925,1.99388538006182E-12));
#34483=CARTESIAN_POINT('Ctrl Pts',(69.0714645817596,-6.20678839560337,0.00251771313458389));
#34484=CARTESIAN_POINT('Ctrl Pts',(69.1030322235516,-6.20695393622908,-0.987187120888528));
#34485=CARTESIAN_POINT('Ctrl Pts',(69.1676851327505,-5.74899888494865,-3.01546442731683));
#34486=CARTESIAN_POINT('Ctrl Pts',(69.2654233093567,-3.62859134903107,-5.35878348065247));
#34487=CARTESIAN_POINT('Ctrl Pts',(69.3646791115776,-0.62823592000139,-6.45958714174554));
#34488=CARTESIAN_POINT('Ctrl Pts',(69.4639349137987,2.52830110610206,-5.95780469931484));
#34489=CARTESIAN_POINT('Ctrl Pts',(69.5962759834268,5.95652483419779,-3.3963489535312));
#34490=CARTESIAN_POINT('Ctrl Pts',(69.7617023204619,6.96369965258984,2.35963460035952));
#34491=CARTESIAN_POINT('Ctrl Pts',(69.9602139249039,1.78096623639146,7.13640802565527));
#34492=CARTESIAN_POINT('Ctrl Pts',(70.1468013453366,-4.61505740066332,5.46838819564559));
#34493=CARTESIAN_POINT('Ctrl Pts',(70.2672182309551,-6.20779982877329,1.68812296321986));
#34494=CARTESIAN_POINT('Ctrl Pts',(70.3214645817596,-6.22327189076832,-0.00449888440332329));
#34495=CARTESIAN_POINT('Origin',(28.1999754182402,0.,0.));
#34496=CARTESIAN_POINT('',(67.5749754182403,-6.22716903015256,-0.00354123602412358));
#34497=CARTESIAN_POINT('',(67.8214645817596,-6.21925,1.42747096013558E-12));
#34498=CARTESIAN_POINT('',(28.1999754182402,-6.21925,5.68729293530136E-12));
#34499=CARTESIAN_POINT('Ctrl Pts',(67.5749754182403,-6.22716903015256,-0.00354123602412323));
#34500=CARTESIAN_POINT('Ctrl Pts',(67.5810286846097,-6.22849064190086,-0.192188270096255));
#34501=CARTESIAN_POINT('Ctrl Pts',(67.6532524857932,-6.13655344587958,-2.44169010369456));
#34502=CARTESIAN_POINT('Ctrl Pts',(67.7916468217906,-3.40809791078333,-6.51499441152191));
#34503=CARTESIAN_POINT('Ctrl Pts',(67.9901584262328,3.63494514635811,-6.39141334988969));
#34504=CARTESIAN_POINT('Ctrl Pts',(68.1555847632678,6.70899997741019,-1.41894774382875));
#34505=CARTESIAN_POINT('Ctrl Pts',(68.2879258328959,5.84773120199377,2.77243208544916));
#34506=CARTESIAN_POINT('Ctrl Pts',(68.387181635117,3.82264019194717,5.24510836053448));
#34507=CARTESIAN_POINT('Ctrl Pts',(68.486437437338,0.848644543025793,6.4157715664878));
#34508=CARTESIAN_POINT('Ctrl Pts',(68.6187785069662,-3.40513155320004,5.95224512547316));
#34509=CARTESIAN_POINT('Ctrl Pts',(68.7316245006002,-5.99206689653167,2.91734514626186));
#34510=CARTESIAN_POINT('Ctrl Pts',(68.8113852268273,-6.22478355345344,0.432318045390996));
#34511=CARTESIAN_POINT('Ctrl Pts',(68.8249754182403,-6.22080542650654,0.00799904362253197));
#34512=CARTESIAN_POINT('Ctrl Pts',(67.8214645817596,-6.21925,1.42747096013558E-12));
#34513=CARTESIAN_POINT('Ctrl Pts',(67.8802643332333,-6.21925000000042,-1.83816020915604));
#34514=CARTESIAN_POINT('Ctrl Pts',(67.939064084707,-5.35502977485096,-3.65808141345836));
#34515=CARTESIAN_POINT('Ctrl Pts',(67.9978638361807,-3.93049712175934,-4.8197783080077));
#34516=CARTESIAN_POINT('Ctrl Pts',(68.0566635876544,-2.50596446866772,-5.98147520255704));
#34517=CARTESIAN_POINT('Ctrl Pts',(68.1154633391281,-0.549389021419833,
-6.46189408921047));
#34518=CARTESIAN_POINT('Ctrl Pts',(68.1742630906018,1.25118869866813,-6.09209302315921));
#34519=CARTESIAN_POINT('Ctrl Pts',(68.2330628420755,3.0517664187561,-5.72229195710796));
#34520=CARTESIAN_POINT('Ctrl Pts',(68.2918625935492,4.6606142207516,-4.50960958424982));
#34521=CARTESIAN_POINT('Ctrl Pts',(68.3506623450229,5.51197192302687,-2.88049233331101));
#34522=CARTESIAN_POINT('Ctrl Pts',(68.4094620964966,6.36332962530213,-1.25137508237221));
#34523=CARTESIAN_POINT('Ctrl Pts',(68.4682618479703,6.4403021637729,0.761847462640626));
#34524=CARTESIAN_POINT('Ctrl Pts',(68.527061599444,5.71582172177462,2.45121451680375));
#34525=CARTESIAN_POINT('Ctrl Pts',(68.5858613509177,4.99134127977633,4.14058157096688));
#34526=CARTESIAN_POINT('Ctrl Pts',(68.6446611023914,3.47978506146497,5.47256790209451));
#34527=CARTESIAN_POINT('Ctrl Pts',(68.7034608538651,1.71270012775685,5.97877318811156));
#34528=CARTESIAN_POINT('Ctrl Pts',(68.7622606053388,-0.054384805951265,
6.48497847412861));
#34529=CARTESIAN_POINT('Ctrl Pts',(68.8210603568125,-2.04193092337402,6.15535714814329));
#34530=CARTESIAN_POINT('Ctrl Pts',(68.8798601082862,-3.55100669662423,5.10582236305082));
#34531=CARTESIAN_POINT('Ctrl Pts',(68.9386598597599,-5.06008246987444,4.05628757795835));
#34532=CARTESIAN_POINT('Ctrl Pts',(68.9974596112336,-6.06074051980825,2.30766719190274));
#34533=CARTESIAN_POINT('Ctrl Pts',(69.0562593627073,-6.20109393743672,0.474873184740495));
#34534=CARTESIAN_POINT('Ctrl Pts',(69.0613277690581,-6.21319208641577,0.31689046282877));
#34535=CARTESIAN_POINT('Ctrl Pts',(69.0663961754089,-6.21924999999995,0.158445276458352));
#34536=CARTESIAN_POINT('Ctrl Pts',(69.0714645817596,-6.21925,1.91508895708806E-12));
#34537=CARTESIAN_POINT('Origin',(28.1999754182402,0.,0.));
#34538=CARTESIAN_POINT('',(66.3249754182403,-6.21259519566301,-0.00324245267844449));
#34539=CARTESIAN_POINT('',(66.5714645817596,-6.22114348643294,-0.0015202752725002));
#34540=CARTESIAN_POINT('',(28.1999754182402,-6.21925,5.68729293530136E-12));
#34541=CARTESIAN_POINT('Ctrl Pts',(66.3249754182403,-6.21259519566301,-0.003242452678444));
#34542=CARTESIAN_POINT('Ctrl Pts',(66.3506721423922,-6.21662143089998,-0.808861812537382));
#34543=CARTESIAN_POINT('Ctrl Pts',(66.4425394013581,-5.69514649096048,-3.68402373808155));
#34544=CARTESIAN_POINT('Ctrl Pts',(66.6005771951379,-1.34895379295012,-7.22795352199158));
#34545=CARTESIAN_POINT('Ctrl Pts',(66.7660035321732,4.20849394244699,-5.41411806724503));
#34546=CARTESIAN_POINT('Ctrl Pts',(66.8983446018011,6.25597908877345,-1.65682395344729));
#34547=CARTESIAN_POINT('Ctrl Pts',(66.9976004040223,6.30519641260689,1.53890622628911));
#34548=CARTESIAN_POINT('Ctrl Pts',(67.0968562062432,4.78925485703138,4.35262885196658));
#34549=CARTESIAN_POINT('Ctrl Pts',(67.2291972758714,1.24102420380131,6.74417930312503));
#34550=CARTESIAN_POINT('Ctrl Pts',(67.388570346537,-4.31609141344847,5.82855040460842));
#34551=CARTESIAN_POINT('Ctrl Pts',(67.5148581497957,-6.21404360605863,1.86998351846371));
#34552=CARTESIAN_POINT('Ctrl Pts',(67.5749754182403,-6.22716903015256,-0.00354123602412323));
#34553=CARTESIAN_POINT('Ctrl Pts',(66.5714645817596,-6.22114348643294,-0.00152027527249955));
#34554=CARTESIAN_POINT('Ctrl Pts',(66.5761486043024,-6.22148244516996,-0.147527676541695));
#34555=CARTESIAN_POINT('Ctrl Pts',(66.6139178942523,-6.18170946866711,-1.32459121785407));
#34556=CARTESIAN_POINT('Ctrl Pts',(66.6847724516092,-5.45227135475848,-3.4864132116906));
#34557=CARTESIAN_POINT('Ctrl Pts',(66.8171135212372,-2.35612050115225,-6.43993724590316));
#34558=CARTESIAN_POINT('Ctrl Pts',(66.9825398582723,3.48975044558929,-6.47183364038364));
#34559=CARTESIAN_POINT('Ctrl Pts',(67.1810514627144,7.33067472739079,-0.567002756194563));
#34560=CARTESIAN_POINT('Ctrl Pts',(67.3795630671566,4.45391682219975,5.85003491379102));
#34561=CARTESIAN_POINT('Ctrl Pts',(67.5780746715986,-2.50983236811194,6.91113104420389));
#34562=CARTESIAN_POINT('Ctrl Pts',(67.7253751764663,-5.95182529533825,3.00613154281414));
#34563=CARTESIAN_POINT('Ctrl Pts',(67.80650514652,-6.22533619653189,0.470469326291353));
#34564=CARTESIAN_POINT('Ctrl Pts',(67.8214645817596,-6.22287026600109,0.00237337644969353));
#34565=CARTESIAN_POINT('Origin',(28.1999754182402,0.,0.));
#34566=CARTESIAN_POINT('',(65.0749754182404,-6.21356978932969,0.00431476290370225));
#34567=CARTESIAN_POINT('',(65.3214645817596,-6.21925,1.15928100452578E-12));
#34568=CARTESIAN_POINT('',(28.1999754182402,-6.21925,5.68729293530136E-12));
#34569=CARTESIAN_POINT('Ctrl Pts',(65.0749754182404,-6.21356978932969,0.00431476290370186));
#34570=CARTESIAN_POINT('Ctrl Pts',(65.1203156001746,-6.20196410271433,-1.41654032948276));
#34571=CARTESIAN_POINT('Ctrl Pts',(65.2318263169229,-5.01369486695274,-4.92727852199253));
#34572=CARTESIAN_POINT('Ctrl Pts',(65.3764223010783,-0.280080766866481,
-6.8516896061695));
#34573=CARTESIAN_POINT('Ctrl Pts',(65.5087633707064,3.70893826617409,-5.30340616226556));
#34574=CARTESIAN_POINT('Ctrl Pts',(65.6080191729274,5.80921341909733,-2.89426564405251));
#34575=CARTESIAN_POINT('Ctrl Pts',(65.7072749751485,6.46744912735215,0.233327601020761));
#34576=CARTESIAN_POINT('Ctrl Pts',(65.8396160447766,5.30092577216001,4.35020478294281));
#34577=CARTESIAN_POINT('Ctrl Pts',(66.0050423818117,0.281730743593815,7.34735437050459));
#34578=CARTESIAN_POINT('Ctrl Pts',(66.1778572621018,-5.20975654679889,4.61816001860487));
#34579=CARTESIAN_POINT('Ctrl Pts',(66.2845016075781,-6.20625364482176,1.26565412900383));
#34580=CARTESIAN_POINT('Ctrl Pts',(66.3249754182403,-6.21259519566301,-0.003242452678444));
#34581=CARTESIAN_POINT('Ctrl Pts',(65.3214645817597,-6.21837015127254,-0.000938862326199455));
#34582=CARTESIAN_POINT('Ctrl Pts',(65.3457920620849,-6.22137299609146,-0.763310719959148));
#34583=CARTESIAN_POINT('Ctrl Pts',(65.4362900772242,-5.72097133082025,-3.5991317981514));
#34584=CARTESIAN_POINT('Ctrl Pts',(65.5929586271775,-1.51176119750446,-7.19566303681453));
#34585=CARTESIAN_POINT('Ctrl Pts',(65.7914702316198,5.23321851206271,-5.16465955355726));
#34586=CARTESIAN_POINT('Ctrl Pts',(65.9899818360617,7.17781718660405,1.59349450345578));
#34587=CARTESIAN_POINT('Ctrl Pts',(66.1884934405039,2.54376969957746,6.89871177591126));
#34588=CARTESIAN_POINT('Ctrl Pts',(66.353919777539,-3.23937625907777,6.04404973191034));
#34589=CARTESIAN_POINT('Ctrl Pts',(66.4815768246242,-5.79506225091564,2.80294095321662));
#34590=CARTESIAN_POINT('Ctrl Pts',(66.5430633368954,-6.21908823370923,0.883785445935368));
#34591=CARTESIAN_POINT('Ctrl Pts',(66.5714645817596,-6.22114348643294,-0.00152027527249955));
#34592=CARTESIAN_POINT('Origin',(28.1999754182402,0.,0.));
#34593=CARTESIAN_POINT('',(63.8249754182403,-6.22975058477463,-0.000685955996849441));
#34594=CARTESIAN_POINT('',(64.0714645817597,-6.21853427270105,0.000112577972291501));
#34595=CARTESIAN_POINT('',(28.1999754182402,-6.21925,5.68729293530136E-12));
#34596=CARTESIAN_POINT('Ctrl Pts',(63.8249754182403,-6.22975058477463,-0.000685955996849274));
#34597=CARTESIAN_POINT('Ctrl Pts',(63.889959057957,-6.22639346802808,-2.02031191703693));
#34598=CARTESIAN_POINT('Ctrl Pts',(63.9880279650808,-4.60005908095223,-5.06504725367468));
#34599=CARTESIAN_POINT('Ctrl Pts',(64.1191821396116,-0.590183859376729,
-6.44468951899971));
#34600=CARTESIAN_POINT('Ctrl Pts',(64.2184379418327,2.56899111035366,-5.9602029195333));
#34601=CARTESIAN_POINT('Ctrl Pts',(64.3176937440537,5.09045728081569,-3.99619627350351));
#34602=CARTESIAN_POINT('Ctrl Pts',(64.4500348136817,6.85670021738249,-0.098781700014005));
#34603=CARTESIAN_POINT('Ctrl Pts',(64.615461150717,4.95753380652983,5.43008720152017));
#34604=CARTESIAN_POINT('Ctrl Pts',(64.8139727551589,-1.8840609360603,7.10708088361284));
#34605=CARTESIAN_POINT('Ctrl Pts',(64.9671441776669,-5.82547528679035,3.37766727413955));
#34606=CARTESIAN_POINT('Ctrl Pts',(65.0541450653606,-6.21890171649222,0.657089227026568));
#34607=CARTESIAN_POINT('Ctrl Pts',(65.0749754182404,-6.21356978932969,0.00431476290370186));
#34608=CARTESIAN_POINT('Ctrl Pts',(64.0714645817596,-6.21925,1.20194898390342E-12));
#34609=CARTESIAN_POINT('Ctrl Pts',(64.1302643332333,-6.21925000000036,-1.83816020915627));
#34610=CARTESIAN_POINT('Ctrl Pts',(64.189064084707,-5.35502977485083,-3.65808141345855));
#34611=CARTESIAN_POINT('Ctrl Pts',(64.2478638361807,-3.93049712175916,-4.81977830800784));
#34612=CARTESIAN_POINT('Ctrl Pts',(64.3066635876544,-2.5059644686675,-5.98147520255713));
#34613=CARTESIAN_POINT('Ctrl Pts',(64.3654633391281,-0.549389021419599,
-6.46189408921049));
#34614=CARTESIAN_POINT('Ctrl Pts',(64.4242630906018,1.25118869866836,-6.09209302315917));
#34615=CARTESIAN_POINT('Ctrl Pts',(64.4830628420755,3.05176641875631,-5.72229195710785));
#34616=CARTESIAN_POINT('Ctrl Pts',(64.5418625935492,4.66061422075176,-4.50960958424965));
#34617=CARTESIAN_POINT('Ctrl Pts',(64.6006623450229,5.51197192302697,-2.88049233331081));
#34618=CARTESIAN_POINT('Ctrl Pts',(64.6594620964966,6.36332962530218,-1.25137508237198));
#34619=CARTESIAN_POINT('Ctrl Pts',(64.7182618479703,6.44030216377287,0.76184746264086));
#34620=CARTESIAN_POINT('Ctrl Pts',(64.777061599444,5.71582172177453,2.45121451680396));
#34621=CARTESIAN_POINT('Ctrl Pts',(64.8358613509177,4.99134127977619,4.14058157096706));
#34622=CARTESIAN_POINT('Ctrl Pts',(64.8946611023914,3.47978506146477,5.47256790209463));
#34623=CARTESIAN_POINT('Ctrl Pts',(64.9534608538651,1.71270012775664,5.97877318811162));
#34624=CARTESIAN_POINT('Ctrl Pts',(65.0122606053388,-0.0543848059515001,
6.48497847412861));
#34625=CARTESIAN_POINT('Ctrl Pts',(65.0710603568125,-2.04193092337424,6.15535714814322));
#34626=CARTESIAN_POINT('Ctrl Pts',(65.1298601082862,-3.55100669662442,5.10582236305069));
#34627=CARTESIAN_POINT('Ctrl Pts',(65.1886598597599,-5.06008246987459,4.05628757795816));
#34628=CARTESIAN_POINT('Ctrl Pts',(65.2474596112336,-6.06074051980833,2.30766719190252));
#34629=CARTESIAN_POINT('Ctrl Pts',(65.3062593627073,-6.20109393743674,0.47487318474027));
#34630=CARTESIAN_POINT('Ctrl Pts',(65.3113277690581,-6.21319208641579,0.316890462828369));
#34631=CARTESIAN_POINT('Ctrl Pts',(65.3163961754089,-6.21924999999997,0.158445276457773));
#34632=CARTESIAN_POINT('Ctrl Pts',(65.3214645817596,-6.21925,1.15928183173078E-12));
#34633=CARTESIAN_POINT('Origin',(28.1999754182402,0.,0.));
#34634=CARTESIAN_POINT('',(62.5749754182403,-6.21856955346695,-0.000259107838776135));
#34635=CARTESIAN_POINT('',(62.8214645817596,-6.22934305414637,0.00327033652799832));
#34636=CARTESIAN_POINT('',(28.1999754182402,-6.21925,5.68729293530136E-12));
#34637=CARTESIAN_POINT('Ctrl Pts',(62.5749754182404,-6.21260916379183,-0.00252876991957987));
#34638=CARTESIAN_POINT('Ctrl Pts',(62.5934319809255,-6.21745248917224,-0.580222709882177));
#34639=CARTESIAN_POINT('Ctrl Pts',(62.6449738110176,-6.01215797913732,-2.1915756033502));
#34640=CARTESIAN_POINT('Ctrl Pts',(62.7296009085167,-4.61050649279502,-4.54153827068194));
#34641=CARTESIAN_POINT('Ctrl Pts',(62.828856710738,-1.88480796006642,-6.2105742987874));
#34642=CARTESIAN_POINT('Ctrl Pts',(62.9281125129588,1.30876242173983,-6.33793979993621));
#34643=CARTESIAN_POINT('Ctrl Pts',(63.0604535825871,5.17340855136809,-4.50110427072531));
#34644=CARTESIAN_POINT('Ctrl Pts',(63.225879919622,7.29142614877463,0.947677780663159));
#34645=CARTESIAN_POINT('Ctrl Pts',(63.4243915240643,3.14821152092017,6.64447503694298));
#34646=CARTESIAN_POINT('Ctrl Pts',(63.6229031285063,-3.87306471768808,6.24977231502176));
#34647=CARTESIAN_POINT('Ctrl Pts',(63.7564310932317,-6.21295322572177,2.12964199441194));
#34648=CARTESIAN_POINT('Ctrl Pts',(63.823788523143,-6.22981190090628,0.0362015461805261));
#34649=CARTESIAN_POINT('Ctrl Pts',(63.8249754182403,-6.22975058477463,-0.000685955996849274));
#34650=CARTESIAN_POINT('Ctrl Pts',(62.8214645817596,-6.22934305414637,0.00327033652799856));
#34651=CARTESIAN_POINT('Ctrl Pts',(62.8850789776498,-6.22299644639126,-1.97466634164587));
#34652=CARTESIAN_POINT('Ctrl Pts',(63.014863908354,-4.12949038798452,-6.0315003317796));
#34653=CARTESIAN_POINT('Ctrl Pts',(63.2108193738721,2.7683587964008,-6.81149571470196));
#34654=CARTESIAN_POINT('Ctrl Pts',(63.4093309783144,7.22635244835865,-1.35750460444815));
#34655=CARTESIAN_POINT('Ctrl Pts',(63.5747573153493,5.41909355797858,4.20208528057022));
#34656=CARTESIAN_POINT('Ctrl Pts',(63.7070983849776,1.66422455917251,6.25401443880813));
#34657=CARTESIAN_POINT('Ctrl Pts',(63.8063541871984,-1.53144515668549,6.30701275558833));
#34658=CARTESIAN_POINT('Ctrl Pts',(63.9056099894197,-4.34695939124221,4.79440132186115));
#34659=CARTESIAN_POINT('Ctrl Pts',(63.99398012094,-5.94670819129815,2.42697794624009));
#34660=CARTESIAN_POINT('Ctrl Pts',(64.0492649850533,-6.21443109280533,0.696924413737985));
#34661=CARTESIAN_POINT('Ctrl Pts',(64.0714645817596,-6.20983994024725,0.00148012439544501));
#34662=CARTESIAN_POINT('Origin',(28.1999754182402,0.,0.));
#34663=CARTESIAN_POINT('',(61.3249754182403,-6.21925,8.78461714269987E-13));
#34664=CARTESIAN_POINT('',(61.5714645817597,-6.21695893348969,-0.00516800745213986));
#34665=CARTESIAN_POINT('',(28.1999754182402,-6.21925,5.68729293530136E-12));
#34666=CARTESIAN_POINT('Ctrl Pts',(61.3249754182403,-6.21925,8.78461714269987E-13));
#34667=CARTESIAN_POINT('Ctrl Pts',(61.383775169714,-6.21925000000026,-1.83816020915659));
#34668=CARTESIAN_POINT('Ctrl Pts',(61.4425749211877,-5.35502977485064,-3.65808141345883));
#34669=CARTESIAN_POINT('Ctrl Pts',(61.5013746726614,-3.93049712175891,-4.81977830800805));
#34670=CARTESIAN_POINT('Ctrl Pts',(61.5601744241351,-2.50596446866719,-5.98147520255726));
#34671=CARTESIAN_POINT('Ctrl Pts',(61.6189741756088,-0.549389021419263,
-6.46189408921052));
#34672=CARTESIAN_POINT('Ctrl Pts',(61.6777739270825,1.25118869866867,-6.0920930231591));
#34673=CARTESIAN_POINT('Ctrl Pts',(61.7365736785562,3.05176641875661,-5.72229195710769));
#34674=CARTESIAN_POINT('Ctrl Pts',(61.7953734300299,4.660614220752,-4.5096095842494));
#34675=CARTESIAN_POINT('Ctrl Pts',(61.8541731815036,5.51197192302712,-2.88049233331053));
#34676=CARTESIAN_POINT('Ctrl Pts',(61.9129729329773,6.36332962530224,-1.25137508237165));
#34677=CARTESIAN_POINT('Ctrl Pts',(61.971772684451,6.44030216377283,0.761847462641195));
#34678=CARTESIAN_POINT('Ctrl Pts',(62.0305724359247,5.7158217217744,2.45121451680426));
#34679=CARTESIAN_POINT('Ctrl Pts',(62.0893721873984,4.99134127977597,4.14058157096732));
#34680=CARTESIAN_POINT('Ctrl Pts',(62.1481719388721,3.47978506146449,5.47256790209481));
#34681=CARTESIAN_POINT('Ctrl Pts',(62.2069716903458,1.71270012775632,5.97877318811171));
#34682=CARTESIAN_POINT('Ctrl Pts',(62.2657714418195,-0.054384805951837,
6.48497847412861));
#34683=CARTESIAN_POINT('Ctrl Pts',(62.3245711932932,-2.04193092337456,6.15535714814311));
#34684=CARTESIAN_POINT('Ctrl Pts',(62.3833709447669,-3.55100669662468,5.10582236305051));
#34685=CARTESIAN_POINT('Ctrl Pts',(62.4421706962406,-5.0600824698748,4.0562875779579));
#34686=CARTESIAN_POINT('Ctrl Pts',(62.5009704477143,-6.06074051980845,2.3076671919022));
#34687=CARTESIAN_POINT('Ctrl Pts',(62.559770199188,-6.20109393743676,0.474873184739948));
#34688=CARTESIAN_POINT('Ctrl Pts',(62.5648386055388,-6.2131920864158,0.316890462828163));
#34689=CARTESIAN_POINT('Ctrl Pts',(62.5699070118896,-6.21924999999997,0.158445276457685));
#34690=CARTESIAN_POINT('Ctrl Pts',(62.5749754182403,-6.21925,1.18931799484743E-12));
#34691=CARTESIAN_POINT('Ctrl Pts',(61.5714645817597,-6.21695893348969,-0.00516800745214034));
#34692=CARTESIAN_POINT('Ctrl Pts',(61.5885519006182,-6.22200109994744,-0.53992295050933));
#34693=CARTESIAN_POINT('Ctrl Pts',(61.6718097542908,-5.91572340500266,-3.14007559790216));
#34694=CARTESIAN_POINT('Ctrl Pts',(61.8212381427774,-2.28199696173699,-6.98947595772644));
#34695=CARTESIAN_POINT('Ctrl Pts',(62.0197497472196,4.64330776244168,-5.70111230219558));
#34696=CARTESIAN_POINT('Ctrl Pts',(62.1851760842546,6.85135343285645,-0.288187149949455));
#34697=CARTESIAN_POINT('Ctrl Pts',(62.3175171538827,5.30779068198273,3.70266094321786));
#34698=CARTESIAN_POINT('Ctrl Pts',(62.4167729561038,2.90113679133094,5.80578500162336));
#34699=CARTESIAN_POINT('Ctrl Pts',(62.5160287583248,-0.225675472877136,
6.46772066226701));
#34700=CARTESIAN_POINT('Ctrl Pts',(62.6483698279529,-4.34392994578106,5.30606900835795));
#34701=CARTESIAN_POINT('Ctrl Pts',(62.7501817690978,-6.19218467788144,2.21918086720454));
#34702=CARTESIAN_POINT('Ctrl Pts',(62.8189084428357,-6.22959807206944,0.0827473300813655));
#34703=CARTESIAN_POINT('Ctrl Pts',(62.8214645817596,-6.22934305414637,0.00327033652799856));
#34704=CARTESIAN_POINT('Origin',(28.1999754182402,0.,0.));
#34705=CARTESIAN_POINT('',(60.0749754182404,-6.21925,7.44365506732958E-13));
#34706=CARTESIAN_POINT('',(60.3214645817597,-6.21111205730243,0.00169677517069255));
#34707=CARTESIAN_POINT('',(28.1999754182402,-6.21925,5.68729293530136E-12));
#34708=CARTESIAN_POINT('Ctrl Pts',(60.0749754182404,-6.22004574063539,0.00250981053279774));
#34709=CARTESIAN_POINT('Ctrl Pts',(60.0996336290834,-6.21761940426262,-0.766580500658636));
#34710=CARTESIAN_POINT('Ctrl Pts',(60.1573771073334,-5.87450282726596,-2.57066518997162));
#34711=CARTESIAN_POINT('Ctrl Pts',(60.2812911203974,-3.57518444437901,-5.85167940714288));
#34712=CARTESIAN_POINT('Ctrl Pts',(60.4467174574326,2.15053713527687,-7.03122880361549));
#34713=CARTESIAN_POINT('Ctrl Pts',(60.6452290618746,7.07649152718233,-1.99588375481379));
#34714=CARTESIAN_POINT('Ctrl Pts',(60.8437406663167,5.5162418506764,4.86120974057477));
#34715=CARTESIAN_POINT('Ctrl Pts',(61.0422522707589,-1.1034200191743,7.26948778940321));
#34716=CARTESIAN_POINT('Ctrl Pts',(61.2026638547334,-5.61407165712723,3.83602481861383));
#34717=CARTESIAN_POINT('Ctrl Pts',(61.2969049038939,-6.21974059825275,0.879711363588332));
#34718=CARTESIAN_POINT('Ctrl Pts',(61.3249754182403,-6.21712757775053,-3.09561547350186E-5));
#34719=CARTESIAN_POINT('Ctrl Pts',(60.3214645817597,-6.21111205730243,0.0016967751706929));
#34720=CARTESIAN_POINT('Ctrl Pts',(60.3581953584006,-6.20814873088829,-1.15054126823442));
#34721=CARTESIAN_POINT('Ctrl Pts',(60.4610966698556,-5.34657007883321,-4.38263206448972));
#34722=CARTESIAN_POINT('Ctrl Pts',(60.6301685161248,-0.133209051532416,
-7.35154703498433));
#34723=CARTESIAN_POINT('Ctrl Pts',(60.7955948531599,5.0470729870606,-4.64232161300714));
#34724=CARTESIAN_POINT('Ctrl Pts',(60.9279359227879,6.44398673196168,-0.597808483107745));
#34725=CARTESIAN_POINT('Ctrl Pts',(61.027191725009,5.96323825064499,2.56193749594574));
#34726=CARTESIAN_POINT('Ctrl Pts',(61.12644752723,4.00221625291053,5.08572561677413));
#34727=CARTESIAN_POINT('Ctrl Pts',(61.2587885968582,0.106894138300333,6.85657854461737));
#34728=CARTESIAN_POINT('Ctrl Pts',(61.4071276150346,-4.8528948701387,5.15944898606185));
#34729=CARTESIAN_POINT('Ctrl Pts',(61.5223813658041,-6.20247534205104,1.53091220329418));
#34730=CARTESIAN_POINT('Ctrl Pts',(61.5714645817597,-6.21695893348969,-0.00516800745214034));
#34731=CARTESIAN_POINT('Origin',(28.1999754182402,0.,0.));
#34732=CARTESIAN_POINT('',(58.8249754182404,-6.21925,6.10272585865188E-13));
#34733=CARTESIAN_POINT('',(59.0714645817597,-6.22408309271093,0.00477558807787742));
#34734=CARTESIAN_POINT('',(28.1999754182402,-6.21925,5.68729293530136E-12));
#34735=CARTESIAN_POINT('Ctrl Pts',(58.8249754182404,-6.21925,6.10272585865188E-13));
#34736=CARTESIAN_POINT('Ctrl Pts',(58.8837751697141,-6.21925000000018,-1.83816020915686));
#34737=CARTESIAN_POINT('Ctrl Pts',(58.9425749211877,-5.35502977485048,-3.65808141345906));
#34738=CARTESIAN_POINT('Ctrl Pts',(59.0013746726614,-3.93049712175871,-4.81977830800821));
#34739=CARTESIAN_POINT('Ctrl Pts',(59.0601744241351,-2.50596446866693,-5.98147520255737));
#34740=CARTESIAN_POINT('Ctrl Pts',(59.1189741756088,-0.549389021418984,
-6.46189408921054));
#34741=CARTESIAN_POINT('Ctrl Pts',(59.1777739270825,1.25118869866893,-6.09209302315905));
#34742=CARTESIAN_POINT('Ctrl Pts',(59.2365736785562,3.05176641875685,-5.72229195710755));
#34743=CARTESIAN_POINT('Ctrl Pts',(59.2953734300299,4.66061422075219,-4.5096095842492));
#34744=CARTESIAN_POINT('Ctrl Pts',(59.3541731815036,5.51197192302724,-2.88049233331029));
#34745=CARTESIAN_POINT('Ctrl Pts',(59.4129729329773,6.3633296253023,-1.25137508237137));
#34746=CARTESIAN_POINT('Ctrl Pts',(59.471772684451,6.4403021637728,0.761847462641473));
#34747=CARTESIAN_POINT('Ctrl Pts',(59.5305724359247,5.71582172177429,2.45121451680451));
#34748=CARTESIAN_POINT('Ctrl Pts',(59.5893721873984,4.99134127977579,4.14058157096754));
#34749=CARTESIAN_POINT('Ctrl Pts',(59.6481719388721,3.47978506146425,5.47256790209496));
#34750=CARTESIAN_POINT('Ctrl Pts',(59.7069716903458,1.71270012775607,5.97877318811178));
#34751=CARTESIAN_POINT('Ctrl Pts',(59.7657714418195,-0.0543848059521168,
6.48497847412861));
#34752=CARTESIAN_POINT('Ctrl Pts',(59.8245711932932,-2.04193092337483,6.15535714814303));
#34753=CARTESIAN_POINT('Ctrl Pts',(59.8833709447669,-3.5510066966249,5.10582236305035));
#34754=CARTESIAN_POINT('Ctrl Pts',(59.9421706962406,-5.06008246987498,4.05628757795768));
#34755=CARTESIAN_POINT('Ctrl Pts',(60.0009704477143,-6.06074051980855,2.30766719190194));
#34756=CARTESIAN_POINT('Ctrl Pts',(60.059770199188,-6.20109393743678,0.47487318473968));
#34757=CARTESIAN_POINT('Ctrl Pts',(60.0648386055388,-6.21319208641582,0.316890462827836));
#34758=CARTESIAN_POINT('Ctrl Pts',(60.0699070118896,-6.21924999999998,0.158445276457299));
#34759=CARTESIAN_POINT('Ctrl Pts',(60.0749754182404,-6.21925,7.44367150067587E-13));
#34760=CARTESIAN_POINT('Ctrl Pts',(59.0714645817597,-6.22408309271093,0.00477558807787732));
#34761=CARTESIAN_POINT('Ctrl Pts',(59.1278388161831,-6.20819293747344,-1.7543657142207));
#34762=CARTESIAN_POINT('Ctrl Pts',(59.2503835854205,-4.50893443442348,-5.60461480076411));
#34763=CARTESIAN_POINT('Ctrl Pts',(59.406013622065,0.858584021869272,-6.80344979938125));
#34764=CARTESIAN_POINT('Ctrl Pts',(59.5383546916932,4.53608016947545,-4.61587658850033));
#34765=CARTESIAN_POINT('Ctrl Pts',(59.6376104939142,6.20833994062302,-1.89215468415061));
#34766=CARTESIAN_POINT('Ctrl Pts',(59.7368662961353,6.33948382661728,1.30126276986307));
#34767=CARTESIAN_POINT('Ctrl Pts',(59.8692073657633,4.50722204056254,5.16807944718129));
#34768=CARTESIAN_POINT('Ctrl Pts',(60.0346337027984,-0.939050263787701,
7.2925422906609));
#34769=CARTESIAN_POINT('Ctrl Pts',(60.1964145305996,-5.58575588337288,3.92144569883786));
#34770=CARTESIAN_POINT('Ctrl Pts',(60.2920248235866,-6.21348716670654,0.925216843563736));
#34771=CARTESIAN_POINT('Ctrl Pts',(60.3214645817597,-6.21111205730243,0.0016967751706929));
#34772=CARTESIAN_POINT('Origin',(28.1999754182402,0.,0.));
#34773=CARTESIAN_POINT('',(57.5749754182404,-6.21812662533432,-0.000394576859186467));
#34774=CARTESIAN_POINT('',(57.8214645817597,-6.22441924678459,-0.00707629521854547));
#34775=CARTESIAN_POINT('',(28.1999754182402,-6.21925,5.68729293530136E-12));
#34776=CARTESIAN_POINT('Ctrl Pts',(57.5749754182404,-6.20740910248718,-0.00415902574651419));
#34777=CARTESIAN_POINT('Ctrl Pts',(57.6058352772412,-6.20996092781725,-0.971356541319267));
#34778=CARTESIAN_POINT('Ctrl Pts',(57.7028656710561,-5.544781642729,-4.00770145453599));
#34779=CARTESIAN_POINT('Ctrl Pts',(57.8660665996852,-0.787641354648353,
-7.31026028219656));
#34780=CARTESIAN_POINT('Ctrl Pts',(58.0645782041271,5.71316809273326,-4.6281740072287));
#34781=CARTESIAN_POINT('Ctrl Pts',(58.2630898085693,6.98362156225626,2.30043872645768));
#34782=CARTESIAN_POINT('Ctrl Pts',(58.4285161456044,2.71657121158352,6.29637487350503));
#34783=CARTESIAN_POINT('Ctrl Pts',(58.5608572152325,-1.56235319508776,6.28023825009631));
#34784=CARTESIAN_POINT('Ctrl Pts',(58.6601130174535,-4.38640864661985,4.78363390655549));
#34785=CARTESIAN_POINT('Ctrl Pts',(58.7481524184562,-5.92552534696238,2.40288525575302));
#34786=CARTESIAN_POINT('Ctrl Pts',(58.8031065520518,-6.22151982471558,0.68137012316749));
#34787=CARTESIAN_POINT('Ctrl Pts',(58.8249754182404,-6.22479259784097,-0.00228417281318501));
#34788=CARTESIAN_POINT('Ctrl Pts',(57.8214645817597,-6.22441924678459,-0.00707629521854609));
#34789=CARTESIAN_POINT('Ctrl Pts',(57.8313117391515,-6.22705934464582,-0.314015706705484));
#34790=CARTESIAN_POINT('Ctrl Pts',(57.9073294313574,-6.06711261063953,-2.68001408884272));
#34791=CARTESIAN_POINT('Ctrl Pts',(58.0164323909703,-3.73549514279114,-5.75066706856635));
#34792=CARTESIAN_POINT('Ctrl Pts',(58.1487734605983,0.485355182835179,-6.45343089609464));
#34793=CARTESIAN_POINT('Ctrl Pts',(58.2480292628194,3.52065721958024,-5.45240377350268));
#34794=CARTESIAN_POINT('Ctrl Pts',(58.3472850650405,5.68201536485552,-3.09790919455678));
#34795=CARTESIAN_POINT('Ctrl Pts',(58.4796261346685,6.77836393432703,1.03820906811895));
#34796=CARTESIAN_POINT('Ctrl Pts',(58.6450524717037,3.98971935895797,6.17617421190118));
#34797=CARTESIAN_POINT('Ctrl Pts',(58.8435640761457,-3.03513575029629,6.69688250414221));
#34798=CARTESIAN_POINT('Ctrl Pts',(58.9857014461645,-6.06892784062922,2.67815832873045));
#34799=CARTESIAN_POINT('Ctrl Pts',(59.0616682813691,-6.22684436717526,0.310466242737264));
#34800=CARTESIAN_POINT('Ctrl Pts',(59.0714645817597,-6.22408309271093,0.00477558807787732));
#34801=CARTESIAN_POINT('Origin',(28.1999754182402,0.,0.));
#34802=CARTESIAN_POINT('',(56.3249754182404,-6.21925,3.42083457460389E-13));
#34803=CARTESIAN_POINT('',(56.5714645817597,-6.21881043026408,5.47690459495173E-5));
#34804=CARTESIAN_POINT('',(28.1999754182402,-6.21925,5.68729293530136E-12));
#34805=CARTESIAN_POINT('Ctrl Pts',(56.3249754182404,-6.21925,3.42083457460389E-13));
#34806=CARTESIAN_POINT('Ctrl Pts',(56.3837751697141,-6.2192500000001,-1.83816020915713));
#34807=CARTESIAN_POINT('Ctrl Pts',(56.4425749211878,-5.35502977485032,-3.65808141345929));
#34808=CARTESIAN_POINT('Ctrl Pts',(56.5013746726615,-3.9304971217585,-4.81977830800838));
#34809=CARTESIAN_POINT('Ctrl Pts',(56.5601744241352,-2.50596446866667,-5.98147520255747));
#34810=CARTESIAN_POINT('Ctrl Pts',(56.6189741756089,-0.549389021418706,
-6.46189408921057));
#34811=CARTESIAN_POINT('Ctrl Pts',(56.6777739270826,1.2511886986692,-6.09209302315899));
#34812=CARTESIAN_POINT('Ctrl Pts',(56.7365736785563,3.0517664187571,-5.72229195710742));
#34813=CARTESIAN_POINT('Ctrl Pts',(56.79537343003,4.66061422075239,-4.509609584249));
#34814=CARTESIAN_POINT('Ctrl Pts',(56.8541731815037,5.51197192302737,-2.88049233331005));
#34815=CARTESIAN_POINT('Ctrl Pts',(56.9129729329774,6.36332962530235,-1.2513750823711));
#34816=CARTESIAN_POINT('Ctrl Pts',(56.9717726844511,6.44030216377277,0.76184746264175));
#34817=CARTESIAN_POINT('Ctrl Pts',(57.0305724359248,5.71582172177419,2.45121451680475));
#34818=CARTESIAN_POINT('Ctrl Pts',(57.0893721873985,4.99134127977561,4.14058157096775));
#34819=CARTESIAN_POINT('Ctrl Pts',(57.1481719388721,3.47978506146401,5.47256790209511));
#34820=CARTESIAN_POINT('Ctrl Pts',(57.2069716903459,1.71270012775581,5.97877318811186));
#34821=CARTESIAN_POINT('Ctrl Pts',(57.2657714418196,-0.0543848059523969,
6.4849784741286));
#34822=CARTESIAN_POINT('Ctrl Pts',(57.3245711932932,-2.04193092337509,6.15535714814294));
#34823=CARTESIAN_POINT('Ctrl Pts',(57.3833709447669,-3.55100669662512,5.1058223630502));
#34824=CARTESIAN_POINT('Ctrl Pts',(57.4421706962406,-5.06008246987515,4.05628757795746));
#34825=CARTESIAN_POINT('Ctrl Pts',(57.5009704477143,-6.06074051980865,2.30766719190168));
#34826=CARTESIAN_POINT('Ctrl Pts',(57.559770199188,-6.2010939374368,0.474873184739413));
#34827=CARTESIAN_POINT('Ctrl Pts',(57.5648386055388,-6.21319208641583,0.316890462827627));
#34828=CARTESIAN_POINT('Ctrl Pts',(57.5699070118896,-6.21924999999998,0.158445276457149));
#34829=CARTESIAN_POINT('Ctrl Pts',(57.5749754182404,-6.21925,6.52939738037828E-13));
#34830=CARTESIAN_POINT('Ctrl Pts',(56.5714645817596,-6.20690476956114,0.00153817820988812));
#34831=CARTESIAN_POINT('Ctrl Pts',(56.6009551969339,-6.20849907782506,-0.923070451156225));
#34832=CARTESIAN_POINT('Ctrl Pts',(56.6635310795152,-5.79712602908302,-2.88516041489965));
#34833=CARTESIAN_POINT('Ctrl Pts',(56.7591922295036,-3.7946488264813,-5.24242122190289));
#34834=CARTESIAN_POINT('Ctrl Pts',(56.8584480317246,-0.830163910262025,
-6.43696838963711));
#34835=CARTESIAN_POINT('Ctrl Pts',(56.9577038339457,2.34039522251466,-6.03364650825719));
#34836=CARTESIAN_POINT('Ctrl Pts',(57.0900449035737,5.84744533060766,-3.58210535870519));
#34837=CARTESIAN_POINT('Ctrl Pts',(57.2554712406089,7.03376829111499,2.14221662907907));
#34838=CARTESIAN_POINT('Ctrl Pts',(57.4539828450509,2.00425491144597,7.07412514357485));
#34839=CARTESIAN_POINT('Ctrl Pts',(57.6426472921013,-4.51444270971877,5.59898313484983));
#34840=CARTESIAN_POINT('Ctrl Pts',(57.7651412043375,-6.20931852051886,1.74854348732337));
#34841=CARTESIAN_POINT('Ctrl Pts',(57.8214645817597,-6.22441924678459,-0.00707629521854609));
#34842=CARTESIAN_POINT('Origin',(28.1999754182402,0.,0.));
#34843=CARTESIAN_POINT('',(55.0749754182404,-6.22846436199193,-0.00261261932939155));
#34844=CARTESIAN_POINT('',(55.3214645817597,-6.21925,8.65253181115805E-14));
#34845=CARTESIAN_POINT('',(28.1999754182402,-6.21925,5.68729293530136E-12));
#34846=CARTESIAN_POINT('Ctrl Pts',(55.0749754182404,-6.22846436199193,-0.00261261932939051));
#34847=CARTESIAN_POINT('Ctrl Pts',(55.0789516579921,-6.22911653311281,-0.126462013579355));
#34848=CARTESIAN_POINT('Ctrl Pts',(55.1490984325579,-6.17099271056379,-2.31070670859694));
#34849=CARTESIAN_POINT('Ctrl Pts',(55.2854157419376,-3.61044798336259,-6.4050721819856));
#34850=CARTESIAN_POINT('Ctrl Pts',(55.4839273463797,3.43301069967906,-6.50210934965618));
#34851=CARTESIAN_POINT('Ctrl Pts',(55.6493536834148,6.66127426453652,-1.62834912347856));
#34852=CARTESIAN_POINT('Ctrl Pts',(55.7816947530429,5.93168364981801,2.58794688172988));
#34853=CARTESIAN_POINT('Ctrl Pts',(55.880950555264,3.98501993711935,5.12282639446718));
#34854=CARTESIAN_POINT('Ctrl Pts',(55.980206357485,1.04914210494851,6.38605048741379));
#34855=CARTESIAN_POINT('Ctrl Pts',(56.1125474271131,-3.21706142470918,6.05595669444211));
#34856=CARTESIAN_POINT('Ctrl Pts',(56.2274704473648,-5.94711148533298,3.04922222251432));
#34857=CARTESIAN_POINT('Ctrl Pts',(56.3093082002096,-6.22328552490555,0.497795406618084));
#34858=CARTESIAN_POINT('Ctrl Pts',(56.3249754182404,-6.21872822153172,0.00816645970560553));
#34859=CARTESIAN_POINT('Ctrl Pts',(55.3214645817597,-6.21925,8.65253181115805E-14));
#34860=CARTESIAN_POINT('Ctrl Pts',(55.3802643332334,-6.21925000000003,-1.8381602091575));
#34861=CARTESIAN_POINT('Ctrl Pts',(55.4390640847071,-5.35502977485006,-3.65808141345974));
#34862=CARTESIAN_POINT('Ctrl Pts',(55.4978638361808,-3.93049712175803,-4.81977830800877));
#34863=CARTESIAN_POINT('Ctrl Pts',(55.5566635876545,-2.505964468666,-5.9814752025578));
#34864=CARTESIAN_POINT('Ctrl Pts',(55.6154633391282,-0.549389021417821,
-6.46189408921067));
#34865=CARTESIAN_POINT('Ctrl Pts',(55.6742630906019,1.25118869867014,-6.0920930231588));
#34866=CARTESIAN_POINT('Ctrl Pts',(55.7330628420756,3.0517664187581,-5.72229195710693));
#34867=CARTESIAN_POINT('Ctrl Pts',(55.7918625935493,4.66061422075329,-4.50960958424812));
#34868=CARTESIAN_POINT('Ctrl Pts',(55.850662345023,5.51197192302798,-2.88049233330888));
#34869=CARTESIAN_POINT('Ctrl Pts',(55.9094620964967,6.36332962530267,-1.25137508236965));
#34870=CARTESIAN_POINT('Ctrl Pts',(55.9682618479704,6.44030216377261,0.761847462643371));
#34871=CARTESIAN_POINT('Ctrl Pts',(56.0270615994441,5.71582172177353,2.45121451680629));
#34872=CARTESIAN_POINT('Ctrl Pts',(56.0858613509178,4.99134127977445,4.1405815709692));
#34873=CARTESIAN_POINT('Ctrl Pts',(56.1446611023915,3.47978506146235,5.47256790209621));
#34874=CARTESIAN_POINT('Ctrl Pts',(56.2034608538652,1.71270012775386,5.97877318811242));
#34875=CARTESIAN_POINT('Ctrl Pts',(56.2622606053389,-0.0543848059546201,
6.48497847412862));
#34876=CARTESIAN_POINT('Ctrl Pts',(56.3210603568126,-2.04193092337735,6.15535714814223));
#34877=CARTESIAN_POINT('Ctrl Pts',(56.3798601082863,-3.55100669662707,5.10582236304884));
#34878=CARTESIAN_POINT('Ctrl Pts',(56.43865985976,-5.0600824698768,4.05628757795546));
#34879=CARTESIAN_POINT('Ctrl Pts',(56.4974596112337,-6.06074051980966,2.30766719189914));
#34880=CARTESIAN_POINT('Ctrl Pts',(56.5562593627074,-6.20109393743701,0.474873184736691));
#34881=CARTESIAN_POINT('Ctrl Pts',(56.5613277690582,-6.21319208641591,0.316890462825663));
#34882=CARTESIAN_POINT('Ctrl Pts',(56.5663961754089,-6.21925,0.15844527645595));
#34883=CARTESIAN_POINT('Ctrl Pts',(56.5714645817597,-6.21925,2.20619882313981E-13));
#34884=CARTESIAN_POINT('Origin',(28.1999754182402,0.,0.));
#34885=CARTESIAN_POINT('',(53.8249754182404,-6.2138011505806,-0.0039455443126054));
#34886=CARTESIAN_POINT('',(54.0714645817597,-6.2215550358857,-0.000870493656277005));
#34887=CARTESIAN_POINT('',(28.1999754182402,-6.21925,5.68729293530136E-12));
#34888=CARTESIAN_POINT('Ctrl Pts',(53.8249754182404,-6.2138011505806,-0.00394554431260567));
#34889=CARTESIAN_POINT('Ctrl Pts',(53.8485951157745,-6.21836794550842,-0.744086608287605));
#34890=CARTESIAN_POINT('Ctrl Pts',(53.9383853481227,-5.75208740079896,-3.55221171660335));
#34891=CARTESIAN_POINT('Ctrl Pts',(54.094346115285,-1.57464063360658,-7.18216508679608));
#34892=CARTESIAN_POINT('Ctrl Pts',(54.2597724523201,4.03688294466771,-5.54325462037972));
#34893=CARTESIAN_POINT('Ctrl Pts',(54.3921135219481,6.20102619469151,-1.85192173617664));
#34894=CARTESIAN_POINT('Ctrl Pts',(54.4913693241692,6.35029591436066,1.34069980500598));
#34895=CARTESIAN_POINT('Ctrl Pts',(54.5906251263902,4.92321156794364,4.2005151876216));
#34896=CARTESIAN_POINT('Ctrl Pts',(54.7229661960184,1.45161424482283,6.70200804084397));
#34897=CARTESIAN_POINT('Ctrl Pts',(54.8844162933016,-4.20421056897935,5.95119407725046));
#34898=CARTESIAN_POINT('Ctrl Pts',(55.0127811231781,-6.21826343708397,1.93457584269618));
#34899=CARTESIAN_POINT('Ctrl Pts',(55.0749754182404,-6.22846436199193,-0.00261261932939051));
#34900=CARTESIAN_POINT('Ctrl Pts',(54.0714645817597,-6.2215550358857,-0.000870493656276667));
#34901=CARTESIAN_POINT('Ctrl Pts',(54.0740715776848,-6.22167540488534,-0.0821163961368401));
#34902=CARTESIAN_POINT('Ctrl Pts',(54.109763841017,-6.20077041387944,-1.1943670518483));
#34903=CARTESIAN_POINT('Ctrl Pts',(54.1785413717561,-5.55877673210131,-3.31396156085478));
#34904=CARTESIAN_POINT('Ctrl Pts',(54.3108824413843,-2.55663608376213,-6.36299517762788));
#34905=CARTESIAN_POINT('Ctrl Pts',(54.4763087784192,3.28536884845591,-6.57794344674629));
#34906=CARTESIAN_POINT('Ctrl Pts',(54.6748203828615,7.30932326741656,-0.796289940546589));
#34907=CARTESIAN_POINT('Ctrl Pts',(54.8733319873035,4.63493030483003,5.70768826815035));
#34908=CARTESIAN_POINT('Ctrl Pts',(55.0718435917456,-2.29217444186588,6.98633843920073));
#34909=CARTESIAN_POINT('Ctrl Pts',(55.2212211232311,-5.90500183263401,3.13752701480774));
#34910=CARTESIAN_POINT('Ctrl Pts',(55.3044281199024,-6.22455833697474,0.535573970350642));
#34911=CARTESIAN_POINT('Ctrl Pts',(55.3214645817597,-6.22177129455467,0.00223847925715545));
#34912=CARTESIAN_POINT('Origin',(28.1999754182402,0.,0.));
#34913=CARTESIAN_POINT('',(52.5749754182404,-6.21194719993059,0.00357180041802368));
#34914=CARTESIAN_POINT('',(52.8214645817597,-6.21925,8.34792304726939E-14));
#34915=CARTESIAN_POINT('',(28.1999754182402,-6.21925,5.68729293530136E-12));
#34916=CARTESIAN_POINT('Ctrl Pts',(52.5749754182404,-6.21194719993059,0.00357180041802359));
#34917=CARTESIAN_POINT('Ctrl Pts',(52.618238573557,-6.20225771496113,-1.35305654649645));
#34918=CARTESIAN_POINT('Ctrl Pts',(52.7276722636877,-5.09844079489878,-4.79761319256802));
#34919=CARTESIAN_POINT('Ctrl Pts',(52.8701912212252,-0.494508874927136,
-6.83955822169301));
#34920=CARTESIAN_POINT('Ctrl Pts',(53.0025322908534,3.54103930044635,-5.41695307870284));
#34921=CARTESIAN_POINT('Ctrl Pts',(53.1017880930744,5.71572828749395,-3.07476573264209));
#34922=CARTESIAN_POINT('Ctrl Pts',(53.2010438952954,6.47158394013595,0.0306804489560287));
#34923=CARTESIAN_POINT('Ctrl Pts',(53.3333849649236,5.43455561682152,4.18206897874528));
#34924=CARTESIAN_POINT('Ctrl Pts',(53.4988113019586,0.511680132839369,7.33492821373557));
#34925=CARTESIAN_POINT('Ctrl Pts',(53.6737032088666,-5.1295763542309,4.74832352785551));
#34926=CARTESIAN_POINT('Ctrl Pts',(53.7824245809605,-6.20557407876551,1.32941708371486));
#34927=CARTESIAN_POINT('Ctrl Pts',(53.8249754182404,-6.2138011505806,-0.00394554431260567));
#34928=CARTESIAN_POINT('Ctrl Pts',(52.8214645817597,-6.21922526303958,-0.00141380809610282));
#34929=CARTESIAN_POINT('Ctrl Pts',(52.8437150354673,-6.22231424961983,-0.698568023883329));
#34930=CARTESIAN_POINT('Ctrl Pts',(52.9321360239888,-5.77659188785169,-3.46761533849687));
#34931=CARTESIAN_POINT('Ctrl Pts',(53.0867275473246,-1.73635698912002,-7.14479200994201));
#34932=CARTESIAN_POINT('Ctrl Pts',(53.2852391517666,5.06891690010915,-5.32600842627953));
#34933=CARTESIAN_POINT('Ctrl Pts',(53.4837507562088,7.22419817707089,1.36793457278422));
#34934=CARTESIAN_POINT('Ctrl Pts',(53.6822623606508,2.75856009795156,6.81566831976048));
#34935=CARTESIAN_POINT('Ctrl Pts',(53.847688697686,-3.04851381910718,6.14252872927938));
#34936=CARTESIAN_POINT('Ctrl Pts',(53.9774227713888,-5.74765690702425,2.93163669228894));
#34937=CARTESIAN_POINT('Ctrl Pts',(54.0409863102778,-6.22014780735358,0.948971678600679));
#34938=CARTESIAN_POINT('Ctrl Pts',(54.0714645817597,-6.2215550358857,-0.000870493656276667));
#34939=CARTESIAN_POINT('Origin',(28.1999754182402,0.,0.));
#34940=CARTESIAN_POINT('',(51.3249754182404,-6.22918278048295,0.000765166614752994));
#34941=CARTESIAN_POINT('',(51.5714645817597,-6.21798365229328,8.59752551505447E-5));
#34942=CARTESIAN_POINT('',(28.1999754182402,-6.21925,5.68729293530136E-12));
#34943=CARTESIAN_POINT('Ctrl Pts',(51.3249754182404,-6.22918278048295,0.00076516661475276));
#34944=CARTESIAN_POINT('Ctrl Pts',(51.3878820313394,-6.22114725490248,-1.95451838237354));
#34945=CARTESIAN_POINT('Ctrl Pts',(51.4838739118454,-4.69363132187248,-4.94233563448507));
#34946=CARTESIAN_POINT('Ctrl Pts',(51.6129510597586,-0.791714381456252,
-6.42304665422641));
#34947=CARTESIAN_POINT('Ctrl Pts',(51.7122068619796,2.38108318749985,-6.03772945910084));
#34948=CARTESIAN_POINT('Ctrl Pts',(51.8114626642006,4.96281693597846,-4.15364755897021));
#34949=CARTESIAN_POINT('Ctrl Pts',(51.9438037338288,6.85024388311463,-0.313455638265433));
#34950=CARTESIAN_POINT('Ctrl Pts',(52.1092300708638,5.12514934704392,5.27217532234014));
#34951=CARTESIAN_POINT('Ctrl Pts',(52.307741675306,-1.66057365242597,7.16259585917574));
#34952=CARTESIAN_POINT('Ctrl Pts',(52.4629901244314,-5.77184773115307,3.5095666463159));
#34953=CARTESIAN_POINT('Ctrl Pts',(52.5520680387429,-6.21707767891914,0.721892046649002));
#34954=CARTESIAN_POINT('Ctrl Pts',(52.5749754182404,-6.21194719993059,0.00357180041802359));
#34955=CARTESIAN_POINT('Ctrl Pts',(51.5714645817597,-6.21925,3.77650582544623E-14));
#34956=CARTESIAN_POINT('Ctrl Pts',(51.6302643332334,-6.21925000000001,-1.83816020915746));
#34957=CARTESIAN_POINT('Ctrl Pts',(51.6890640847071,-5.35502977485011,-3.65808141345961));
#34958=CARTESIAN_POINT('Ctrl Pts',(51.7478638361808,-3.93049712175819,-4.81977830800863));
#34959=CARTESIAN_POINT('Ctrl Pts',(51.8066635876545,-2.50596446866627,-5.98147520255765));
#34960=CARTESIAN_POINT('Ctrl Pts',(51.8654633391282,-0.549389021418235,
-6.46189408921061));
#34961=CARTESIAN_POINT('Ctrl Pts',(51.9242630906019,1.25118869866967,-6.0920930231589));
#34962=CARTESIAN_POINT('Ctrl Pts',(51.9830628420756,3.05176641875757,-5.72229195710718));
#34963=CARTESIAN_POINT('Ctrl Pts',(52.0418625935493,4.66061422075278,-4.5096095842486));
#34964=CARTESIAN_POINT('Ctrl Pts',(52.100662345023,5.51197192302763,-2.88049233330955));
#34965=CARTESIAN_POINT('Ctrl Pts',(52.1594620964967,6.36332962530248,-1.25137508237049));
#34966=CARTESIAN_POINT('Ctrl Pts',(52.2182618479704,6.4403021637727,0.761847462642404));
#34967=CARTESIAN_POINT('Ctrl Pts',(52.2770615994441,5.71582172177393,2.45121451680536));
#34968=CARTESIAN_POINT('Ctrl Pts',(52.3358613509178,4.99134127977516,4.14058157096831));
#34969=CARTESIAN_POINT('Ctrl Pts',(52.3946611023915,3.47978506146339,5.47256790209552));
#34970=CARTESIAN_POINT('Ctrl Pts',(52.4534608538652,1.71270012775509,5.97877318811206));
#34971=CARTESIAN_POINT('Ctrl Pts',(52.5122606053389,-0.0543848059532034,
6.48497847412861));
#34972=CARTESIAN_POINT('Ctrl Pts',(52.5710603568126,-2.0419309233759,6.15535714814268));
#34973=CARTESIAN_POINT('Ctrl Pts',(52.6298601082863,-3.55100669662581,5.10582236304972));
#34974=CARTESIAN_POINT('Ctrl Pts',(52.68865985976,-5.06008246987572,4.05628757795677));
#34975=CARTESIAN_POINT('Ctrl Pts',(52.7474596112337,-6.06074051980899,2.30766719190081));
#34976=CARTESIAN_POINT('Ctrl Pts',(52.8062593627074,-6.20109393743687,0.474873184738493));
#34977=CARTESIAN_POINT('Ctrl Pts',(52.8113277690581,-6.21319208641587,0.316890462826823));
#34978=CARTESIAN_POINT('Ctrl Pts',(52.8163961754089,-6.21925,0.158445276456461));
#34979=CARTESIAN_POINT('Ctrl Pts',(52.8214645817597,-6.21925,8.34787642693416E-14));
#34980=CARTESIAN_POINT('Origin',(28.1999754182402,0.,0.));
#34981=CARTESIAN_POINT('',(50.0749754182403,-6.21439911675028,-0.00289789719525526));
#34982=CARTESIAN_POINT('',(50.3214645817597,-6.22838628080824,0.00457472256878852));
#34983=CARTESIAN_POINT('',(28.1999754182402,-6.21925,5.68729293530136E-12));
#34984=CARTESIAN_POINT('Ctrl Pts',(50.0749754182403,-6.21439911675028,-0.00289789719525507));
#34985=CARTESIAN_POINT('Ctrl Pts',(50.0913549543078,-6.2190407860767,-0.515297532616419));
#34986=CARTESIAN_POINT('Ctrl Pts',(50.1408197577822,-6.04526190938845,-2.06095057890313));
#34987=CARTESIAN_POINT('Ctrl Pts',(50.2233698286639,-4.75046670097809,-4.39492959068425));
#34988=CARTESIAN_POINT('Ctrl Pts',(50.3226256308848,-2.07837204216358,-6.14850419382157));
#34989=CARTESIAN_POINT('Ctrl Pts',(50.4218814331059,1.10964349084127,-6.37581612873264));
#34990=CARTESIAN_POINT('Ctrl Pts',(50.554222502734,5.02991597370948,-4.66090559792109));
#34991=CARTESIAN_POINT('Ctrl Pts',(50.719648839769,7.31752721429885,0.718876851061941));
#34992=CARTESIAN_POINT('Ctrl Pts',(50.9181604442113,3.35474386460336,6.54262775189899));
#34993=CARTESIAN_POINT('Ctrl Pts',(51.1166720486532,-3.6754491338023,6.36799481484125));
#34994=CARTESIAN_POINT('Ctrl Pts',(51.2522770399964,-6.18160088298851,2.26024312233628));
#34995=CARTESIAN_POINT('Ctrl Pts',(51.3217114965254,-6.22959970527259,0.102215429474412));
#34996=CARTESIAN_POINT('Ctrl Pts',(51.3249754182404,-6.22918278048295,0.00076516661475276));
#34997=CARTESIAN_POINT('Ctrl Pts',(50.3214645817597,-6.22838628080824,0.00457472256878885));
#34998=CARTESIAN_POINT('Ctrl Pts',(50.3830019510321,-6.21821227336961,-1.9098165579918));
#34999=CARTESIAN_POINT('Ctrl Pts',(50.5107098551187,-4.24352685123475,-5.90977734476775));
#35000=CARTESIAN_POINT('Ctrl Pts',(50.7045882940192,2.55369426009361,-6.89484807105841));
#35001=CARTESIAN_POINT('Ctrl Pts',(50.9030998984613,7.1802970231816,-1.58313711278791));
#35002=CARTESIAN_POINT('Ctrl Pts',(51.0685262354964,5.54802698009573,4.03032161538502));
#35003=CARTESIAN_POINT('Ctrl Pts',(51.2008673051245,1.8592571864357,6.19883075255818));
#35004=CARTESIAN_POINT('Ctrl Pts',(51.3001231073455,-1.33318551163412,6.35187771912034));
#35005=CARTESIAN_POINT('Ctrl Pts',(51.3993789095666,-4.19468734797827,4.92817796319135));
#35006=CARTESIAN_POINT('Ctrl Pts',(51.4898260677046,-5.90711317747617,2.55757447662341));
#35007=CARTESIAN_POINT('Ctrl Pts',(51.5471879584357,-6.21271273978697,0.761507326426199));
#35008=CARTESIAN_POINT('Ctrl Pts',(51.5714645817597,-6.20863502281416,0.000720675188000328));
#35009=CARTESIAN_POINT('Origin',(28.1999754182402,0.,0.));
#35010=CARTESIAN_POINT('',(48.8249754182404,-6.2166083149304,-0.000591004908469454));
#35011=CARTESIAN_POINT('',(49.0714645817597,-6.21899721478014,-0.005340755338481));
#35012=CARTESIAN_POINT('',(28.1999754182402,-6.21925,5.68729293530136E-12));
#35013=CARTESIAN_POINT('Ctrl Pts',(48.8249754182404,-6.2166083149304,-0.000591004908469146));
#35014=CARTESIAN_POINT('Ctrl Pts',(48.8279131446832,-6.21638226706522,-0.092651946701776));
#35015=CARTESIAN_POINT('Ctrl Pts',(48.8639361385331,-6.18899652759796,-1.22134599105756));
#35016=CARTESIAN_POINT('Ctrl Pts',(48.93304439979,-5.55601616227824,-3.3547605833489));
#35017=CARTESIAN_POINT('Ctrl Pts',(49.0323002020111,-3.26771921629748,-5.58608549053932));
#35018=CARTESIAN_POINT('Ctrl Pts',(49.1646412716392,0.833484420250366,-6.80657031231661));
#35019=CARTESIAN_POINT('Ctrl Pts',(49.3300676086743,6.05314692292063,-4.17401494828823));
#35020=CARTESIAN_POINT('Ctrl Pts',(49.5285792131164,6.78529949630181,2.83195957642392));
#35021=CARTESIAN_POINT('Ctrl Pts',(49.7270908175584,1.30290129179695,7.23620981735928));
#35022=CARTESIAN_POINT('Ctrl Pts',(49.9092228859333,-4.82912622707473,5.19479701430948));
#35023=CARTESIAN_POINT('Ctrl Pts',(50.0251844194937,-6.20028923288899,1.55470968704536));
#35024=CARTESIAN_POINT('Ctrl Pts',(50.0749754182403,-6.21439911675028,-0.00289789719525507));
#35025=CARTESIAN_POINT('Ctrl Pts',(49.0714645817597,-6.21899721478014,-0.00534075533848107));
#35026=CARTESIAN_POINT('Ctrl Pts',(49.0864748740005,-6.22356854582095,-0.474708533744452));
#35027=CARTESIAN_POINT('Ctrl Pts',(49.1676557010554,-5.96234790315834,-3.00834188896351));
#35028=CARTESIAN_POINT('Ctrl Pts',(49.3150070629244,-2.4997580926362,-6.91458558232614));
#35029=CARTESIAN_POINT('Ctrl Pts',(49.5135186673665,4.46249608146065,-5.84372459840002));
#35030=CARTESIAN_POINT('Ctrl Pts',(49.6789450044016,6.838968356171,-0.502600754676708));
#35031=CARTESIAN_POINT('Ctrl Pts',(49.8112860740297,5.42113886922714,3.53462775193207));
#35032=CARTESIAN_POINT('Ctrl Pts',(49.9105418762507,3.08152614660459,5.71208637669992));
#35033=CARTESIAN_POINT('Ctrl Pts',(50.0097976784718,-0.0230235705233395,
6.47161571011243));
#35034=CARTESIAN_POINT('Ctrl Pts',(50.1421387480999,-4.17563615511025,5.43949982952901));
#35035=CARTESIAN_POINT('Ctrl Pts',(50.2460277158625,-6.15931160573698,2.35024230288155));
#35036=CARTESIAN_POINT('Ctrl Pts',(50.3168314162181,-6.22915228464041,0.148709771223719));
#35037=CARTESIAN_POINT('Ctrl Pts',(50.3214645817597,-6.22838628080824,0.00457472256878885));
#35038=CARTESIAN_POINT('Origin',(28.1999754182402,0.,0.));
#35039=CARTESIAN_POINT('',(47.5749754182404,-6.21925,3.75611000635878E-13));
#35040=CARTESIAN_POINT('',(47.8214645817597,-6.21071229255457,0.000741149837754085));
#35041=CARTESIAN_POINT('',(28.1999754182402,-6.21925,5.68729293530136E-12));
#35042=CARTESIAN_POINT('Ctrl Pts',(47.5749754182404,-6.21933081007893,0.00292931974371469));
#35043=CARTESIAN_POINT('Ctrl Pts',(47.5975566024657,-6.2170155757593,-0.701663893040958));
#35044=CARTESIAN_POINT('Ctrl Pts',(47.653223054098,-5.91532415731919,-2.44161599281549));
#35045=CARTESIAN_POINT('Ctrl Pts',(47.7750600405443,-3.756680423898,-5.73684999699412));
#35046=CARTESIAN_POINT('Ctrl Pts',(47.9404863775796,1.92929451774911,-7.09512587082007));
#35047=CARTESIAN_POINT('Ctrl Pts',(48.1389979820215,7.01051831056036,-2.21651016562319));
#35048=CARTESIAN_POINT('Ctrl Pts',(48.3375095864638,5.66576857146238,4.68608053618823));
#35049=CARTESIAN_POINT('Ctrl Pts',(48.5360211909057,-0.875229719861018,
7.30047679240671));
#35050=CARTESIAN_POINT('Ctrl Pts',(48.6985098014981,-5.55095834388157,3.96734594113617));
#35051=CARTESIAN_POINT('Ctrl Pts',(48.7948278772762,-6.21892806369116,0.94415693805931));
#35052=CARTESIAN_POINT('Ctrl Pts',(48.8249754182404,-6.2166083149304,-0.000591004908469146));
#35053=CARTESIAN_POINT('Ctrl Pts',(47.8214645817597,-6.21071229255457,0.000741149837754154));
#35054=CARTESIAN_POINT('Ctrl Pts',(47.856118331783,-6.20949620099682,-1.08651601273864));
#35055=CARTESIAN_POINT('Ctrl Pts',(47.9569426166203,-5.41832110916315,-4.25151146531121));
#35056=CARTESIAN_POINT('Ctrl Pts',(48.1239374362717,-0.363362580539744,
-7.34376988297294));
#35057=CARTESIAN_POINT('Ctrl Pts',(48.2893637733068,4.89922005122494,-4.79809739219469));
#35058=CARTESIAN_POINT('Ctrl Pts',(48.4217048429349,6.42210544142411,-0.79931325736819));
#35059=CARTESIAN_POINT('Ctrl Pts',(48.5209606451559,6.04054241262091,2.37393797905852));
#35060=CARTESIAN_POINT('Ctrl Pts',(48.620216447377,4.1595164104518,4.95789907272788));
#35061=CARTESIAN_POINT('Ctrl Pts',(48.7525575170051,0.321560287482606,6.84986822331817));
#35062=CARTESIAN_POINT('Ctrl Pts',(48.9029735617993,-4.75909947860206,5.28731370912977));
#35063=CARTESIAN_POINT('Ctrl Pts',(49.0203043391865,-6.20341654511846,1.59442619216282));
#35064=CARTESIAN_POINT('Ctrl Pts',(49.0714645817597,-6.21899721478014,-0.00534075533848107));
#35065=CARTESIAN_POINT('Origin',(28.1999754182402,0.,0.));
#35066=CARTESIAN_POINT('',(46.3249754182404,-6.21925,3.29897242091433E-13));
#35067=CARTESIAN_POINT('',(46.5714645817596,-6.22210936345043,0.0051709891022092));
#35068=CARTESIAN_POINT('',(28.1999754182402,-6.21925,5.68729293530136E-12));
#35069=CARTESIAN_POINT('Ctrl Pts',(46.3249754182404,-6.21925,3.29897242091433E-13));
#35070=CARTESIAN_POINT('Ctrl Pts',(46.3837751697141,-6.2192500000001,-1.83816020915711));
#35071=CARTESIAN_POINT('Ctrl Pts',(46.4425749211878,-5.35502977485034,-3.65808141345925));
#35072=CARTESIAN_POINT('Ctrl Pts',(46.5013746726615,-3.93049712175856,-4.81977830800834));
#35073=CARTESIAN_POINT('Ctrl Pts',(46.5601744241352,-2.50596446866677,-5.98147520255743));
#35074=CARTESIAN_POINT('Ctrl Pts',(46.6189741756089,-0.549389021418848,
-6.46189408921054));
#35075=CARTESIAN_POINT('Ctrl Pts',(46.6777739270826,1.25118869866904,-6.09209302315903));
#35076=CARTESIAN_POINT('Ctrl Pts',(46.7365736785563,3.05176641875692,-5.72229195710751));
#35077=CARTESIAN_POINT('Ctrl Pts',(46.7953734300299,4.66061422075222,-4.50960958424917));
#35078=CARTESIAN_POINT('Ctrl Pts',(46.8541731815036,5.51197192302725,-2.88049233331027));
#35079=CARTESIAN_POINT('Ctrl Pts',(46.9129729329773,6.36332962530229,-1.25137508237138));
#35080=CARTESIAN_POINT('Ctrl Pts',(46.971772684451,6.4403021637728,0.761847462641424));
#35081=CARTESIAN_POINT('Ctrl Pts',(47.0305724359247,5.71582172177432,2.45121451680444));
#35082=CARTESIAN_POINT('Ctrl Pts',(47.0893721873984,4.99134127977585,4.14058157096745));
#35083=CARTESIAN_POINT('Ctrl Pts',(47.1481719388721,3.47978506146436,5.47256790209488));
#35084=CARTESIAN_POINT('Ctrl Pts',(47.2069716903458,1.71270012775622,5.97877318811174));
#35085=CARTESIAN_POINT('Ctrl Pts',(47.2657714418195,-0.0543848059519203,
6.4849784741286));
#35086=CARTESIAN_POINT('Ctrl Pts',(47.3245711932932,-2.04193092337461,6.15535714814309));
#35087=CARTESIAN_POINT('Ctrl Pts',(47.3833709447669,-3.5510066966247,5.1058223630505));
#35088=CARTESIAN_POINT('Ctrl Pts',(47.4421706962406,-5.06008246987479,4.0562875779579));
#35089=CARTESIAN_POINT('Ctrl Pts',(47.5009704477143,-6.06074051980843,2.30766719190224));
#35090=CARTESIAN_POINT('Ctrl Pts',(47.559770199188,-6.20109393743675,0.474873184740018));
#35091=CARTESIAN_POINT('Ctrl Pts',(47.5648386055388,-6.21319208641582,0.316890462827939));
#35092=CARTESIAN_POINT('Ctrl Pts',(47.5699070118896,-6.21924999999999,0.158445276457166));
#35093=CARTESIAN_POINT('Ctrl Pts',(47.5749754182404,-6.21925,3.75610948106313E-13));
#35094=CARTESIAN_POINT('Ctrl Pts',(46.5714645817596,-6.22210936345043,0.00517098910220969));
#35095=CARTESIAN_POINT('Ctrl Pts',(46.6257617895654,-6.20584908536478,-1.6905361365724));
#35096=CARTESIAN_POINT('Ctrl Pts',(46.7462295321853,-4.61113712656708,-5.47890052593373));
#35097=CARTESIAN_POINT('Ctrl Pts',(46.899782542212,0.645108111263187,-6.82700016259648));
#35098=CARTESIAN_POINT('Ctrl Pts',(47.0321236118402,4.38930599811985,-4.75566323860751));
#35099=CARTESIAN_POINT('Ctrl Pts',(47.1313794140611,6.14604086368536,-2.08564519249999));
#35100=CARTESIAN_POINT('Ctrl Pts',(47.2306352162823,6.37712454126565,1.10209916493979));
#35101=CARTESIAN_POINT('Ctrl Pts',(47.3629762859102,4.66685348261288,5.0243979009563));
#35102=CARTESIAN_POINT('Ctrl Pts',(47.5284026229454,-0.710218612843849,
7.31837263201097));
#35103=CARTESIAN_POINT('Ctrl Pts',(47.6922604773642,-5.52119639342655,4.05305379686667));
#35104=CARTESIAN_POINT('Ctrl Pts',(47.7899477969689,-6.21181829972221,0.98957641245848));
#35105=CARTESIAN_POINT('Ctrl Pts',(47.8214645817597,-6.21071229255457,0.000741149837754154));
#35106=CARTESIAN_POINT('Origin',(28.1999754182402,0.,0.));
#35107=CARTESIAN_POINT('',(45.0749754182404,-6.21854788291297,-0.000317205416753715));
#35108=CARTESIAN_POINT('',(45.3214645817596,-6.22620958835039,-0.00623427698102752));
#35109=CARTESIAN_POINT('',(28.1999754182402,-6.21925,5.68729293530136E-12));
#35110=CARTESIAN_POINT('Ctrl Pts',(45.0749754182404,-6.20821420870357,-0.00498579630805643));
#35111=CARTESIAN_POINT('Ctrl Pts',(45.1037582506235,-6.2119349975194,-0.906770203246303));
#35112=CARTESIAN_POINT('Ctrl Pts',(45.1987116178207,-5.6083688757905,-3.87600348080113));
#35113=CARTESIAN_POINT('Ctrl Pts',(45.3598355198321,-1.01618098913832,-7.2820093720296));
#35114=CARTESIAN_POINT('Ctrl Pts',(45.5583471242741,5.56543150817819,-4.80481596159418));
#35115=CARTESIAN_POINT('Ctrl Pts',(45.7568587287163,7.05223625244414,2.08061344288397));
#35116=CARTESIAN_POINT('Ctrl Pts',(45.9222850657513,2.91241425495877,6.20821543624437));
#35117=CARTESIAN_POINT('Ctrl Pts',(46.0546261353794,-1.3649168534335,6.32608425231493));
#35118=CARTESIAN_POINT('Ctrl Pts',(46.1538819376005,-4.23445444437469,4.9186512099969));
#35119=CARTESIAN_POINT('Ctrl Pts',(46.2439983652208,-5.88542304071439,2.5322667313354));
#35120=CARTESIAN_POINT('Ctrl Pts',(46.3010295254341,-6.22263107846942,0.746134257446151));
#35121=CARTESIAN_POINT('Ctrl Pts',(46.3249754182404,-6.22573560541529,-0.00204345304936147));
#35122=CARTESIAN_POINT('Ctrl Pts',(45.3214645817597,-6.22620958835039,-0.00623427698102683));
#35123=CARTESIAN_POINT('Ctrl Pts',(45.3292347125338,-6.22805343704289,-0.248224525845919));
#35124=CARTESIAN_POINT('Ctrl Pts',(45.403175378122,-6.10552815017325,-2.54852208963383));
#35125=CARTESIAN_POINT('Ctrl Pts',(45.5102013111172,-3.91374922444537,-5.63086695842329));
#35126=CARTESIAN_POINT('Ctrl Pts',(45.6425423807454,0.283023412847933,-6.46546500508306));
#35127=CARTESIAN_POINT('Ctrl Pts',(45.7417981829663,3.34818463267598,-5.55998145973536));
#35128=CARTESIAN_POINT('Ctrl Pts',(45.8410539851874,5.58221537749888,-3.27432610828378));
#35129=CARTESIAN_POINT('Ctrl Pts',(45.9733950548155,6.80755168564738,0.825430640665489));
#35130=CARTESIAN_POINT('Ctrl Pts',(46.1388213918506,4.18117380984599,6.04820419883911));
#35131=CARTESIAN_POINT('Ctrl Pts',(46.3373329962928,-2.82392956463494,6.78864538114884));
#35132=CARTESIAN_POINT('Ctrl Pts',(46.481547392929,-6.02823238238414,2.80958978582469));
#35133=CARTESIAN_POINT('Ctrl Pts',(46.5595912547514,-6.22566504534934,0.375976156200805));
#35134=CARTESIAN_POINT('Ctrl Pts',(46.5714645817596,-6.22210936345043,0.00517098910220969));
#35135=CARTESIAN_POINT('Origin',(28.1999754182402,0.,0.));
#35136=CARTESIAN_POINT('',(43.8249754182404,-6.21925,4.15231546436714E-13));
#35137=CARTESIAN_POINT('',(44.0714645817597,-6.21730219627848,9.77522333141482E-5));
#35138=CARTESIAN_POINT('',(28.1999754182402,-6.21925,5.68729293530136E-12));
#35139=CARTESIAN_POINT('Ctrl Pts',(43.8249754182404,-6.21925,5.91993262811754E-13));
#35140=CARTESIAN_POINT('Ctrl Pts',(43.8837751697141,-6.21925000000018,-1.83816020915688));
#35141=CARTESIAN_POINT('Ctrl Pts',(43.9425749211877,-5.35502977485047,-3.65808141345908));
#35142=CARTESIAN_POINT('Ctrl Pts',(44.0013746726614,-3.93049712175869,-4.81977830800823));
#35143=CARTESIAN_POINT('Ctrl Pts',(44.0601744241351,-2.50596446866692,-5.98147520255737));
#35144=CARTESIAN_POINT('Ctrl Pts',(44.1189741756088,-0.549389021418965,
-6.46189408921054));
#35145=CARTESIAN_POINT('Ctrl Pts',(44.1777739270825,1.25118869866895,-6.09209302315904));
#35146=CARTESIAN_POINT('Ctrl Pts',(44.2365736785562,3.05176641875687,-5.72229195710755));
#35147=CARTESIAN_POINT('Ctrl Pts',(44.2953734300299,4.6606142207522,-4.50960958424919));
#35148=CARTESIAN_POINT('Ctrl Pts',(44.3541731815036,5.51197192302725,-2.88049233331027));
#35149=CARTESIAN_POINT('Ctrl Pts',(44.4129729329773,6.3633296253023,-1.25137508237135));
#35150=CARTESIAN_POINT('Ctrl Pts',(44.471772684451,6.4403021637728,0.761847462641492));
#35151=CARTESIAN_POINT('Ctrl Pts',(44.5305724359247,5.71582172177429,2.45121451680452));
#35152=CARTESIAN_POINT('Ctrl Pts',(44.5893721873984,4.99134127977578,4.14058157096755));
#35153=CARTESIAN_POINT('Ctrl Pts',(44.6481719388721,3.47978506146424,5.47256790209497));
#35154=CARTESIAN_POINT('Ctrl Pts',(44.7069716903458,1.71270012775605,5.97877318811179));
#35155=CARTESIAN_POINT('Ctrl Pts',(44.7657714418195,-0.0543848059521362,
6.48497847412861));
#35156=CARTESIAN_POINT('Ctrl Pts',(44.8245711932932,-2.04193092337485,6.15535714814302));
#35157=CARTESIAN_POINT('Ctrl Pts',(44.8833709447669,-3.55100669662492,5.10582236305034));
#35158=CARTESIAN_POINT('Ctrl Pts',(44.9421706962406,-5.06008246987499,4.05628757795767));
#35159=CARTESIAN_POINT('Ctrl Pts',(45.0009704477143,-6.06074051980856,2.30766719190193));
#35160=CARTESIAN_POINT('Ctrl Pts',(45.059770199188,-6.20109393743678,0.474873184739662));
#35161=CARTESIAN_POINT('Ctrl Pts',(45.0648386055388,-6.21319208641583,0.316890462827671));
#35162=CARTESIAN_POINT('Ctrl Pts',(45.0699070118896,-6.21924999999999,0.158445276456986));
#35163=CARTESIAN_POINT('Ctrl Pts',(45.0749754182404,-6.21925,2.84183536076554E-13));
#35164=CARTESIAN_POINT('Ctrl Pts',(44.0714645817597,-6.20735719350781,0.000596850939321783));
#35165=CARTESIAN_POINT('Ctrl Pts',(44.0988781703163,-6.21014037266732,-0.858805783627428));
#35166=CARTESIAN_POINT('Ctrl Pts',(44.1593770262799,-5.84277927858636,-2.75472237638653));
#35167=CARTESIAN_POINT('Ctrl Pts',(44.2529611496505,-3.9569578199035,-5.12101794526032));
#35168=CARTESIAN_POINT('Ctrl Pts',(44.3522169518716,-1.03133493987818,-6.40781416778569));
#35169=CARTESIAN_POINT('Ctrl Pts',(44.4514727540926,2.15029947849091,-6.10397838601804));
#35170=CARTESIAN_POINT('Ctrl Pts',(44.5838138237208,5.73240126379457,-3.76346535073147));
#35171=CARTESIAN_POINT('Ctrl Pts',(44.7492401607558,7.09740355031088,1.92089856656498));
#35172=CARTESIAN_POINT('Ctrl Pts',(44.9477517651979,2.22480311159819,7.00789093890849));
#35173=CARTESIAN_POINT('Ctrl Pts',(45.1384932388659,-4.40913087075351,5.72362536591463));
#35174=CARTESIAN_POINT('Ctrl Pts',(45.2630641777198,-6.21235119757683,1.81256758339546));
#35175=CARTESIAN_POINT('Ctrl Pts',(45.3214645817597,-6.22620958835039,-0.00623427698102683));
#35176=CARTESIAN_POINT('Origin',(28.1999754182402,0.,0.));
#35177=CARTESIAN_POINT('',(42.5749754182404,-6.22934530309283,-0.00155873460105957));
#35178=CARTESIAN_POINT('',(42.8214645817597,-6.21925,3.36435123462946E-13));
#35179=CARTESIAN_POINT('',(28.1999754182402,-6.21925,5.68729293530136E-12));
#35180=CARTESIAN_POINT('Ctrl Pts',(42.5749754182404,-6.22934530309283,-0.00155873460105878));
#35181=CARTESIAN_POINT('Ctrl Pts',(42.5768746313744,-6.22952614868411,-0.0606917412216028));
#35182=CARTESIAN_POINT('Ctrl Pts',(42.6449443793225,-6.20328599844248,-2.17990023331552));
#35183=CARTESIAN_POINT('Ctrl Pts',(42.7791846620846,-3.80925655132213,-6.2888670540267));
#35184=CARTESIAN_POINT('Ctrl Pts',(42.9776962665266,3.22770883173084,-6.60642748817874));
#35185=CARTESIAN_POINT('Ctrl Pts',(43.1431226035619,6.60701429937979,-1.83615297377451));
#35186=CARTESIAN_POINT('Ctrl Pts',(43.2754636731898,6.00981779016149,2.40092276286268));
#35187=CARTESIAN_POINT('Ctrl Pts',(43.3747194754109,4.14349036564128,4.9955201688039));
#35188=CARTESIAN_POINT('Ctrl Pts',(43.473975277632,1.24861120530404,6.35006378252714));
#35189=CARTESIAN_POINT('Ctrl Pts',(43.6063163472601,-3.02583705454058,6.15373104828925));
#35190=CARTESIAN_POINT('Ctrl Pts',(43.7233163941295,-5.89972442142763,3.18119516786605));
#35191=CARTESIAN_POINT('Ctrl Pts',(43.807231173592,-6.22164619015469,0.56313307617446));
#35192=CARTESIAN_POINT('Ctrl Pts',(43.8249754182404,-6.21669210645943,0.0080881789777975));
#35193=CARTESIAN_POINT('Ctrl Pts',(42.8214645817597,-6.21925,3.36435123462946E-13));
#35194=CARTESIAN_POINT('Ctrl Pts',(42.8802643332334,-6.2192500000001,-1.83816020915713));
#35195=CARTESIAN_POINT('Ctrl Pts',(42.9390640847071,-5.35502977485032,-3.6580814134593));
#35196=CARTESIAN_POINT('Ctrl Pts',(42.9978638361808,-3.93049712175849,-4.81977830800839));
#35197=CARTESIAN_POINT('Ctrl Pts',(43.0566635876545,-2.50596446866667,-5.98147520255748));
#35198=CARTESIAN_POINT('Ctrl Pts',(43.1154633391282,-0.5493890214187,-6.46189408921057));
#35199=CARTESIAN_POINT('Ctrl Pts',(43.1742630906019,1.2511886986692,-6.09209302315899));
#35200=CARTESIAN_POINT('Ctrl Pts',(43.2330628420756,3.05176641875711,-5.72229195710742));
#35201=CARTESIAN_POINT('Ctrl Pts',(43.2918625935493,4.66061422075239,-4.509609584249));
#35202=CARTESIAN_POINT('Ctrl Pts',(43.350662345023,5.51197192302737,-2.88049233331005));
#35203=CARTESIAN_POINT('Ctrl Pts',(43.4094620964967,6.36332962530235,-1.25137508237109));
#35204=CARTESIAN_POINT('Ctrl Pts',(43.4682618479704,6.44030216377276,0.761847462641756));
#35205=CARTESIAN_POINT('Ctrl Pts',(43.5270615994441,5.71582172177419,2.45121451680476));
#35206=CARTESIAN_POINT('Ctrl Pts',(43.5858613509178,4.99134127977561,4.14058157096776));
#35207=CARTESIAN_POINT('Ctrl Pts',(43.6446611023915,3.47978506146401,5.47256790209512));
#35208=CARTESIAN_POINT('Ctrl Pts',(43.7034608538652,1.7127001277558,5.97877318811186));
#35209=CARTESIAN_POINT('Ctrl Pts',(43.7622606053389,-0.0543848059524024,
6.4849784741286));
#35210=CARTESIAN_POINT('Ctrl Pts',(43.8210603568125,-2.0419309233751,6.15535714814294));
#35211=CARTESIAN_POINT('Ctrl Pts',(43.8798601082863,-3.55100669662513,5.1058223630502));
#35212=CARTESIAN_POINT('Ctrl Pts',(43.93865985976,-5.06008246987515,4.05628757795746));
#35213=CARTESIAN_POINT('Ctrl Pts',(43.9974596112336,-6.06074051980865,2.30766719190168));
#35214=CARTESIAN_POINT('Ctrl Pts',(44.0562593627073,-6.2010939374368,0.474873184739407));
#35215=CARTESIAN_POINT('Ctrl Pts',(44.0613277690581,-6.21319208641584,0.316890462827504));
#35216=CARTESIAN_POINT('Ctrl Pts',(44.0663961754089,-6.21924999999999,0.158445276456907));
#35217=CARTESIAN_POINT('Ctrl Pts',(44.0714645817597,-6.21925,2.93767971290306E-13));
#35218=CARTESIAN_POINT('Origin',(28.1999754182402,0.,0.));
#35219=CARTESIAN_POINT('',(41.3249754182403,-6.21523911303322,-0.00450227194547106));
#35220=CARTESIAN_POINT('',(41.5714645817597,-6.22175358549805,-0.000179260700348682));
#35221=CARTESIAN_POINT('',(28.1999754182402,-6.21925,5.68729293530136E-12));
#35222=CARTESIAN_POINT('Ctrl Pts',(41.3249754182403,-6.21523911303322,-0.00450227194547133));
#35223=CARTESIAN_POINT('Ctrl Pts',(41.3465180891568,-6.22007772484495,-0.679164296726016));
#35224=CARTESIAN_POINT('Ctrl Pts',(41.4342312948873,-5.80641375796907,-3.42039969603429));
#35225=CARTESIAN_POINT('Ctrl Pts',(41.5881150354319,-1.7987828877996,-7.12933156625193));
#35226=CARTESIAN_POINT('Ctrl Pts',(41.753541372467,3.86131211317401,-5.66695371958917));
#35227=CARTESIAN_POINT('Ctrl Pts',(41.8858824420951,6.13999062787377,-2.04520294195858));
#35228=CARTESIAN_POINT('Ctrl Pts',(41.9851382443162,6.38916632461915,1.14117826979005));
#35229=CARTESIAN_POINT('Ctrl Pts',(42.0843940465372,5.05233903023813,4.04428118553917));
#35230=CARTESIAN_POINT('Ctrl Pts',(42.2167351161653,1.66078038279294,6.65326267446582));
#35231=CARTESIAN_POINT('Ctrl Pts',(42.3802622400663,-4.08881072896843,6.07255729926071));
#35232=CARTESIAN_POINT('Ctrl Pts',(42.5107040965604,-6.22322530267627,1.99956289956022));
#35233=CARTESIAN_POINT('Ctrl Pts',(42.5749754182404,-6.22934530309283,-0.00155873460105878));
#35234=CARTESIAN_POINT('Ctrl Pts',(41.5714645817596,-6.22175358549805,-0.000179260700348691));
#35235=CARTESIAN_POINT('Ctrl Pts',(41.5719945510671,-6.22175922636749,-0.0166938072709939));
#35236=CARTESIAN_POINT('Ctrl Pts',(41.6056097877816,-6.21775797837456,-1.06418559288761));
#35237=CARTESIAN_POINT('Ctrl Pts',(41.6723102919031,-5.65982942715753,-3.13825920530084));
#35238=CARTESIAN_POINT('Ctrl Pts',(41.8046513615312,-2.7546438300705,-6.2798115469148));
#35239=CARTESIAN_POINT('Ctrl Pts',(41.9700776985662,3.07776459442245,-6.67760088357463));
#35240=CARTESIAN_POINT('Ctrl Pts',(42.1685893030084,7.280801980269,-1.02479599000183));
#35241=CARTESIAN_POINT('Ctrl Pts',(42.3671009074504,4.81139734096477,5.55974279300492));
#35242=CARTESIAN_POINT('Ctrl Pts',(42.5656125118927,-2.0722681306563,7.05469299499727));
#35243=CARTESIAN_POINT('Ctrl Pts',(42.7170670699956,-5.85573779370101,3.26899088665945));
#35244=CARTESIAN_POINT('Ctrl Pts',(42.8023510932847,-6.22370194316221,0.600581950735336));
#35245=CARTESIAN_POINT('Ctrl Pts',(42.8214645817597,-6.22070394341143,0.00198527999243369));
#35246=CARTESIAN_POINT('Origin',(28.1999754182402,0.,0.));
#35247=CARTESIAN_POINT('',(40.0749754182403,-6.21056889989778,0.00266732454412204));
#35248=CARTESIAN_POINT('',(40.3214645817597,-6.21925,5.98531640916278E-13));
#35249=CARTESIAN_POINT('',(28.1999754182402,-6.21925,5.68729293530136E-12));
#35250=CARTESIAN_POINT('Ctrl Pts',(40.0749754182403,-6.21056889989778,0.00266732454412187));
#35251=CARTESIAN_POINT('Ctrl Pts',(40.1161615469393,-6.20290591724236,-1.28951842298143));
#35252=CARTESIAN_POINT('Ctrl Pts',(40.2235182104523,-5.18004941908787,-4.66744415132467));
#35253=CARTESIAN_POINT('Ctrl Pts',(40.3639601413723,-0.708451912413997,
-6.82071782022295));
#35254=CARTESIAN_POINT('Ctrl Pts',(40.4963012110003,3.3696668804336,-5.52518643116073));
#35255=CARTESIAN_POINT('Ctrl Pts',(40.5955570132214,5.6166365191778,-3.25224974110642));
#35256=CARTESIAN_POINT('Ctrl Pts',(40.6948128154424,6.46937068698724,-0.17199679800523));
#35257=CARTESIAN_POINT('Ctrl Pts',(40.8271538850705,5.56285463090548,4.00983092545351));
#35258=CARTESIAN_POINT('Ctrl Pts',(40.9925802221055,0.741127608027151,7.3153071246269));
#35259=CARTESIAN_POINT('Ctrl Pts',(41.1695491556312,-5.04628844301002,4.87802538828724));
#35260=CARTESIAN_POINT('Ctrl Pts',(41.2803475543428,-6.20521542979432,1.39312967144128));
#35261=CARTESIAN_POINT('Ctrl Pts',(41.3249754182403,-6.21523911303322,-0.00450227194547133));
#35262=CARTESIAN_POINT('Ctrl Pts',(40.3214645817597,-6.22018273820767,-0.00181530436698364));
#35263=CARTESIAN_POINT('Ctrl Pts',(40.3416380088496,-6.22324239534247,-0.63371717248096));
#35264=CARTESIAN_POINT('Ctrl Pts',(40.4279819707534,-5.829640410661,-3.3360972611883));
#35265=CARTESIAN_POINT('Ctrl Pts',(40.5804964674716,-1.95924956424283,-7.08691255794874));
#35266=CARTESIAN_POINT('Ctrl Pts',(40.7790080719135,4.89964311770096,-5.48213294404453));
#35267=CARTESIAN_POINT('Ctrl Pts',(40.9775196763558,7.26349285183276,1.1410328165251));
#35268=CARTESIAN_POINT('Ctrl Pts',(41.1760312807977,2.97064458683377,6.72593927996026));
#35269=CARTESIAN_POINT('Ctrl Pts',(41.3414576178329,-2.85466105015735,6.23498243654499));
#35270=CARTESIAN_POINT('Ctrl Pts',(41.4732687181535,-5.69783323613032,3.06016323492747));
#35271=CARTESIAN_POINT('Ctrl Pts',(41.5389092836601,-6.22140707451404,1.01428700936641));
#35272=CARTESIAN_POINT('Ctrl Pts',(41.5714645817596,-6.22175358549805,-0.000179260700348691));
#35273=CARTESIAN_POINT('Origin',(28.1999754182402,0.,0.));
#35274=CARTESIAN_POINT('',(38.8249754182403,-6.22814110134059,0.00214874350932149));
#35275=CARTESIAN_POINT('',(39.0714645817597,-6.21833151244906,-1.0638405337316E-5));
#35276=CARTESIAN_POINT('',(28.1999754182402,-6.21925,5.68729293530136E-12));
#35277=CARTESIAN_POINT('Ctrl Pts',(38.8249754182403,-6.22814110134059,0.00214874350932153));
#35278=CARTESIAN_POINT('Ctrl Pts',(38.8858050047217,-6.216610570833,-1.88918205659997));
#35279=CARTESIAN_POINT('Ctrl Pts',(38.9797198586102,-4.7840918117624,-4.8187084571317));
#35280=CARTESIAN_POINT('Ctrl Pts',(39.1067199799055,-0.992468299979939,
-6.39510333440429));
#35281=CARTESIAN_POINT('Ctrl Pts',(39.2059757821266,2.19083962730784,-6.10933350657059));
#35282=CARTESIAN_POINT('Ctrl Pts',(39.3052315843476,4.83030849556222,-4.30702447425982));
#35283=CARTESIAN_POINT('Ctrl Pts',(39.4375726539757,6.83706805014439,-0.527822103558383));
#35284=CARTESIAN_POINT('Ctrl Pts',(39.6029989910108,5.28773755787813,5.10909189367368));
#35285=CARTESIAN_POINT('Ctrl Pts',(39.8015105954529,-1.43545748919326,7.2110849456744));
#35286=CARTESIAN_POINT('Ctrl Pts',(39.9588360711961,-5.71561946767958,3.6414683897976));
#35287=CARTESIAN_POINT('Ctrl Pts',(40.0499910121252,-6.21521743271123,0.786535449862077));
#35288=CARTESIAN_POINT('Ctrl Pts',(40.0749754182403,-6.21056889989778,0.00266732454412187));
#35289=CARTESIAN_POINT('Ctrl Pts',(39.0714645817597,-6.21925,4.64436579980868E-13));
#35290=CARTESIAN_POINT('Ctrl Pts',(39.1302643332334,-6.21925000000014,-1.83816020915697));
#35291=CARTESIAN_POINT('Ctrl Pts',(39.1890640847071,-5.35502977485042,-3.65808141345913));
#35292=CARTESIAN_POINT('Ctrl Pts',(39.2478638361808,-3.93049712175866,-4.81977830800825));
#35293=CARTESIAN_POINT('Ctrl Pts',(39.3066635876544,-2.5059644686669,-5.98147520255737));
#35294=CARTESIAN_POINT('Ctrl Pts',(39.3654633391281,-0.549389021418988,
-6.46189408921053));
#35295=CARTESIAN_POINT('Ctrl Pts',(39.4242630906018,1.2511886986689,-6.09209302315905));
#35296=CARTESIAN_POINT('Ctrl Pts',(39.4830628420755,3.0517664187568,-5.72229195710758));
#35297=CARTESIAN_POINT('Ctrl Pts',(39.5418625935492,4.66061422075212,-4.50960958424927));
#35298=CARTESIAN_POINT('Ctrl Pts',(39.6006623450229,5.51197192302719,-2.88049233331039));
#35299=CARTESIAN_POINT('Ctrl Pts',(39.6594620964966,6.36332962530226,-1.25137508237152));
#35300=CARTESIAN_POINT('Ctrl Pts',(39.7182618479703,6.44030216377281,0.761847462641284));
#35301=CARTESIAN_POINT('Ctrl Pts',(39.777061599444,5.71582172177438,2.45121451680431));
#35302=CARTESIAN_POINT('Ctrl Pts',(39.8358613509177,4.99134127977594,4.14058157096734));
#35303=CARTESIAN_POINT('Ctrl Pts',(39.8946611023914,3.47978506146448,5.47256790209481));
#35304=CARTESIAN_POINT('Ctrl Pts',(39.9534608538651,1.71270012775635,5.9787731881117));
#35305=CARTESIAN_POINT('Ctrl Pts',(40.0122606053388,-0.0543848059517801,
6.4849784741286));
#35306=CARTESIAN_POINT('Ctrl Pts',(40.0710603568125,-2.04193092337447,6.15535714814314));
#35307=CARTESIAN_POINT('Ctrl Pts',(40.1298601082862,-3.55100669662459,5.10582236305057));
#35308=CARTESIAN_POINT('Ctrl Pts',(40.1886598597599,-5.0600824698747,4.05628757795801));
#35309=CARTESIAN_POINT('Ctrl Pts',(40.2474596112336,-6.06074051980838,2.30766719190237));
#35310=CARTESIAN_POINT('Ctrl Pts',(40.3062593627073,-6.20109393743674,0.474873184740152));
#35311=CARTESIAN_POINT('Ctrl Pts',(40.3113277690581,-6.21319208641581,0.316890462828103));
#35312=CARTESIAN_POINT('Ctrl Pts',(40.3163961754089,-6.21924999999998,0.158445276457359));
#35313=CARTESIAN_POINT('Ctrl Pts',(40.3214645817597,-6.21925,5.98531144183268E-13));
#35314=CARTESIAN_POINT('Origin',(28.1999754182402,0.,0.));
#35315=CARTESIAN_POINT('',(37.5749754182404,-6.21630311580474,-0.00309819098741701));
#35316=CARTESIAN_POINT('',(37.8214645817596,-6.22702764812334,0.00572193935648446));
#35317=CARTESIAN_POINT('',(28.1999754182402,-6.21925,5.68729293530136E-12));
#35318=CARTESIAN_POINT('Ctrl Pts',(37.5749754182404,-6.21630311580474,-0.00309819098741684));
#35319=CARTESIAN_POINT('Ctrl Pts',(37.5892779276901,-6.22053647474818,-0.45026242937358));
#35320=CARTESIAN_POINT('Ctrl Pts',(37.6366657045469,-6.07611397572792,-1.93034435153842));
#35321=CARTESIAN_POINT('Ctrl Pts',(37.7171387488107,-4.88576711085616,-4.2440098636368));
#35322=CARTESIAN_POINT('Ctrl Pts',(37.8163945510318,-2.26989742046013,-6.08040293629282));
#35323=CARTESIAN_POINT('Ctrl Pts',(37.9156503532528,0.909436095338548,-6.40743833155411));
#35324=CARTESIAN_POINT('Ctrl Pts',(38.0479914228809,4.88148948210039,-4.81613497853341));
#35325=CARTESIAN_POINT('Ctrl Pts',(38.213417759916,7.33645041645639,0.489370765242909));
#35326=CARTESIAN_POINT('Ctrl Pts',(38.4119293643581,3.55798549376158,6.43436271305828));
#35327=CARTESIAN_POINT('Ctrl Pts',(38.6104409688003,-3.4742282511699,6.47997086072042));
#35328=CARTESIAN_POINT('Ctrl Pts',(38.748122986761,-6.14812552610466,2.39103132068625));
#35329=CARTESIAN_POINT('Ctrl Pts',(38.8196344699077,-6.2291535028914,0.168211027796827));
#35330=CARTESIAN_POINT('Ctrl Pts',(38.8249754182403,-6.22814110134059,0.00214874350932153));
#35331=CARTESIAN_POINT('Ctrl Pts',(37.8214645817596,-6.22702764812334,0.00572193935648436));
#35332=CARTESIAN_POINT('Ctrl Pts',(37.8809249244144,-6.214154207475,-1.84534440380487));
#35333=CARTESIAN_POINT('Ctrl Pts',(38.0065558018834,-4.3540617358176,-5.78681812394731));
#35334=CARTESIAN_POINT('Ctrl Pts',(38.1983572141661,2.33652476986658,-6.97143717584924));
#35335=CARTESIAN_POINT('Ctrl Pts',(38.3968688186083,7.12719834562496,-1.8072167000993));
#35336=CARTESIAN_POINT('Ctrl Pts',(38.5622951556433,5.67151826603053,3.85460455214176));
#35337=CARTESIAN_POINT('Ctrl Pts',(38.6946362252714,2.05246604268208,6.13756654772971));
#35338=CARTESIAN_POINT('Ctrl Pts',(38.7938920274925,-1.13361812652741,6.39051203819357));
#35339=CARTESIAN_POINT('Ctrl Pts',(38.8931478297135,-4.03830067804228,5.0571204867886));
#35340=CARTESIAN_POINT('Ctrl Pts',(38.9856720144692,-5.86513335389985,2.6881251712379));
#35341=CARTESIAN_POINT('Ctrl Pts',(39.045110931818,-6.21100116850847,0.82596242185995));
#35342=CARTESIAN_POINT('Ctrl Pts',(39.0714645817597,-6.20771145695589,-0.000133645472617031));
#35343=CARTESIAN_POINT('Origin',(28.1999754182402,0.,0.));
#35344=CARTESIAN_POINT('',(36.3249754182403,-6.2162013314378,-0.0011376377559993));
#35345=CARTESIAN_POINT('',(36.5714645817597,-6.2210655398886,-0.00528659965813971));
#35346=CARTESIAN_POINT('',(28.1999754182402,-6.21925,5.68729293530136E-12));
#35347=CARTESIAN_POINT('Ctrl Pts',(36.3249754182403,-6.2162013314378,-0.00113763775599949));
#35348=CARTESIAN_POINT('Ctrl Pts',(36.3258361180656,-6.21614725314266,-0.0281046714168168));
#35349=CARTESIAN_POINT('Ctrl Pts',(36.3597820852978,-6.20720164280366,-1.09161759141586));
#35350=CARTESIAN_POINT('Ctrl Pts',(36.426813319937,-5.65834786130082,-3.17912466680208));
#35351=CARTESIAN_POINT('Ctrl Pts',(36.526069122158,-3.44104873410895,-5.48101483247933));
#35352=CARTESIAN_POINT('Ctrl Pts',(36.6584101917862,0.619923098873849,-6.82933313338426));
#35353=CARTESIAN_POINT('Ctrl Pts',(36.8238365288212,5.919465903525,-4.36152632411429));
#35354=CARTESIAN_POINT('Ctrl Pts',(37.0223481332634,6.8706564039049,2.61808419966792));
#35355=CARTESIAN_POINT('Ctrl Pts',(37.2208597377055,1.52886927114417,7.19185949867951));
#35356=CARTESIAN_POINT('Ctrl Pts',(37.4050688326978,-4.73470315697655,5.32239779041791));
#35357=CARTESIAN_POINT('Ctrl Pts',(37.5231073928761,-6.20095084704205,1.61854213304384));
#35358=CARTESIAN_POINT('Ctrl Pts',(37.5749754182404,-6.21630311580474,-0.00309819098741684));
#35359=CARTESIAN_POINT('Ctrl Pts',(36.5714645817597,-6.2210655398886,-0.0052865996581393));
#35360=CARTESIAN_POINT('Ctrl Pts',(36.5843978473829,-6.2249967155556,-0.409366363204161));
#35361=CARTESIAN_POINT('Ctrl Pts',(36.6635016478201,-6.00657242484259,-2.87671415514283));
#35362=CARTESIAN_POINT('Ctrl Pts',(36.8087759830713,-2.71506717634408,-6.83291259456277));
#35363=CARTESIAN_POINT('Ctrl Pts',(37.0072875875135,4.27730707652595,-5.98060470455043));
#35364=CARTESIAN_POINT('Ctrl Pts',(37.1727139245486,6.81987484110359,-0.716521351391848));
#35365=CARTESIAN_POINT('Ctrl Pts',(37.3050549941766,5.52916938658696,3.36312739553527));
#35366=CARTESIAN_POINT('Ctrl Pts',(37.4043107963977,3.25889279038126,5.6127846874694));
#35367=CARTESIAN_POINT('Ctrl Pts',(37.5035665986187,0.179650915968158,6.46916266085227));
#35368=CARTESIAN_POINT('Ctrl Pts',(37.6359076682469,-4.00324642534526,5.56759497029643));
#35369=CARTESIAN_POINT('Ctrl Pts',(37.7418736626271,-6.12426506880607,2.48148226091111));
#35370=CARTESIAN_POINT('Ctrl Pts',(37.8147543896004,-6.22848043592516,0.214617655518784));
#35371=CARTESIAN_POINT('Ctrl Pts',(37.8214645817596,-6.22702764812334,0.00572193935648436));
#35372=CARTESIAN_POINT('Origin',(28.1999754182402,0.,0.));
#35373=CARTESIAN_POINT('',(35.0749754182404,-6.21859864471026,0.00324434653253106));
#35374=CARTESIAN_POINT('',(35.3214645817596,-6.210630471212,-0.000241035779820487));
#35375=CARTESIAN_POINT('',(28.1999754182402,-6.21925,5.68729293530136E-12));
#35376=CARTESIAN_POINT('Ctrl Pts',(35.0749754182404,-6.21859864471025,0.00324434653253113));
#35377=CARTESIAN_POINT('Ctrl Pts',(35.095479575848,-6.21654040868293,-0.636816772095382));
#35378=CARTESIAN_POINT('Ctrl Pts',(35.1490690008627,-5.95386142902179,-2.31247659416935));
#35379=CARTESIAN_POINT('Ctrl Pts',(35.2688289606914,-3.93449142709178,-5.61639323287909));
#35380=CARTESIAN_POINT('Ctrl Pts',(35.4342552977265,1.706159430506,-7.15206323045347));
#35381=CARTESIAN_POINT('Ctrl Pts',(35.6327669021685,6.93766837888352,-2.43496237142141));
#35382=CARTESIAN_POINT('Ctrl Pts',(35.8312785066107,5.80973766223456,4.50635469098045));
#35383=CARTESIAN_POINT('Ctrl Pts',(36.0297901110528,-0.646180895956555,
7.3243046569134));
#35384=CARTESIAN_POINT('Ctrl Pts',(36.1943557482627,-5.48506849708825,4.09851879072839));
#35385=CARTESIAN_POINT('Ctrl Pts',(36.2927508506585,-6.21822602067945,1.00850704118591));
#35386=CARTESIAN_POINT('Ctrl Pts',(36.3249754182403,-6.2162013314378,-0.00113763775599949));
#35387=CARTESIAN_POINT('Ctrl Pts',(35.3214645817596,-6.210630471212,-0.00024103577982007));
#35388=CARTESIAN_POINT('Ctrl Pts',(35.3540413051653,-6.21100194781226,-1.02236541662845));
#35389=CARTESIAN_POINT('Ctrl Pts',(35.452788563385,-5.48716606870768,-4.12015825613875));
#35390=CARTESIAN_POINT('Ctrl Pts',(35.6177063564187,-0.593159681851761,
-7.32878912572931));
#35391=CARTESIAN_POINT('Ctrl Pts',(35.7831326934538,4.74656140271064,-4.94916665150982));
#35392=CARTESIAN_POINT('Ctrl Pts',(35.9154737630819,6.39392461916095,-1.00003397421454));
#35393=CARTESIAN_POINT('Ctrl Pts',(36.0147295653029,6.1119213231936,2.18360983365812));
#35394=CARTESIAN_POINT('Ctrl Pts',(36.1139853675239,4.31273644099712,4.82520925710656));
#35395=CARTESIAN_POINT('Ctrl Pts',(36.2463264371521,0.535911013730674,6.83643877180359));
#35396=CARTESIAN_POINT('Ctrl Pts',(36.3988195085639,-4.66198719373343,5.41438603443864));
#35397=CARTESIAN_POINT('Ctrl Pts',(36.5182273125688,-6.20488362084988,1.65802905264626));
#35398=CARTESIAN_POINT('Ctrl Pts',(36.5714645817597,-6.2210655398886,-0.0052865996581393));
#35399=CARTESIAN_POINT('Origin',(28.1999754182402,0.,0.));
#35400=CARTESIAN_POINT('',(33.8249754182404,-6.22651516743638,-0.00167075726269435));
#35401=CARTESIAN_POINT('',(34.0714645817596,-6.22005335440933,0.0053417081121826));
#35402=CARTESIAN_POINT('',(28.1999754182402,-6.21925,5.68729293530136E-12));
#35403=CARTESIAN_POINT('Ctrl Pts',(33.8249754182403,-6.22651516743638,-0.0016707572626945));
#35404=CARTESIAN_POINT('Ctrl Pts',(33.8320377662234,-6.22722193989077,-0.222213824936918));
#35405=CARTESIAN_POINT('Ctrl Pts',(33.9052706490206,-6.10845944272299,-2.50753618971029));
#35406=CARTESIAN_POINT('Ctrl Pts',(34.0446740666317,-3.31312753510712,-6.56400641995886));
#35407=CARTESIAN_POINT('Ctrl Pts',(34.2431856710738,3.72736559794809,-6.33774649263565));
#35408=CARTESIAN_POINT('Ctrl Pts',(34.4416972755159,7.34611894960073,-0.307926448941118));
#35409=CARTESIAN_POINT('Ctrl Pts',(34.640208879958,4.233914906245,6.01140200914276));
#35410=CARTESIAN_POINT('Ctrl Pts',(34.8056352169931,-1.57434350116745,6.67424438783693));
#35411=CARTESIAN_POINT('Ctrl Pts',(34.9379762866212,-4.99945699673356,4.10947315312662));
#35412=CARTESIAN_POINT('Ctrl Pts',(35.0167279312346,-6.08991113296614,1.82004144531782));
#35413=CARTESIAN_POINT('Ctrl Pts',(35.062394308441,-6.21986155411372,0.395978316191532));
#35414=CARTESIAN_POINT('Ctrl Pts',(35.0749754182404,-6.21859864471025,0.00324434653253113));
#35415=CARTESIAN_POINT('Ctrl Pts',(34.0714645817596,-6.22005335440933,0.00534170811218225));
#35416=CARTESIAN_POINT('Ctrl Pts',(34.1236847629477,-6.20409670026243,-1.62686967844328));
#35417=CARTESIAN_POINT('Ctrl Pts',(34.2420754789499,-4.70995884997351,-5.35226492593367));
#35418=CARTESIAN_POINT('Ctrl Pts',(34.393551462359,0.430999447686097,-6.84385381815942));
#35419=CARTESIAN_POINT('Ctrl Pts',(34.5258925319871,4.23822627631683,-4.89078499723656));
#35420=CARTESIAN_POINT('Ctrl Pts',(34.6251483342081,6.07771306114946,-2.27708986044939));
#35421=CARTESIAN_POINT('Ctrl Pts',(34.7244041364292,6.40850984162318,0.901854494708191));
#35422=CARTESIAN_POINT('Ctrl Pts',(34.8567452060572,4.82190714720603,4.87578785427672));
#35423=CARTESIAN_POINT('Ctrl Pts',(35.0221715430924,-0.48069030065227,7.33702428029021));
#35424=CARTESIAN_POINT('Ctrl Pts',(35.1881064241288,-5.45381342879383,4.1845056440569));
#35425=CARTESIAN_POINT('Ctrl Pts',(35.2878707703512,-6.2102473966254,1.05379540792869));
#35426=CARTESIAN_POINT('Ctrl Pts',(35.3214645817596,-6.210630471212,-0.00024103577982007));
#35427=CARTESIAN_POINT('Origin',(28.1999754182402,0.,0.));
#35428=CARTESIAN_POINT('',(32.5749754182403,-6.21844556314562,-0.000466044233505376));
#35429=CARTESIAN_POINT('',(32.8214645817597,-6.22773255198024,-0.00518142285415191));
#35430=CARTESIAN_POINT('',(28.1999754182402,-6.21925,5.68729293530136E-12));
#35431=CARTESIAN_POINT('Ctrl Pts',(32.5749754182403,-6.20937279635969,-0.00572228109726187));
#35432=CARTESIAN_POINT('Ctrl Pts',(32.6016812240059,-6.21396328164207,-0.84203719014262));
#35433=CARTESIAN_POINT('Ctrl Pts',(32.6945575645854,-5.66911297578352,-3.74417462738773));
#35434=CARTESIAN_POINT('Ctrl Pts',(32.853604439979,-1.24379023624101,-7.2466418339485));
#35435=CARTESIAN_POINT('Ctrl Pts',(33.0521160444211,5.41227178463782,-4.97673046693937));
#35436=CARTESIAN_POINT('Ctrl Pts',(33.2506276488633,7.11391162562153,1.85873863792625));
#35437=CARTESIAN_POINT('Ctrl Pts',(33.4160539858983,3.10541110519021,6.11397050225541));
#35438=CARTESIAN_POINT('Ctrl Pts',(33.5483950555264,-1.16614656773419,6.36572295470293));
#35439=CARTESIAN_POINT('Ctrl Pts',(33.6476508577475,-4.07834394078075,5.04884480068));
#35440=CARTESIAN_POINT('Ctrl Pts',(33.7398443119854,-5.84299343888296,2.66154714325195));
#35441=CARTESIAN_POINT('Ctrl Pts',(33.7989524988164,-6.22391089437088,0.810973209496164));
#35442=CARTESIAN_POINT('Ctrl Pts',(33.8249754182403,-6.22651516743638,-0.0016707572626945));
#35443=CARTESIAN_POINT('Ctrl Pts',(32.8214645817597,-6.22773255198024,-0.00518142285415288));
#35444=CARTESIAN_POINT('Ctrl Pts',(32.8271576859162,-6.22883195533547,-0.182350455011576));
#35445=CARTESIAN_POINT('Ctrl Pts',(32.8990213248867,-6.14169081306461,-2.41719204780253));
#35446=CARTESIAN_POINT('Ctrl Pts',(33.0039702312642,-4.08817544863011,-5.50554583451141));
#35447=CARTESIAN_POINT('Ctrl Pts',(33.1363113008923,0.0804192017098835,
-6.47115594816462));
#35448=CARTESIAN_POINT('Ctrl Pts',(33.2355671031134,3.17242495854284,-5.66210588059523));
#35449=CARTESIAN_POINT('Ctrl Pts',(33.3348229053343,5.47694100310651,-3.44753091698999));
#35450=CARTESIAN_POINT('Ctrl Pts',(33.4671639749625,6.83006089629673,0.611842341327977));
#35451=CARTESIAN_POINT('Ctrl Pts',(33.6325903119975,4.36852741272638,5.91430153013899));
#35452=CARTESIAN_POINT('Ctrl Pts',(33.8311019164398,-2.60995361271077,6.87374912585412));
#35453=CARTESIAN_POINT('Ctrl Pts',(33.9773933396937,-5.98521297716978,2.94115569332543));
#35454=CARTESIAN_POINT('Ctrl Pts',(34.0575142281337,-6.22431609274099,0.441378610258281));
#35455=CARTESIAN_POINT('Ctrl Pts',(34.0714645817596,-6.22005335440933,0.00534170811218225));
#35456=CARTESIAN_POINT('Origin',(28.1999754182402,0.,0.));
#35457=CARTESIAN_POINT('',(31.3249754182403,-6.21925,7.0933178088184E-13));
#35458=CARTESIAN_POINT('',(31.5714645817597,-6.20816386984268,-0.000295703980951467));
#35459=CARTESIAN_POINT('',(28.1999754182402,-6.21925,5.68729293530136E-12));
#35460=CARTESIAN_POINT('Ctrl Pts',(31.3249754182403,-6.21925,6.65141351788081E-13));
#35461=CARTESIAN_POINT('Ctrl Pts',(31.383775169714,-6.2192500000002,-1.83816020915679));
#35462=CARTESIAN_POINT('Ctrl Pts',(31.4425749211877,-5.35502977485053,-3.65808141345899));
#35463=CARTESIAN_POINT('Ctrl Pts',(31.5013746726614,-3.93049712175878,-4.81977830800815));
#35464=CARTESIAN_POINT('Ctrl Pts',(31.5601744241351,-2.50596446866704,-5.98147520255732));
#35465=CARTESIAN_POINT('Ctrl Pts',(31.6189741756088,-0.549389021419119,
-6.46189408921052));
#35466=CARTESIAN_POINT('Ctrl Pts',(31.6777739270825,1.25118869866879,-6.09209302315908));
#35467=CARTESIAN_POINT('Ctrl Pts',(31.7365736785562,3.05176641875671,-5.72229195710763));
#35468=CARTESIAN_POINT('Ctrl Pts',(31.7953734300299,4.66061422075206,-4.50960958424933));
#35469=CARTESIAN_POINT('Ctrl Pts',(31.8541731815036,5.51197192302716,-2.88049233331045));
#35470=CARTESIAN_POINT('Ctrl Pts',(31.9129729329773,6.36332962530225,-1.25137508237158));
#35471=CARTESIAN_POINT('Ctrl Pts',(31.971772684451,6.44030216377282,0.761847462641246));
#35472=CARTESIAN_POINT('Ctrl Pts',(32.0305724359247,5.71582172177439,2.45121451680429));
#35473=CARTESIAN_POINT('Ctrl Pts',(32.0893721873984,4.99134127977595,4.14058157096734));
#35474=CARTESIAN_POINT('Ctrl Pts',(32.1481719388721,3.47978506146448,5.47256790209481));
#35475=CARTESIAN_POINT('Ctrl Pts',(32.2069716903458,1.71270012775633,5.97877318811171));
#35476=CARTESIAN_POINT('Ctrl Pts',(32.2657714418195,-0.0543848059518154,
6.4849784741286));
#35477=CARTESIAN_POINT('Ctrl Pts',(32.3245711932932,-2.04193092337452,6.15535714814312));
#35478=CARTESIAN_POINT('Ctrl Pts',(32.3833709447669,-3.55100669662464,5.10582236305054));
#35479=CARTESIAN_POINT('Ctrl Pts',(32.4421706962406,-5.06008246987476,4.05628757795795));
#35480=CARTESIAN_POINT('Ctrl Pts',(32.5009704477143,-6.06074051980842,2.30766719190228));
#35481=CARTESIAN_POINT('Ctrl Pts',(32.559770199188,-6.20109393743675,0.474873184740044));
#35482=CARTESIAN_POINT('Ctrl Pts',(32.5648386055388,-6.21319208641581,0.316890462828053));
#35483=CARTESIAN_POINT('Ctrl Pts',(32.5699070118896,-6.21924999999998,0.158445276457369));
#35484=CARTESIAN_POINT('Ctrl Pts',(32.5749754182403,-6.21925,6.666646287092E-13));
#35485=CARTESIAN_POINT('Ctrl Pts',(31.5714645817597,-6.20816386984268,-0.000295703980950981));
#35486=CARTESIAN_POINT('Ctrl Pts',(31.5968011436986,-6.21130704176283,-0.794297582896872));
#35487=CARTESIAN_POINT('Ctrl Pts',(31.6552229730446,-5.88436859534305,-2.6238606368355));
#35488=CARTESIAN_POINT('Ctrl Pts',(31.7467300697975,-4.11675109351076,-4.99488165618313));
#35489=CARTESIAN_POINT('Ctrl Pts',(31.8459858720185,-1.23075458232488,-6.37221708890274));
#35490=CARTESIAN_POINT('Ctrl Pts',(31.9452416742396,1.95775582174799,-6.16839483200312));
#35491=CARTESIAN_POINT('Ctrl Pts',(32.0775827438677,5.61197648499354,-3.94108216408908));
#35492=CARTESIAN_POINT('Ctrl Pts',(32.2430090809028,7.15393902550158,1.69766694268016));
#35493=CARTESIAN_POINT('Ctrl Pts',(32.4415206853449,2.4432388603139,6.93479746587837));
#35494=CARTESIAN_POINT('Ctrl Pts',(32.6343391856305,-4.30040480542789,5.84717018705371));
#35495=CARTESIAN_POINT('Ctrl Pts',(32.7609871511021,-6.21605367023959,1.87687229730388));
#35496=CARTESIAN_POINT('Ctrl Pts',(32.8214645817597,-6.22773255198024,-0.00518142285415288));
#35497=CARTESIAN_POINT('Origin',(-8.,0.,2.1));
#35498=CARTESIAN_POINT('',(0.,-9.,2.1));
#35499=CARTESIAN_POINT('',(-16.,9.,2.1));
#35500=CARTESIAN_POINT('Origin',(-16.,9.,0.));
#35501=CARTESIAN_POINT('',(-16.,9.,-2.1));
#35502=CARTESIAN_POINT('Origin',(-8.,0.,-2.1));
#35503=CARTESIAN_POINT('',(0.,-9.,-2.1));
#35504=CARTESIAN_POINT('Origin',(0.,-9.,0.));
#35505=CARTESIAN_POINT('Origin',(109.067,1.12618006296016E-15,0.));
#35506=CARTESIAN_POINT('',(109.067,6.85892174064777,1.01078264511681));
#35507=CARTESIAN_POINT('Ctrl Pts',(109.067,-2.15756780909041,-5.83789702209075));
#35508=CARTESIAN_POINT('Ctrl Pts',(109.067,-2.0135726607274,-5.9015965205511));
#35509=CARTESIAN_POINT('Ctrl Pts',(109.067,-1.86728073205768,-5.95949577427964));
#35510=CARTESIAN_POINT('Ctrl Pts',(109.067,-1.71893720698406,-6.01134642449991));
#35511=CARTESIAN_POINT('Ctrl Pts',(109.067,-1.55748216789094,-6.06777995440398));
#35512=CARTESIAN_POINT('Ctrl Pts',(109.067,-1.39359690962913,-6.11704974662805));
#35513=CARTESIAN_POINT('Ctrl Pts',(109.067,-1.22777124491188,-6.15927407685968));
#35514=CARTESIAN_POINT('Ctrl Pts',(109.067,-1.12095704707141,-6.18647226702362));
#35515=CARTESIAN_POINT('Ctrl Pts',(109.067,-1.01333719076962,-6.21074625738224));
#35516=CARTESIAN_POINT('Ctrl Pts',(109.067,-0.905038201094559,-6.2321171997402));
#35517=CARTESIAN_POINT('Ctrl Pts',(109.067,-0.842383954466684,-6.24448093736308));
#35518=CARTESIAN_POINT('Ctrl Pts',(109.067,-0.779502349592861,-6.25587288063033));
#35519=CARTESIAN_POINT('Ctrl Pts',(109.067,-0.716417544951752,-6.26629587236679));
#35520=CARTESIAN_POINT('Ctrl Pts',(109.067,-0.682837053570036,-6.2718441051967));
#35521=CARTESIAN_POINT('Ctrl Pts',(109.067,-0.64919898185994,-6.27711776920991));
#35522=CARTESIAN_POINT('Ctrl Pts',(109.067,-0.615506954172322,-6.28211718696264));
#35523=CARTESIAN_POINT('Ctrl Pts',(109.067,-0.590641187520192,-6.28580691310166));
#35524=CARTESIAN_POINT('Ctrl Pts',(109.067,-0.565749932528012,-6.28934664569366));
#35525=CARTESIAN_POINT('Ctrl Pts',(109.067,-0.540842974343021,-6.29273560102282));
#35526=CARTESIAN_POINT('Ctrl Pts',(109.067,-0.366963296689134,-6.31639446999596));
#35527=CARTESIAN_POINT('Ctrl Pts',(109.067,-0.192199995525417,-6.3327270073782));
#35528=CARTESIAN_POINT('Ctrl Pts',(109.067,-0.0170658993305209,-6.34185755124692));
#35529=CARTESIAN_POINT('Ctrl Pts',(109.067,0.159767917302458,-6.35107670933961));
#35530=CARTESIAN_POINT('Ctrl Pts',(109.067,0.336980514165373,-6.35295346928648));
#35531=CARTESIAN_POINT('Ctrl Pts',(109.067,0.514059064472075,-6.34756433866805));
#35532=CARTESIAN_POINT('Ctrl Pts',(109.067,0.663134169149158,-6.34302745258179));
#35533=CARTESIAN_POINT('Ctrl Pts',(109.067,0.812114778451582,-6.33334015175942));
#35534=CARTESIAN_POINT('Ctrl Pts',(109.067,0.960697048025707,-6.3185197289033));
#35535=CARTESIAN_POINT('Ctrl Pts',(109.067,0.986307215777789,-6.31596522817728));
#35536=CARTESIAN_POINT('Ctrl Pts',(109.067,1.01190554605928,-6.31325816427479));
#35537=CARTESIAN_POINT('Ctrl Pts',(109.067,1.03749047650535,-6.31039854793851));
#35538=CARTESIAN_POINT('Ctrl Pts',(109.067,1.06164020100599,-6.30769934393465));
#35539=CARTESIAN_POINT('Ctrl Pts',(109.067,1.08576977624899,-6.30486512412045));
#35540=CARTESIAN_POINT('Ctrl Pts',(109.067,1.10987372754823,-6.30189671902766));
#35541=CARTESIAN_POINT('Ctrl Pts',(109.067,1.20838784565032,-6.28976469111842));
#35542=CARTESIAN_POINT('Ctrl Pts',(109.067,1.30649618888237,-6.2753891231948));
#35543=CARTESIAN_POINT('Ctrl Pts',(109.067,1.40411036563822,-6.25879202047389));
#35544=CARTESIAN_POINT('Ctrl Pts',(109.067,1.57975009016904,-6.22892842230823));
#35545=CARTESIAN_POINT('Ctrl Pts',(109.067,1.75378995004789,-6.19187556201615));
#35546=CARTESIAN_POINT('Ctrl Pts',(109.067,1.9258564963741,-6.14786245476911));
#35547=CARTESIAN_POINT('Ctrl Pts',(109.067,2.09942770353434,-6.10346446853151));
#35548=CARTESIAN_POINT('Ctrl Pts',(109.067,2.27099158455466,-6.05198385933624));
#35549=CARTESIAN_POINT('Ctrl Pts',(109.067,2.44016284904198,-5.99360265655463));
#35550=CARTESIAN_POINT('Ctrl Pts',(109.067,2.61121284388512,-5.93457310171272));
#35551=CARTESIAN_POINT('Ctrl Pts',(109.067,2.7798174976817,-5.86848873919628));
#35552=CARTESIAN_POINT('Ctrl Pts',(109.067,2.94556620576367,-5.79548528379882));
#35553=CARTESIAN_POINT('Ctrl Pts',(109.067,3.06987773682515,-5.74073269225073));
#35554=CARTESIAN_POINT('Ctrl Pts',(109.067,3.1925826133881,-5.68208701342321));
#35555=CARTESIAN_POINT('Ctrl Pts',(109.067,3.31349941504197,-5.6195869992619));
#35556=CARTESIAN_POINT('Ctrl Pts',(109.067,3.34663878643761,-5.60245777360265));
#35557=CARTESIAN_POINT('Ctrl Pts',(109.067,3.37964379966736,-5.58503894784604));
#35558=CARTESIAN_POINT('Ctrl Pts',(109.067,3.4125105980543,-5.56733111927243));
#35559=CARTESIAN_POINT('Ctrl Pts',(109.067,3.43139568280936,-5.55715629665954));
#35560=CARTESIAN_POINT('Ctrl Pts',(109.067,3.45023242661829,-5.54688747547546));
#35561=CARTESIAN_POINT('Ctrl Pts',(109.067,3.46901112922455,-5.53652991792905));
#35562=CARTESIAN_POINT('Ctrl Pts',(109.067,3.62877163156698,-5.44841261657179));
#35563=CARTESIAN_POINT('Ctrl Pts',(109.067,3.78452202689656,-5.35377495289507));
#35564=CARTESIAN_POINT('Ctrl Pts',(109.067,3.93587605353499,-5.25282511603666));
#35565=CARTESIAN_POINT('Ctrl Pts',(109.067,4.07468561123279,-5.16024216654266));
#35566=CARTESIAN_POINT('Ctrl Pts',(109.067,4.20979769549856,-5.06234929407872));
#35567=CARTESIAN_POINT('Ctrl Pts',(109.067,4.34090372720216,-4.95927004899439));
#35568=CARTESIAN_POINT('Ctrl Pts',(109.067,4.48236568874247,-4.84804868095934));
#35569=CARTESIAN_POINT('Ctrl Pts',(109.067,4.61916464818014,-4.73078973445163));
#35570=CARTESIAN_POINT('Ctrl Pts',(109.067,4.75105064478682,-4.60792710833882));
#35571=CARTESIAN_POINT('Ctrl Pts',(109.067,4.88388391613822,-4.4841820180844));
#35572=CARTESIAN_POINT('Ctrl Pts',(109.067,5.01173392221482,-4.35475193857044));
#35573=CARTESIAN_POINT('Ctrl Pts',(109.067,5.13431262660541,-4.22003860820336));
#35574=CARTESIAN_POINT('Ctrl Pts',(109.067,5.19748221283924,-4.15061557602353));
#35575=CARTESIAN_POINT('Ctrl Pts',(109.067,5.25925129919297,-4.07978882346575));
#35576=CARTESIAN_POINT('Ctrl Pts',(109.067,5.31957640477001,-4.0076097744433));
#35577=CARTESIAN_POINT('Ctrl Pts',(109.067,5.33808213817268,-3.98546764595979));
#35578=CARTESIAN_POINT('Ctrl Pts',(109.067,5.35645196334427,-3.96319824319762));
#35579=CARTESIAN_POINT('Ctrl Pts',(109.067,5.3746845673014,-3.94080301147104));
#35580=CARTESIAN_POINT('Ctrl Pts',(109.067,5.38726994465937,-3.92534430667161));
#35581=CARTESIAN_POINT('Ctrl Pts',(109.067,5.39978828430919,-3.90982764047081));
#35582=CARTESIAN_POINT('Ctrl Pts',(109.067,5.41223383221326,-3.89426036487904));
#35583=CARTESIAN_POINT('Ctrl Pts',(109.067,5.52700188467733,-3.750704941236));
#35584=CARTESIAN_POINT('Ctrl Pts',(109.067,5.6357169848108,-3.60268437046879));
#35585=CARTESIAN_POINT('Ctrl Pts',(109.067,5.73814962803564,-3.45067190929303));
#35586=CARTESIAN_POINT('Ctrl Pts',(109.067,5.84145552549992,-3.29736351820676));
#35587=CARTESIAN_POINT('Ctrl Pts',(109.067,5.93837191258434,-3.13999433806236));
#35588=CARTESIAN_POINT('Ctrl Pts',(109.067,6.02863118663199,-2.97900751654019));
#35589=CARTESIAN_POINT('Ctrl Pts',(109.067,6.11884425326949,-2.81810311074946));
#35590=CARTESIAN_POINT('Ctrl Pts',(109.067,6.20240750924262,-2.65358415770578));
#35591=CARTESIAN_POINT('Ctrl Pts',(109.067,6.27901423903501,-2.48585980888858));
#35592=CARTESIAN_POINT('Ctrl Pts',(109.067,6.30202101264031,-2.43548830586537));
#35593=CARTESIAN_POINT('Ctrl Pts',(109.067,6.32440005144439,-2.38482750170827));
#35594=CARTESIAN_POINT('Ctrl Pts',(109.067,6.34614224786266,-2.33388801902908));
#35595=CARTESIAN_POINT('Ctrl Pts',(109.067,6.40204411734148,-2.20291632429923));
#35596=CARTESIAN_POINT('Ctrl Pts',(109.067,6.45373726838296,-2.07010281771283));
#35597=CARTESIAN_POINT('Ctrl Pts',(109.067,6.5011990215905,-1.93564346445603));
#35598=CARTESIAN_POINT('Ctrl Pts',(109.067,6.5219635386188,-1.87681749740618));
#35599=CARTESIAN_POINT('Ctrl Pts',(109.067,6.54191791372575,-1.81767642326058));
#35600=CARTESIAN_POINT('Ctrl Pts',(109.067,6.56105917890401,-1.75823633122607));
#35601=CARTESIAN_POINT('Ctrl Pts',(109.067,6.57150884537305,-1.72578658817798));
#35602=CARTESIAN_POINT('Ctrl Pts',(109.067,6.58171616720908,-1.69324772523769));
#35603=CARTESIAN_POINT('Ctrl Pts',(109.067,6.59168057800658,-1.66062234252173));
#35604=CARTESIAN_POINT('Ctrl Pts',(109.067,6.59948481623486,-1.63506977707871));
#35605=CARTESIAN_POINT('Ctrl Pts',(109.067,6.6071405710643,-1.60946211965833));
#35606=CARTESIAN_POINT('Ctrl Pts',(109.067,6.61464142664228,-1.58382220961391));
#35607=CARTESIAN_POINT('Ctrl Pts',(109.067,6.66647256761742,-1.40664964865927));
#35608=CARTESIAN_POINT('Ctrl Pts',(109.067,6.71098048972246,-1.22771717878011));
#35609=CARTESIAN_POINT('Ctrl Pts',(109.067,6.74821024821888,-1.04748636093756));
#35610=CARTESIAN_POINT('Ctrl Pts',(109.067,6.78607258251663,-0.8641932171862));
#35611=CARTESIAN_POINT('Ctrl Pts',(109.067,6.81640757241096,-0.679556633939157));
#35612=CARTESIAN_POINT('Ctrl Pts',(109.067,6.83921525633307,-0.494036516019991));
#35613=CARTESIAN_POINT('Ctrl Pts',(109.067,6.8620662536148,-0.308164082643737));
#35614=CARTESIAN_POINT('Ctrl Pts',(109.067,6.87736147631527,-0.121404073567072));
#35615=CARTESIAN_POINT('Ctrl Pts',(109.067,6.88505100358449,0.0657966891430848));
#35616=CARTESIAN_POINT('Ctrl Pts',(109.067,6.89266799101194,0.251231476750997));
#35617=CARTESIAN_POINT('Ctrl Pts',(109.067,6.89282216605126,0.437099421891961));
#35618=CARTESIAN_POINT('Ctrl Pts',(109.067,6.88541461247308,0.62297144031264));
#35619=CARTESIAN_POINT('Ctrl Pts',(109.067,6.88026095061278,0.752288295347639));
#35620=CARTESIAN_POINT('Ctrl Pts',(109.067,6.87144606107714,0.881607238796431));
#35621=CARTESIAN_POINT('Ctrl Pts',(109.067,6.85892174064777,1.01078264511681));
#35622=CARTESIAN_POINT('',(109.067,-6.933,-8.4904762584886E-16));
#35623=CARTESIAN_POINT('Origin',(109.067,0.,0.));
#35624=CARTESIAN_POINT('',(109.067,3.46348981423002,6.00884185984444));
#35625=CARTESIAN_POINT('Origin',(109.067,0.,0.));
#35626=CARTESIAN_POINT('Ctrl Pts',(109.067,3.46405146923353,6.01146880811302));
#35627=CARTESIAN_POINT('Ctrl Pts',(109.067,3.30912874255884,6.09212153599444));
#35628=CARTESIAN_POINT('Ctrl Pts',(109.067,3.1512484438972,6.16654224984595));
#35629=CARTESIAN_POINT('Ctrl Pts',(109.067,2.99061701977446,6.23440908312552));
#35630=CARTESIAN_POINT('Ctrl Pts',(109.067,2.81845433699699,6.30714787724899));
#35631=CARTESIAN_POINT('Ctrl Pts',(109.067,2.64313094670355,6.37235874611403));
#35632=CARTESIAN_POINT('Ctrl Pts',(109.067,2.46518012087715,6.43006589265));
#35633=CARTESIAN_POINT('Ctrl Pts',(109.067,2.35251751740855,6.4666009148242));
#35634=CARTESIAN_POINT('Ctrl Pts',(109.067,2.23880142696933,6.50012719452215));
#35635=CARTESIAN_POINT('Ctrl Pts',(109.067,2.1241655087431,6.53064026904539));
#35636=CARTESIAN_POINT('Ctrl Pts',(109.067,2.06495123148562,6.54640155645648));
#35637=CARTESIAN_POINT('Ctrl Pts',(109.067,2.00549151947031,6.56135873964514));
#35638=CARTESIAN_POINT('Ctrl Pts',(109.067,1.94580478784761,6.57551034809967));
#35639=CARTESIAN_POINT('Ctrl Pts',(109.067,1.90531981645002,6.58510925639864));
#35640=CARTESIAN_POINT('Ctrl Pts',(109.067,1.86473039837682,6.59433752490925));
#35641=CARTESIAN_POINT('Ctrl Pts',(109.067,1.82404229299711,6.60319454242566));
#35642=CARTESIAN_POINT('Ctrl Pts',(109.067,1.79431097931758,6.6096664772476));
#35643=CARTESIAN_POINT('Ctrl Pts',(109.067,1.76452539060412,6.61594044050794));
#35644=CARTESIAN_POINT('Ctrl Pts',(109.067,1.7347064700501,6.62201254137047));
#35645=CARTESIAN_POINT('Ctrl Pts',(109.067,1.55155509466467,6.65930811088765));
#35646=CARTESIAN_POINT('Ctrl Pts',(109.067,1.36699117500837,6.68902756324626));
#35647=CARTESIAN_POINT('Ctrl Pts',(109.067,1.18154536859613,6.71119870068649));
#35648=CARTESIAN_POINT('Ctrl Pts',(109.067,0.996051600557548,6.73337557222138));
#35649=CARTESIAN_POINT('Ctrl Pts',(109.067,0.809674689036533,6.74800018653563));
#35650=CARTESIAN_POINT('Ctrl Pts',(109.067,0.622944059228044,6.75504829234912));
#35651=CARTESIAN_POINT('Ctrl Pts',(109.067,0.460793212061621,6.76116863977015));
#35652=CARTESIAN_POINT('Ctrl Pts',(109.067,0.298375303328641,6.76157501218272));
#35653=CARTESIAN_POINT('Ctrl Pts',(109.067,0.136043018085803,6.75621996754557));
#35654=CARTESIAN_POINT('Ctrl Pts',(109.067,0.105092913226025,6.75519898029832));
#35655=CARTESIAN_POINT('Ctrl Pts',(109.067,0.074145947935451,6.75396847540538));
#35656=CARTESIAN_POINT('Ctrl Pts',(109.067,0.0432046090642379,6.75252800360357));
#35657=CARTESIAN_POINT('Ctrl Pts',(109.067,0.020305459140885,6.75146193532879));
#35658=CARTESIAN_POINT('Ctrl Pts',(109.067,-0.00258678730564892,6.75028101279484));
#35659=CARTESIAN_POINT('Ctrl Pts',(109.067,-0.0254628612165071,6.74898570654463));
#35660=CARTESIAN_POINT('Ctrl Pts',(109.067,-0.133799396937078,6.74285139379534));
#35661=CARTESIAN_POINT('Ctrl Pts',(109.067,-0.241828769116266,6.73414967973701));
#35662=CARTESIAN_POINT('Ctrl Pts',(109.067,-0.349448736226522,6.72288662725207));
#35663=CARTESIAN_POINT('Ctrl Pts',(109.067,-0.532719427466918,6.70370628860471));
#35664=CARTESIAN_POINT('Ctrl Pts',(109.067,-0.71480348606703,6.6771008732754));
#35665=CARTESIAN_POINT('Ctrl Pts',(109.067,-0.895302658472974,6.64322184101536));
#35666=CARTESIAN_POINT('Ctrl Pts',(109.067,-1.07613522511967,6.60928023187983));
#35667=CARTESIAN_POINT('Ctrl Pts',(109.067,-1.25537769913326,6.56803789023454));
#35668=CARTESIAN_POINT('Ctrl Pts',(109.067,-1.43261590046417,6.51959676567458));
#35669=CARTESIAN_POINT('Ctrl Pts',(109.067,-1.6104255942165,6.4709994460316));
#35670=CARTESIAN_POINT('Ctrl Pts',(109.067,-1.78621873701221,6.41515664486632));
#35671=CARTESIAN_POINT('Ctrl Pts',(109.067,-1.95955339481228,6.35212381902113));
#35672=CARTESIAN_POINT('Ctrl Pts',(109.067,-2.08955438816234,6.30484919963723));
#35673=CARTESIAN_POINT('Ctrl Pts',(109.067,-2.21817205794986,6.25352919760746));
#35674=CARTESIAN_POINT('Ctrl Pts',(109.067,-2.34520781399991,6.19817078339132));
#35675=CARTESIAN_POINT('Ctrl Pts',(109.067,-2.38702415979058,6.17994846029692));
#35676=CARTESIAN_POINT('Ctrl Pts',(109.067,-2.42866900487268,6.16128845441856));
#35677=CARTESIAN_POINT('Ctrl Pts',(109.067,-2.47013496906611,6.14219069678272));
#35678=CARTESIAN_POINT('Ctrl Pts',(109.067,-2.49201710721469,6.13211255730026));
#35679=CARTESIAN_POINT('Ctrl Pts',(109.067,-2.51384261560681,6.12191561532782));
#35680=CARTESIAN_POINT('Ctrl Pts',(109.067,-2.53560342805358,6.11160351080748));
#35681=CARTESIAN_POINT('Ctrl Pts',(109.067,-2.69890086127494,6.03421944238624));
#35682=CARTESIAN_POINT('Ctrl Pts',(109.067,-2.85868286445364,5.95029614110067));
#35683=CARTESIAN_POINT('Ctrl Pts',(109.067,-3.01456652439573,5.8599486944075));
#35684=CARTESIAN_POINT('Ctrl Pts',(109.067,-3.15730235684114,5.77722149889608));
#35685=CARTESIAN_POINT('Ctrl Pts',(109.067,-3.29676987486409,5.68910744517844));
#35686=CARTESIAN_POINT('Ctrl Pts',(109.067,-3.43265613191939,5.59566156792999));
#35687=CARTESIAN_POINT('Ctrl Pts',(109.067,-3.58145554886069,5.49333560538265));
#35688=CARTESIAN_POINT('Ctrl Pts',(109.067,-3.72596163392383,5.38461635190157));
#35689=CARTESIAN_POINT('Ctrl Pts',(109.067,-3.86583639657926,5.26988938971029));
#35690=CARTESIAN_POINT('Ctrl Pts',(109.067,-4.00522968928239,5.15555733496311));
#35691=CARTESIAN_POINT('Ctrl Pts',(109.067,-4.1400239540109,5.03525822345385));
#35692=CARTESIAN_POINT('Ctrl Pts',(109.067,-4.26984353036136,4.90934272162992));
#35693=CARTESIAN_POINT('Ctrl Pts',(109.067,-4.33436650584876,4.84676015075681));
#35694=CARTESIAN_POINT('Ctrl Pts',(109.067,-4.39765990532932,4.78278974609324));
#35695=CARTESIAN_POINT('Ctrl Pts',(109.067,-4.45967325628869,4.71747243917582));
#35696=CARTESIAN_POINT('Ctrl Pts',(109.067,-4.477009225061,4.69921284224235));
#35697=CARTESIAN_POINT('Ctrl Pts',(109.067,-4.49424514026326,4.6808479786264));
#35698=CARTESIAN_POINT('Ctrl Pts',(109.067,-4.51137985542899,4.66237872705053));
#35699=CARTESIAN_POINT('Ctrl Pts',(109.067,-4.52593111622634,4.64669414205375));
#35700=CARTESIAN_POINT('Ctrl Pts',(109.067,-4.54040839081441,4.63093529486271));
#35701=CARTESIAN_POINT('Ctrl Pts',(109.067,-4.55480284574971,4.61511188698257));
#35702=CARTESIAN_POINT('Ctrl Pts',(109.067,-4.67524484062003,4.48271348639725));
#35703=CARTESIAN_POINT('Ctrl Pts',(109.067,-4.79005070725105,4.34562748465468));
#35704=CARTESIAN_POINT('Ctrl Pts',(109.067,-4.89892627992167,4.20425211433211));
#35705=CARTESIAN_POINT('Ctrl Pts',(109.067,-5.00772778645258,4.06297291919076));
#35706=CARTESIAN_POINT('Ctrl Pts',(109.067,-5.11060752150017,3.91740955440837));
#35707=CARTESIAN_POINT('Ctrl Pts',(109.067,-5.20723092161534,3.76792762612764));
#35708=CARTESIAN_POINT('Ctrl Pts',(109.067,-5.30260180511279,3.6203834127172));
#35709=CARTESIAN_POINT('Ctrl Pts',(109.067,-5.39187784502882,3.46902093588031));
#35710=CARTESIAN_POINT('Ctrl Pts',(109.067,-5.47469157281416,3.3141702583193));
#35711=CARTESIAN_POINT('Ctrl Pts',(109.067,-5.49803287402587,3.27052512357597));
#35712=CARTESIAN_POINT('Ctrl Pts',(109.067,-5.52086050257896,3.22660278126208));
#35713=CARTESIAN_POINT('Ctrl Pts',(109.067,-5.54316550433805,3.18241041195473));
#35714=CARTESIAN_POINT('Ctrl Pts',(109.067,-5.60230175559497,3.06524516430197));
#35715=CARTESIAN_POINT('Ctrl Pts',(109.067,-5.65776545712255,2.94618196012103));
#35716=CARTESIAN_POINT('Ctrl Pts',(109.067,-5.70950047684215,2.82539173952989));
#35717=CARTESIAN_POINT('Ctrl Pts',(109.067,-5.73213454796948,2.77254601802126));
#35718=CARTESIAN_POINT('Ctrl Pts',(109.067,-5.75405472907524,2.71936971398817));
#35719=CARTESIAN_POINT('Ctrl Pts',(109.067,-5.7752553910661,2.665877096622));
#35720=CARTESIAN_POINT('Ctrl Pts',(109.067,-5.78798264815911,2.63376421759534));
#35721=CARTESIAN_POINT('Ctrl Pts',(109.067,-5.80045058798087,2.60153734283538));
#35722=CARTESIAN_POINT('Ctrl Pts',(109.067,-5.81265789335266,2.56919956290054));
#35723=CARTESIAN_POINT('Ctrl Pts',(109.067,-5.82219808721407,2.54392709856629));
#35724=CARTESIAN_POINT('Ctrl Pts',(109.067,-5.83158011004563,2.5185839007308));
#35725=CARTESIAN_POINT('Ctrl Pts',(109.067,-5.84079494789832,2.49319504473949));
#35726=CARTESIAN_POINT('Ctrl Pts',(109.067,-5.90045856108198,2.32880898529301));
#35727=CARTESIAN_POINT('Ctrl Pts',(109.067,-5.95319307428684,2.16231505043118));
#35728=CARTESIAN_POINT('Ctrl Pts',(109.067,-5.99896322840551,1.99414444801905));
#35729=CARTESIAN_POINT('Ctrl Pts',(109.067,-6.04501451703568,1.82494088950119));
#35730=CARTESIAN_POINT('Ctrl Pts',(109.067,-6.08401576538923,1.65403930183469));
#35731=CARTESIAN_POINT('Ctrl Pts',(109.067,-6.11588044698519,1.48186537531838));
#35732=CARTESIAN_POINT('Ctrl Pts',(109.067,-6.14757987742922,1.31058434771906));
#35733=CARTESIAN_POINT('Ctrl Pts',(109.067,-6.17221661993806,1.13804344736959));
#35734=CARTESIAN_POINT('Ctrl Pts',(109.067,-6.18965430287559,0.96465894100687));
#35735=CARTESIAN_POINT('Ctrl Pts',(109.067,-6.20678035459018,0.794373012932948));
#35736=CARTESIAN_POINT('Ctrl Pts',(109.067,-6.21696230688685,0.6232727421406));
#35737=CARTESIAN_POINT('Ctrl Pts',(109.067,-6.22002164922363,0.451759430133508));
#35738=CARTESIAN_POINT('Ctrl Pts',(109.067,-6.22187578004815,0.347812867898749));
#35739=CARTESIAN_POINT('Ctrl Pts',(109.067,-6.22111280177593,0.243714769828713));
#35740=CARTESIAN_POINT('Ctrl Pts',(109.067,-6.21768400249992,0.139557183822751));
#35741=CARTESIAN_POINT('Ctrl Pts',(30.6549162453659,0.653767430832815,-6.1847925356379));
#35742=CARTESIAN_POINT('Ctrl Pts',(30.6880015127729,1.68232745378033,-6.07606794386137));
#35743=CARTESIAN_POINT('Ctrl Pts',(30.7541720475869,3.67991374771159,-5.3378881315643));
#35744=CARTESIAN_POINT('Ctrl Pts',(30.853427849808,5.79294729058132,-2.91848348878711));
#35745=CARTESIAN_POINT('Ctrl Pts',(30.9526836520291,6.46975467895848,0.195461407864942));
#35746=CARTESIAN_POINT('Ctrl Pts',(31.0850247216571,5.32189755126117,4.32218967016898));
#35747=CARTESIAN_POINT('Ctrl Pts',(31.2504510586922,0.326999582929717,7.34773416501965));
#35748=CARTESIAN_POINT('Ctrl Pts',(31.4489626631343,-6.0124639065617,4.23976817199318));
#35749=CARTESIAN_POINT('Ctrl Pts',(31.6143890001695,-6.67314725497242,-1.56582020690343));
#35750=CARTESIAN_POINT('Ctrl Pts',(31.7467300697975,-4.11675109351076,-4.99488165618313));
#35751=CARTESIAN_POINT('Ctrl Pts',(31.8459858720185,-1.23075458232488,-6.37221708890274));
#35752=CARTESIAN_POINT('Ctrl Pts',(31.9452416742396,1.95775582174799,-6.16839483200312));
#35753=CARTESIAN_POINT('Ctrl Pts',(32.0775827438677,5.61197648499354,-3.94108216408908));
#35754=CARTESIAN_POINT('Ctrl Pts',(32.2430090809028,7.15393902550158,1.69766694268016));
#35755=CARTESIAN_POINT('Ctrl Pts',(32.4415206853449,2.4432388603139,6.93479746587837));
#35756=CARTESIAN_POINT('Ctrl Pts',(32.640032289787,-4.49951570882378,5.81505721359621));
#35757=CARTESIAN_POINT('Ctrl Pts',(32.8385438942291,-7.32504123893786,-0.637509834538132));
#35758=CARTESIAN_POINT('Ctrl Pts',(33.0039702312642,-4.08817544863011,-5.50554583451141));
#35759=CARTESIAN_POINT('Ctrl Pts',(33.1363113008923,0.0804192017098835,
-6.47115594816462));
#35760=CARTESIAN_POINT('Ctrl Pts',(33.2355671031134,3.17242495854284,-5.66210588059523));
#35761=CARTESIAN_POINT('Ctrl Pts',(33.3348229053343,5.47694100310651,-3.44753091698999));
#35762=CARTESIAN_POINT('Ctrl Pts',(33.4671639749625,6.83006089629673,0.611842341327977));
#35763=CARTESIAN_POINT('Ctrl Pts',(33.6325903119975,4.36852741272638,5.91430153013899));
#35764=CARTESIAN_POINT('Ctrl Pts',(33.8311019164398,-2.60995361271077,6.87374912585412));
#35765=CARTESIAN_POINT('Ctrl Pts',(34.0296135208817,-7.19004543862418,1.53737728295951));
#35766=CARTESIAN_POINT('Ctrl Pts',(34.2281251253239,-5.18342127361679,-5.21489534401854));
#35767=CARTESIAN_POINT('Ctrl Pts',(34.393551462359,0.430999447686097,-6.84385381815942));
#35768=CARTESIAN_POINT('Ctrl Pts',(34.5258925319871,4.23822627631683,-4.89078499723656));
#35769=CARTESIAN_POINT('Ctrl Pts',(34.6251483342081,6.07771306114946,-2.27708986044939));
#35770=CARTESIAN_POINT('Ctrl Pts',(34.7244041364292,6.40850984162318,0.901854494708191));
#35771=CARTESIAN_POINT('Ctrl Pts',(34.8567452060572,4.82190714720603,4.87578785427672));
#35772=CARTESIAN_POINT('Ctrl Pts',(35.0221715430924,-0.48069030065227,7.33702428029021));
#35773=CARTESIAN_POINT('Ctrl Pts',(35.2206831475344,-6.43014857662837,3.56559582231111));
#35774=CARTESIAN_POINT('Ctrl Pts',(35.4191947519766,-6.48407686024324,-3.46655903964816));
#35775=CARTESIAN_POINT('Ctrl Pts',(35.6177063564187,-0.593159681851761,
-7.32878912572931));
#35776=CARTESIAN_POINT('Ctrl Pts',(35.7831326934538,4.74656140271064,-4.94916665150982));
#35777=CARTESIAN_POINT('Ctrl Pts',(35.9154737630819,6.39392461916095,-1.00003397421454));
#35778=CARTESIAN_POINT('Ctrl Pts',(36.0147295653029,6.1119213231936,2.18360983365812));
#35779=CARTESIAN_POINT('Ctrl Pts',(36.1139853675239,4.31273644099712,4.82520925710656));
#35780=CARTESIAN_POINT('Ctrl Pts',(36.2463264371521,0.535911013730674,6.83643877180359));
#35781=CARTESIAN_POINT('Ctrl Pts',(36.4117527741871,-5.10283212902811,5.29377868085695));
#35782=CARTESIAN_POINT('Ctrl Pts',(36.6102643786293,-7.21277826054165,-1.42692468663486));
#35783=CARTESIAN_POINT('Ctrl Pts',(36.8087759830713,-2.71506717634408,-6.83291259456277));
#35784=CARTESIAN_POINT('Ctrl Pts',(37.0072875875135,4.27730707652595,-5.98060470455043));
#35785=CARTESIAN_POINT('Ctrl Pts',(37.1727139245486,6.81987484110359,-0.716521351391848));
#35786=CARTESIAN_POINT('Ctrl Pts',(37.3050549941766,5.52916938658696,3.36312739553527));
#35787=CARTESIAN_POINT('Ctrl Pts',(37.4043107963977,3.25889279038126,5.6127846874694));
#35788=CARTESIAN_POINT('Ctrl Pts',(37.5035665986187,0.179650915968158,6.46916266085227));
#35789=CARTESIAN_POINT('Ctrl Pts',(37.6359076682469,-4.00324642534526,5.56759497029643));
#35790=CARTESIAN_POINT('Ctrl Pts',(37.8013340052818,-7.31442513907121,0.749782197655131));
#35791=CARTESIAN_POINT('Ctrl Pts',(37.9998456097241,-4.58813259367446,-5.74537410443173));
#35792=CARTESIAN_POINT('Ctrl Pts',(38.1983572141661,2.33652476986658,-6.97143717584924));
#35793=CARTESIAN_POINT('Ctrl Pts',(38.3968688186083,7.12719834562496,-1.8072167000993));
#35794=CARTESIAN_POINT('Ctrl Pts',(38.5622951556433,5.67151826603053,3.85460455214176));
#35795=CARTESIAN_POINT('Ctrl Pts',(38.6946362252714,2.05246604268208,6.13756654772971));
#35796=CARTESIAN_POINT('Ctrl Pts',(38.7938920274925,-1.13361812652741,6.39051203819357));
#35797=CARTESIAN_POINT('Ctrl Pts',(38.8931478297135,-4.03830067804228,5.0571204867886));
#35798=CARTESIAN_POINT('Ctrl Pts',(39.0254888993416,-6.65129306476565,1.66865103059635));
#35799=CARTESIAN_POINT('Ctrl Pts',(39.1909152363767,-6.07072539313457,-4.14840712323998));
#35800=CARTESIAN_POINT('Ctrl Pts',(39.3894268408188,0.203920765924685,-7.34974153411109));
#35801=CARTESIAN_POINT('Ctrl Pts',(39.5879384452609,6.28435572899307,-3.81669456054382));
#35802=CARTESIAN_POINT('Ctrl Pts',(39.786450049703,6.61024172910176,3.21989017543126));
#35803=CARTESIAN_POINT('Ctrl Pts',(39.9518763867381,1.8439687800484,6.60483722990331));
#35804=CARTESIAN_POINT('Ctrl Pts',(40.0842174563662,-2.39381056423673,6.01265423641858));
#35805=CARTESIAN_POINT('Ctrl Pts',(40.1834732585872,-4.99061430015067,4.14939791707426));
#35806=CARTESIAN_POINT('Ctrl Pts',(40.2827290608084,-6.34858204315922,1.25612341171161));
#35807=CARTESIAN_POINT('Ctrl Pts',(40.4150701304363,-6.15730676139607,-3.01855414749781));
#35808=CARTESIAN_POINT('Ctrl Pts',(40.5804964674716,-1.95924956424283,-7.08691255794874));
#35809=CARTESIAN_POINT('Ctrl Pts',(40.7790080719135,4.89964311770096,-5.48213294404453));
#35810=CARTESIAN_POINT('Ctrl Pts',(40.9775196763558,7.26349285183276,1.1410328165251));
#35811=CARTESIAN_POINT('Ctrl Pts',(41.1760312807977,2.97064458683377,6.72593927996026));
#35812=CARTESIAN_POINT('Ctrl Pts',(41.3414576178329,-2.85466105015735,6.23498243654499));
#35813=CARTESIAN_POINT('Ctrl Pts',(41.473798687461,-5.70926470123999,3.04739832567862));
#35814=CARTESIAN_POINT('Ctrl Pts',(41.573054489682,-6.49007271635678,-0.0518681355929193));
#35815=CARTESIAN_POINT('Ctrl Pts',(41.6723102919031,-5.65982942715753,-3.13825920530084));
#35816=CARTESIAN_POINT('Ctrl Pts',(41.8046513615312,-2.7546438300705,-6.2798115469148));
#35817=CARTESIAN_POINT('Ctrl Pts',(41.9700776985662,3.07776459442245,-6.67760088357463));
#35818=CARTESIAN_POINT('Ctrl Pts',(42.1685893030084,7.280801980269,-1.02479599000183));
#35819=CARTESIAN_POINT('Ctrl Pts',(42.3671009074504,4.81139734096477,5.55974279300492));
#35820=CARTESIAN_POINT('Ctrl Pts',(42.5656125118927,-2.0722681306563,7.05469299499727));
#35821=CARTESIAN_POINT('Ctrl Pts',(42.7310388489277,-6.20476526695897,2.91975746890894));
#35822=CARTESIAN_POINT('Ctrl Pts',(42.8633799185558,-6.32769472643081,-1.35743118914858));
#35823=CARTESIAN_POINT('Ctrl Pts',(42.9626357207768,-4.92365776368081,-4.22863197656575));
#35824=CARTESIAN_POINT('Ctrl Pts',(43.0618915229979,-2.29740564112336,-6.05014605644428));
#35825=CARTESIAN_POINT('Ctrl Pts',(43.1942325926259,1.94929714981741,-6.57452175576472));
#35826=CARTESIAN_POINT('Ctrl Pts',(43.3596589296611,6.6608602966818,-3.11382860271486));
#35827=CARTESIAN_POINT('Ctrl Pts',(43.5581705341031,6.22255147548853,3.9166487501317));
#35828=CARTESIAN_POINT('Ctrl Pts',(43.7566821385453,0.0864251429686191,
7.35206195510319));
#35829=CARTESIAN_POINT('Ctrl Pts',(43.9551937429874,-6.13625319161177,4.05084993889327));
#35830=CARTESIAN_POINT('Ctrl Pts',(44.1206200800225,-6.62377372820908,-1.77474428941108));
#35831=CARTESIAN_POINT('Ctrl Pts',(44.2529611496505,-3.9569578199035,-5.12101794526032));
#35832=CARTESIAN_POINT('Ctrl Pts',(44.3522169518716,-1.03133493987818,-6.40781416778569));
#35833=CARTESIAN_POINT('Ctrl Pts',(44.4514727540926,2.15029947849091,-6.10397838601804));
#35834=CARTESIAN_POINT('Ctrl Pts',(44.5838138237208,5.73240126379457,-3.76346535073147));
#35835=CARTESIAN_POINT('Ctrl Pts',(44.7492401607558,7.09740355031088,1.92089856656498));
#35836=CARTESIAN_POINT('Ctrl Pts',(44.9477517651979,2.22480311159819,7.00789093890849));
#35837=CARTESIAN_POINT('Ctrl Pts',(45.1462633696401,-4.67937380009033,5.67130894380136));
#35838=CARTESIAN_POINT('Ctrl Pts',(45.3447749740821,-7.30150721100801,-0.866591545421022));
#35839=CARTESIAN_POINT('Ctrl Pts',(45.5102013111172,-3.91374922444537,-5.63086695842329));
#35840=CARTESIAN_POINT('Ctrl Pts',(45.6425423807454,0.283023412847933,-6.46546500508306));
#35841=CARTESIAN_POINT('Ctrl Pts',(45.7417981829663,3.34818463267598,-5.55998145973536));
#35842=CARTESIAN_POINT('Ctrl Pts',(45.8410539851874,5.58221537749888,-3.27432610828378));
#35843=CARTESIAN_POINT('Ctrl Pts',(45.9733950548155,6.80755168564738,0.825430640665489));
#35844=CARTESIAN_POINT('Ctrl Pts',(46.1388213918506,4.18117380984599,6.04820419883911));
#35845=CARTESIAN_POINT('Ctrl Pts',(46.3373329962928,-2.82392956463494,6.78864538114884));
#35846=CARTESIAN_POINT('Ctrl Pts',(46.5358446007348,-7.23466322442155,1.31146190421813));
#35847=CARTESIAN_POINT('Ctrl Pts',(46.734356205177,-5.01757083003903,-5.37466012176944));
#35848=CARTESIAN_POINT('Ctrl Pts',(46.899782542212,0.645108111263187,-6.82700016259648));
#35849=CARTESIAN_POINT('Ctrl Pts',(47.0321236118402,4.38930599811985,-4.75566323860751));
#35850=CARTESIAN_POINT('Ctrl Pts',(47.1313794140611,6.14604086368536,-2.08564519249999));
#35851=CARTESIAN_POINT('Ctrl Pts',(47.2306352162823,6.37712454126565,1.10209916493979));
#35852=CARTESIAN_POINT('Ctrl Pts',(47.3629762859102,4.66685348261288,5.0243979009563));
#35853=CARTESIAN_POINT('Ctrl Pts',(47.5284026229454,-0.710218612843849,
7.31837263201097));
#35854=CARTESIAN_POINT('Ctrl Pts',(47.7269142273875,-6.5386540061078,3.36248242901333));
#35855=CARTESIAN_POINT('Ctrl Pts',(47.9254258318296,-6.37233896675448,-3.66791226582583));
#35856=CARTESIAN_POINT('Ctrl Pts',(48.1239374362717,-0.363362580539744,
-7.34376988297294));
#35857=CARTESIAN_POINT('Ctrl Pts',(48.2893637733068,4.89922005122494,-4.79809739219469));
#35858=CARTESIAN_POINT('Ctrl Pts',(48.4217048429349,6.42210544142411,-0.79931325736819));
#35859=CARTESIAN_POINT('Ctrl Pts',(48.5209606451559,6.04054241262091,2.37393797905852));
#35860=CARTESIAN_POINT('Ctrl Pts',(48.620216447377,4.1595164104518,4.95789907272788));
#35861=CARTESIAN_POINT('Ctrl Pts',(48.7525575170051,0.321560287482606,6.84986822331817));
#35862=CARTESIAN_POINT('Ctrl Pts',(48.9179838540402,-5.26610780985881,5.1313835360399));
#35863=CARTESIAN_POINT('Ctrl Pts',(49.1164954584823,-7.1645555542505,-1.65209806218378));
#35864=CARTESIAN_POINT('Ctrl Pts',(49.3150070629244,-2.4997580926362,-6.91458558232614));
#35865=CARTESIAN_POINT('Ctrl Pts',(49.5135186673665,4.46249608146065,-5.84372459840002));
#35866=CARTESIAN_POINT('Ctrl Pts',(49.6789450044016,6.838968356171,-0.502600754676708));
#35867=CARTESIAN_POINT('Ctrl Pts',(49.8112860740297,5.42113886922714,3.53462775193207));
#35868=CARTESIAN_POINT('Ctrl Pts',(49.9105418762507,3.08152614660459,5.71208637669992));
#35869=CARTESIAN_POINT('Ctrl Pts',(50.0097976784718,-0.0230235705233395,
6.47161571011243));
#35870=CARTESIAN_POINT('Ctrl Pts',(50.1421387480999,-4.17563615511025,5.43949982952901));
#35871=CARTESIAN_POINT('Ctrl Pts',(50.3075650851349,-7.33431768531273,0.52035809776168));
#35872=CARTESIAN_POINT('Ctrl Pts',(50.5060766895771,-4.40596188428978,-5.88623684294122));
#35873=CARTESIAN_POINT('Ctrl Pts',(50.7045882940192,2.55369426009361,-6.89484807105841));
#35874=CARTESIAN_POINT('Ctrl Pts',(50.9030998984613,7.1802970231816,-1.58313711278791));
#35875=CARTESIAN_POINT('Ctrl Pts',(51.0685262354964,5.54802698009573,4.03032161538502));
#35876=CARTESIAN_POINT('Ctrl Pts',(51.2008673051245,1.8592571864357,6.19883075255818));
#35877=CARTESIAN_POINT('Ctrl Pts',(51.3001231073455,-1.33318551163412,6.35187771912034));
#35878=CARTESIAN_POINT('Ctrl Pts',(51.3993789095666,-4.19468734797827,4.92817796319135));
#35879=CARTESIAN_POINT('Ctrl Pts',(51.5317199791946,-6.70028587202019,1.45954271212482));
#35880=CARTESIAN_POINT('Ctrl Pts',(51.6971463162298,-5.93783767930351,-4.33648154074716));
#35881=CARTESIAN_POINT('Ctrl Pts',(51.8956579206718,0.433983073355225,-7.33975088058538));
#35882=CARTESIAN_POINT('Ctrl Pts',(52.094169525114,6.40079599604896,-3.61802361987541));
#35883=CARTESIAN_POINT('Ctrl Pts',(52.2926811295561,6.50616656657558,3.42531532372877));
#35884=CARTESIAN_POINT('Ctrl Pts',(52.4581074665912,1.63622927289707,6.65934302028545));
#35885=CARTESIAN_POINT('Ctrl Pts',(52.5904485362193,-2.58092699663894,5.93474142841911));
#35886=CARTESIAN_POINT('Ctrl Pts',(52.6897043384402,-5.11810793105627,3.99107822187782));
#35887=CARTESIAN_POINT('Ctrl Pts',(52.7889601406614,-6.38480472479868,1.05669702865221));
#35888=CARTESIAN_POINT('Ctrl Pts',(52.9213012102894,-6.05975872316839,-3.20989406558761));
#35889=CARTESIAN_POINT('Ctrl Pts',(53.0867275473246,-1.73635698912002,-7.14479200994201));
#35890=CARTESIAN_POINT('Ctrl Pts',(53.2852391517666,5.06891690010915,-5.32600842627953));
#35891=CARTESIAN_POINT('Ctrl Pts',(53.4837507562088,7.22419817707089,1.36793457278422));
#35892=CARTESIAN_POINT('Ctrl Pts',(53.6822623606508,2.75856009795156,6.81566831976048));
#35893=CARTESIAN_POINT('Ctrl Pts',(53.847688697686,-3.04851381910718,6.14252872927938));
#35894=CARTESIAN_POINT('Ctrl Pts',(53.980029767314,-5.80189597337518,2.86711407138024));
#35895=CARTESIAN_POINT('Ctrl Pts',(54.0792855695351,-6.4852653283173,-0.255083885053564));
#35896=CARTESIAN_POINT('Ctrl Pts',(54.1785413717561,-5.55877673210131,-3.31396156085478));
#35897=CARTESIAN_POINT('Ctrl Pts',(54.3108824413843,-2.55663608376213,-6.36299517762788));
#35898=CARTESIAN_POINT('Ctrl Pts',(54.4763087784192,3.28536884845591,-6.57794344674629));
#35899=CARTESIAN_POINT('Ctrl Pts',(54.6748203828615,7.30932326741656,-0.796289940546589));
#35900=CARTESIAN_POINT('Ctrl Pts',(54.8733319873035,4.63493030483003,5.70768826815035));
#35901=CARTESIAN_POINT('Ctrl Pts',(55.0718435917456,-2.29217444186588,6.98633843920073));
#35902=CARTESIAN_POINT('Ctrl Pts',(55.2372699287808,-6.29315635428496,2.72401886847961));
#35903=CARTESIAN_POINT('Ctrl Pts',(55.3696109984087,-6.28208235318225,-1.55492163532759));
#35904=CARTESIAN_POINT('Ctrl Pts',(55.4688668006299,-4.78882033941213,-4.38074581822788));
#35905=CARTESIAN_POINT('Ctrl Pts',(55.5681226028509,-2.10681428668835,-6.11912359293222));
#35906=CARTESIAN_POINT('Ctrl Pts',(55.700463672479,2.1542268731561,-6.51025362595669));
#35907=CARTESIAN_POINT('Ctrl Pts',(55.865890009514,6.75510516300982,-2.90371188234558));
#35908=CARTESIAN_POINT('Ctrl Pts',(56.0644016139562,6.09684697384953,4.10959137560839));
#35909=CARTESIAN_POINT('Ctrl Pts',(56.2629132183983,-0.143852232229424,
7.35116254971248));
#35910=CARTESIAN_POINT('Ctrl Pts',(56.4614248228404,-6.26009883682339,3.85670209015414));
#35911=CARTESIAN_POINT('Ctrl Pts',(56.6268511598755,-6.56494768793653,-1.98130198353674));
#35912=CARTESIAN_POINT('Ctrl Pts',(56.7591922295036,-3.7946488264813,-5.24242122190289));
#35913=CARTESIAN_POINT('Ctrl Pts',(56.8584480317246,-0.830163910262025,
-6.43696838963711));
#35914=CARTESIAN_POINT('Ctrl Pts',(56.9577038339457,2.34039522251466,-6.03364650825719));
#35915=CARTESIAN_POINT('Ctrl Pts',(57.0900449035737,5.84744533060766,-3.58210535870519));
#35916=CARTESIAN_POINT('Ctrl Pts',(57.2554712406089,7.03376829111499,2.14221662907907));
#35917=CARTESIAN_POINT('Ctrl Pts',(57.4539828450509,2.00425491144597,7.07412514357485));
#35918=CARTESIAN_POINT('Ctrl Pts',(57.6524944494932,-4.85467979449576,5.52198953185602));
#35919=CARTESIAN_POINT('Ctrl Pts',(57.8510060539352,-7.27078821313233,-1.09481834966948));
#35920=CARTESIAN_POINT('Ctrl Pts',(58.0164323909703,-3.73549514279114,-5.75066706856635));
#35921=CARTESIAN_POINT('Ctrl Pts',(58.1487734605983,0.485355182835179,-6.45343089609464));
#35922=CARTESIAN_POINT('Ctrl Pts',(58.2480292628194,3.52065721958024,-5.45240377350268));
#35923=CARTESIAN_POINT('Ctrl Pts',(58.3472850650405,5.68201536485552,-3.09790919455678));
#35924=CARTESIAN_POINT('Ctrl Pts',(58.4796261346685,6.77836393432703,1.03820906811895));
#35925=CARTESIAN_POINT('Ctrl Pts',(58.6450524717037,3.98971935895797,6.17617421190118));
#35926=CARTESIAN_POINT('Ctrl Pts',(58.8435640761457,-3.03513575029629,6.69688250414221));
#35927=CARTESIAN_POINT('Ctrl Pts',(59.0420756805879,-7.27218428522181,1.08426012505574));
#35928=CARTESIAN_POINT('Ctrl Pts',(59.2405872850299,-4.84679866862674,-5.52915283970294));
#35929=CARTESIAN_POINT('Ctrl Pts',(59.406013622065,0.858584021869272,-6.80344979938125));
#35930=CARTESIAN_POINT('Ctrl Pts',(59.5383546916932,4.53608016947545,-4.61587658850033));
#35931=CARTESIAN_POINT('Ctrl Pts',(59.6376104939142,6.20833994062302,-1.89215468415061));
#35932=CARTESIAN_POINT('Ctrl Pts',(59.7368662961353,6.33948382661728,1.30126276986307));
#35933=CARTESIAN_POINT('Ctrl Pts',(59.8692073657633,4.50722204056254,5.16807944718129));
#35934=CARTESIAN_POINT('Ctrl Pts',(60.0346337027984,-0.939050263787701,
7.2925422906609));
#35935=CARTESIAN_POINT('Ctrl Pts',(60.2331453072406,-6.64074557868628,3.15607073054002));
#35936=CARTESIAN_POINT('Ctrl Pts',(60.4316569116826,-6.25435035863348,-3.86566758639099));
#35937=CARTESIAN_POINT('Ctrl Pts',(60.6301685161248,-0.133209051532416,
-7.35154703498433));
#35938=CARTESIAN_POINT('Ctrl Pts',(60.7955948531599,5.0470729870606,-4.64232161300714));
#35939=CARTESIAN_POINT('Ctrl Pts',(60.9279359227879,6.44398673196168,-0.597808483107745));
#35940=CARTESIAN_POINT('Ctrl Pts',(61.027191725009,5.96323825064499,2.56193749594574));
#35941=CARTESIAN_POINT('Ctrl Pts',(61.12644752723,4.00221625291053,5.08572561677413));
#35942=CARTESIAN_POINT('Ctrl Pts',(61.2587885968582,0.106894138300333,6.85657854461737));
#35943=CARTESIAN_POINT('Ctrl Pts',(61.4242149338931,-5.42421789290193,4.96395494634262));
#35944=CARTESIAN_POINT('Ctrl Pts',(61.6227265383354,-7.10930503660753,-1.87565087195877));
#35945=CARTESIAN_POINT('Ctrl Pts',(61.8212381427774,-2.28199696173699,-6.98947595772644));
#35946=CARTESIAN_POINT('Ctrl Pts',(62.0197497472196,4.64330776244168,-5.70111230219558));
#35947=CARTESIAN_POINT('Ctrl Pts',(62.1851760842546,6.85135343285645,-0.288187149949455));
#35948=CARTESIAN_POINT('Ctrl Pts',(62.3175171538827,5.30779068198273,3.70266094321786));
#35949=CARTESIAN_POINT('Ctrl Pts',(62.4167729561038,2.90113679133094,5.80578500162336));
#35950=CARTESIAN_POINT('Ctrl Pts',(62.5160287583248,-0.225675472877136,
6.46772066226701));
#35951=CARTESIAN_POINT('Ctrl Pts',(62.6483698279529,-4.34392994578106,5.30606900835795));
#35952=CARTESIAN_POINT('Ctrl Pts',(62.813796164988,-7.34701589818293,0.29042357143327));
#35953=CARTESIAN_POINT('Ctrl Pts',(63.0123077694301,-4.21946930612633,-6.02132569054943));
#35954=CARTESIAN_POINT('Ctrl Pts',(63.2108193738721,2.7683587964008,-6.81149571470196));
#35955=CARTESIAN_POINT('Ctrl Pts',(63.4093309783144,7.22635244835865,-1.35750460444815));
#35956=CARTESIAN_POINT('Ctrl Pts',(63.5747573153493,5.41909355797858,4.20208528057022));
#35957=CARTESIAN_POINT('Ctrl Pts',(63.7070983849776,1.66422455917251,6.25401443880813));
#35958=CARTESIAN_POINT('Ctrl Pts',(63.8063541871984,-1.53144515668549,6.30701275558833));
#35959=CARTESIAN_POINT('Ctrl Pts',(63.9056099894197,-4.34695939124221,4.79440132186115));
#35960=CARTESIAN_POINT('Ctrl Pts',(64.0379510590476,-6.74270627645356,1.24900270807729));
#35961=CARTESIAN_POINT('Ctrl Pts',(64.2033773960828,-5.79912545859896,-4.52030224370326));
#35962=CARTESIAN_POINT('Ctrl Pts',(64.4018890005248,0.663619680803454,-7.32256056419159));
#35963=CARTESIAN_POINT('Ctrl Pts',(64.600400604967,6.5109576340338,-3.4158037099402));
#35964=CARTESIAN_POINT('Ctrl Pts',(64.798912209409,6.39570941553163,3.62738053298608));
#35965=CARTESIAN_POINT('Ctrl Pts',(64.9643385464442,1.42688476588627,6.70731656925046));
#35966=CARTESIAN_POINT('Ctrl Pts',(65.0966796160723,-2.76551176215596,5.8510071507069));
#35967=CARTESIAN_POINT('Ctrl Pts',(65.1959354182932,-5.24058113930113,3.82884362299698));
#35968=CARTESIAN_POINT('Ctrl Pts',(65.2951912205144,-6.4147644634311,0.856234116925767));
#35969=CARTESIAN_POINT('Ctrl Pts',(65.4275322901425,-5.95626658402133,-3.39808535436641));
#35970=CARTESIAN_POINT('Ctrl Pts',(65.5929586271775,-1.51176119750446,-7.19566303681453));
#35971=CARTESIAN_POINT('Ctrl Pts',(65.7914702316198,5.23321851206271,-5.16465955355726));
#35972=CARTESIAN_POINT('Ctrl Pts',(65.9899818360617,7.17781718660405,1.59349450345578));
#35973=CARTESIAN_POINT('Ctrl Pts',(66.1884934405039,2.54376969957746,6.89871177591126));
#35974=CARTESIAN_POINT('Ctrl Pts',(66.353919777539,-3.23937625907777,6.04404973191034));
#35975=CARTESIAN_POINT('Ctrl Pts',(66.486260847167,-5.88883608535315,2.68401742388717));
#35976=CARTESIAN_POINT('Ctrl Pts',(66.5855166493881,-6.47409645489935,-0.45804941602601));
#35977=CARTESIAN_POINT('Ctrl Pts',(66.6847724516092,-5.45227135475848,-3.4864132116906));
#35978=CARTESIAN_POINT('Ctrl Pts',(66.8171135212372,-2.35612050115225,-6.43993724590316));
#35979=CARTESIAN_POINT('Ctrl Pts',(66.9825398582723,3.48975044558929,-6.47183364038364));
#35980=CARTESIAN_POINT('Ctrl Pts',(67.1810514627144,7.33067472739079,-0.567002756194563));
#35981=CARTESIAN_POINT('Ctrl Pts',(67.3795630671566,4.45391682219975,5.85003491379102));
#35982=CARTESIAN_POINT('Ctrl Pts',(67.5780746715986,-2.50983236811194,6.91113104420389));
#35983=CARTESIAN_POINT('Ctrl Pts',(67.7435010086337,-6.37537432645889,2.5256079652503));
#35984=CARTESIAN_POINT('Ctrl Pts',(67.8758420782619,-6.23030789835879,-1.75088645287108));
#35985=CARTESIAN_POINT('Ctrl Pts',(67.9750978804828,-4.64928527757637,-4.52856336585343));
#35986=CARTESIAN_POINT('Ctrl Pts',(68.074353682704,-1.91415673077897,-6.18209724638608));
#35987=CARTESIAN_POINT('Ctrl Pts',(68.2066947523319,2.35704435361657,-6.43960284826646));
#35988=CARTESIAN_POINT('Ctrl Pts',(68.3721210893672,6.84272208387396,-2.69074004151496));
#35989=CARTESIAN_POINT('Ctrl Pts',(68.5706326938092,5.96516493496265,4.29849148457416));
#35990=CARTESIAN_POINT('Ctrl Pts',(68.7691442982513,-0.373993920311934,
7.34307320266848));
#35991=CARTESIAN_POINT('Ctrl Pts',(68.9676559026935,-6.37779317569966,3.65872989786245));
#35992=CARTESIAN_POINT('Ctrl Pts',(69.1330822397285,-6.49970078748444,-2.18584368611994));
#35993=CARTESIAN_POINT('Ctrl Pts',(69.2654233093567,-3.62859134903107,-5.35878348065247));
#35994=CARTESIAN_POINT('Ctrl Pts',(69.3646791115776,-0.62823592000139,-6.45958714174554));
#35995=CARTESIAN_POINT('Ctrl Pts',(69.4639349137987,2.52830110610206,-5.95780469931484));
#35996=CARTESIAN_POINT('Ctrl Pts',(69.5962759834268,5.95652483419779,-3.3963489535312));
#35997=CARTESIAN_POINT('Ctrl Pts',(69.7617023204619,6.96369965258984,2.35963460035952));
#35998=CARTESIAN_POINT('Ctrl Pts',(69.9602139249039,1.78096623639146,7.13640802565527));
#35999=CARTESIAN_POINT('Ctrl Pts',(70.1587255293462,-5.02380608586829,5.3617905732631));
#36000=CARTESIAN_POINT('Ctrl Pts',(70.3572371337882,-7.23566990141503,-1.31149301022891));
#36001=CARTESIAN_POINT('Ctrl Pts',(70.5557487382304,-2.81181884640884,-6.79534921779986));
#36002=CARTESIAN_POINT('Ctrl Pts',(70.7211750752654,3.00649289900833,-6.16512333542295));
#36003=CARTESIAN_POINT('Ctrl Pts',(70.8535161448936,5.77263950695759,-2.91134114312552));
#36004=CARTESIAN_POINT('Ctrl Pts',(70.9858572145215,6.74314937401964,1.2444879873417));
#36005=CARTESIAN_POINT('Ctrl Pts',(71.1512835515567,3.79854938863639,6.30172191780343));
#36006=CARTESIAN_POINT('Ctrl Pts',(71.3497951559988,-3.25302923561936,6.59577169661227));
#36007=CARTESIAN_POINT('Ctrl Pts',(71.5152214930338,-6.6101259714308,1.81625507702285));
#36008=CARTESIAN_POINT('Ctrl Pts',(71.647562562662,-6.00358031277986,-2.41949711668263));
#36009=CARTESIAN_POINT('Ctrl Pts',(71.7468183648829,-4.12753807040063,-5.00810542026236));
#36010=CARTESIAN_POINT('Ctrl Pts',(71.8460741671042,-1.22942858196295,-6.35390206362266));
#36011=CARTESIAN_POINT('Ctrl Pts',(71.978415236732,3.04488676341186,-6.14439894507291));
#36012=CARTESIAN_POINT('Ctrl Pts',(72.1438415737674,7.09505541724423,-1.92914383180871));
#36013=CARTESIAN_POINT('Ctrl Pts',(72.3423531782092,5.46132883333844,4.92289529580099));
#36014=CARTESIAN_POINT('Ctrl Pts',(72.5408647826516,-1.17190946057312,7.25857562521031));
#36015=CARTESIAN_POINT('Ctrl Pts',(72.7393763870934,-6.73847855351414,2.94204908409314));
#36016=CARTESIAN_POINT('Ctrl Pts',(72.9048027241288,-6.22280912928604,-2.88112258378322));
#36017=CARTESIAN_POINT('Ctrl Pts',(73.0371437937567,-3.02311377228348,-5.72215776666869));
#36018=CARTESIAN_POINT('Ctrl Pts',(73.1363995959778,0.0794348410866285,
-6.48979416820313));
#36019=CARTESIAN_POINT('Ctrl Pts',(73.2356553981989,3.16227467098884,-5.6464470206576));
#36020=CARTESIAN_POINT('Ctrl Pts',(73.367996467827,6.29145571547599,-2.72794273270417));
#36021=CARTESIAN_POINT('Ctrl Pts',(73.533422804862,6.66446686956165,3.10610303551645));
#36022=CARTESIAN_POINT('Ctrl Pts',(73.7319344093041,0.993858002836962,7.28508954315968));
#36023=CARTESIAN_POINT('Ctrl Pts',(73.9304460137462,-5.58013110682443,4.78773641119374));
#36024=CARTESIAN_POINT('Ctrl Pts',(74.1289576181884,-7.04582651485609,-2.10221746089843));
#36025=CARTESIAN_POINT('Ctrl Pts',(74.2943839552234,-2.89337352700839,-6.21711227638719));
#36026=CARTESIAN_POINT('Ctrl Pts',(74.4267250248515,1.38429868618496,-6.32187133024273));
#36027=CARTESIAN_POINT('Ctrl Pts',(74.5259808270725,4.24950930786462,-4.9056503007122));
#36028=CARTESIAN_POINT('Ctrl Pts',(74.6252366292937,6.05985073959253,-2.27168416620927));
#36029=CARTESIAN_POINT('Ctrl Pts',(74.7575776989216,6.5661819132465,1.9772078337143));
#36030=CARTESIAN_POINT('Ctrl Pts',(74.9230040359569,3.08550547279318,6.67402760129288));
#36031=CARTESIAN_POINT('Ctrl Pts',(75.1215156403989,-3.94304652828918,6.20585758518567));
#36032=CARTESIAN_POINT('Ctrl Pts',(75.3200272448411,-7.35236275094442,0.0551931363052712));
#36033=CARTESIAN_POINT('Ctrl Pts',(75.5185388492831,-4.02474686326202,-6.15340565402118));
#36034=CARTESIAN_POINT('Ctrl Pts',(75.6839651863182,1.80286576781962,-6.61617493105383));
#36035=CARTESIAN_POINT('Ctrl Pts',(75.8163062559463,5.13778071835795,-3.93516826512113));
#36036=CARTESIAN_POINT('Ctrl Pts',(75.9155620581673,6.41213741680385,-1.0041055296563));
#36037=CARTESIAN_POINT('Ctrl Pts',(76.0148178603885,6.09478893729921,2.1762095014379));
#36038=CARTESIAN_POINT('Ctrl Pts',(76.1471589300164,3.73908041305424,5.74833657329857));
#36039=CARTESIAN_POINT('Ctrl Pts',(76.3125852670516,-1.95103068448381,7.08917962300208));
#36040=CARTESIAN_POINT('Ctrl Pts',(76.5110968714937,-7.01727857255056,2.19501383418843));
#36041=CARTESIAN_POINT('Ctrl Pts',(76.7096084759358,-5.65138000548379,-4.70342304397645));
#36042=CARTESIAN_POINT('Ctrl Pts',(76.9081200803781,0.897600199059924,-7.29776009071585));
#36043=CARTESIAN_POINT('Ctrl Pts',(77.0735464174129,5.64744158313445,-3.88979424396703));
#36044=CARTESIAN_POINT('Ctrl Pts',(77.2058874870412,6.46420439911098,0.31048586229469));
#36045=CARTESIAN_POINT('Ctrl Pts',(77.3051432892621,5.54570835728657,3.37177297323113));
#36046=CARTESIAN_POINT('Ctrl Pts',(77.4043990914832,3.2505835667813,5.59607420068252));
#36047=CARTESIAN_POINT('Ctrl Pts',(77.5367401611112,-0.854341364942577,
6.80398387178119));
#36048=CARTESIAN_POINT('Ctrl Pts',(77.7021664981465,-6.06591106563178,4.15544358677189));
#36049=CARTESIAN_POINT('Ctrl Pts',(77.9006781025884,-6.7765882047847,-2.85274194412771));
#36050=CARTESIAN_POINT('Ctrl Pts',(78.0991897070306,-1.28071754910471,-7.24016897982555));
#36051=CARTESIAN_POINT('Ctrl Pts',(78.2977013114727,5.39592604241165,-4.99469424527876));
#36052=CARTESIAN_POINT('Ctrl Pts',(78.4631276485078,6.82419817520737,0.674103078769445));
#36053=CARTESIAN_POINT('Ctrl Pts',(78.5954687181358,4.73697475670672,4.40946823761063));
#36054=CARTESIAN_POINT('Ctrl Pts',(78.6947245203569,2.0595182708145,6.1548451369039));
#36055=CARTESIAN_POINT('Ctrl Pts',(78.793980322578,-1.12917895789654,6.37238533558803));
#36056=CARTESIAN_POINT('Ctrl Pts',(78.9263213922061,-5.04417715043781,4.64546796031478));
#36057=CARTESIAN_POINT('Ctrl Pts',(79.091747729241,-7.31528962469706,-0.741300320920373));
#36058=CARTESIAN_POINT('Ctrl Pts',(79.2902593336834,-3.33467618405536,-6.55287868379289));
#36059=CARTESIAN_POINT('Ctrl Pts',(79.4887709381253,3.69494857957145,-6.35670034619658));
#36060=CARTESIAN_POINT('Ctrl Pts',(79.6872825425675,7.34524717088535,-0.332163299594867));
#36061=CARTESIAN_POINT('Ctrl Pts',(79.8527088796025,4.77724243558189,4.91955794833087));
#36062=CARTESIAN_POINT('Ctrl Pts',(79.9850499492307,0.772025231896089,6.42544294391362));
#36063=CARTESIAN_POINT('Ctrl Pts',(80.0843057514517,-2.39957651105506,6.03040353000374));
#36064=CARTESIAN_POINT('Ctrl Pts',(80.1835615536727,-4.97552377725469,4.13841794966956));
#36065=CARTESIAN_POINT('Ctrl Pts',(80.3159026233009,-6.85117239325693,0.292459455625172));
#36066=CARTESIAN_POINT('Ctrl Pts',(80.4813289603358,-5.10896704970656,-5.28785818115516));
#36067=CARTESIAN_POINT('Ctrl Pts',(80.6798405647781,1.68251786406567,-7.15747287344582));
#36068=CARTESIAN_POINT('Ctrl Pts',(80.8783521692202,6.92514205415142,-2.4703626913545));
#36069=CARTESIAN_POINT('Ctrl Pts',(81.0768637736622,5.82471539119074,4.48727969605447));
#36070=CARTESIAN_POINT('Ctrl Pts',(81.2422901106974,0.473544591506288,6.84104167617517));
#36071=CARTESIAN_POINT('Ctrl Pts',(81.3746311803253,-3.55762461323784,5.40607501755736));
#36072=CARTESIAN_POINT('Ctrl Pts',(81.4738869825466,-5.72512502258832,3.05723365852555));
#36073=CARTESIAN_POINT('Ctrl Pts',(81.5731427847674,-6.47145951622151,-0.0505144937619511));
#36074=CARTESIAN_POINT('Ctrl Pts',(81.7054838543957,-5.42171283747731,-4.19870522938243));
#36075=CARTESIAN_POINT('Ctrl Pts',(81.8709101914306,-0.48919755281723,-7.33646196836831));
#36076=CARTESIAN_POINT('Ctrl Pts',(82.069421795873,5.90490006067872,-4.38091766304837));
#36077=CARTESIAN_POINT('Ctrl Pts',(82.2679334003147,6.88393788382687,2.58296022203711));
#36078=CARTESIAN_POINT('Ctrl Pts',(82.4664450047572,1.55262125162276,7.18695733311437));
#36079=CARTESIAN_POINT('Ctrl Pts',(82.6318713417919,-4.05385301920155,5.53085629844241));
#36080=CARTESIAN_POINT('Ctrl Pts',(82.7642124114203,-6.20667286345935,1.83290805829735));
#36081=CARTESIAN_POINT('Ctrl Pts',(82.8634682136412,-6.34615709688077,-1.36015597223205));
#36082=CARTESIAN_POINT('Ctrl Pts',(82.9627240158624,-4.91031465598665,-4.2155841781865));
#36083=CARTESIAN_POINT('Ctrl Pts',(83.0950650854904,-1.43106703177257,-6.70642548947526));
#36084=CARTESIAN_POINT('Ctrl Pts',(83.2604914225255,4.36166608043273,-5.91936292702175));
#36085=CARTESIAN_POINT('Ctrl Pts',(83.4590030269676,7.33784111646791,0.465158087628112));
#36086=CARTESIAN_POINT('Ctrl Pts',(83.6575146314097,3.59080068386597,6.41610744499814));
#36087=CARTESIAN_POINT('Ctrl Pts',(83.8560262358518,-3.45292231992367,6.49155727938758));
#36088=CARTESIAN_POINT('Ctrl Pts',(84.0214525728869,-6.66623356367417,1.60792592175586));
#36089=CARTESIAN_POINT('Ctrl Pts',(84.1537936425151,-5.92372422041267,-2.6061142232585));
#36090=CARTESIAN_POINT('Ctrl Pts',(84.253049444736,-3.96930072085848,-5.13501567227216));
#36091=CARTESIAN_POINT('Ctrl Pts',(84.3523052469571,-1.02956513266701,-6.38923591846239));
#36092=CARTESIAN_POINT('Ctrl Pts',(84.4846463165852,3.23560668510475,-6.04606856350603));
#36093=CARTESIAN_POINT('Ctrl Pts',(84.6500726536202,7.15210351133029,-1.70599056920427));
#36094=CARTESIAN_POINT('Ctrl Pts',(84.8485842580625,5.30442784199376,5.09149580831549));
#36095=CARTESIAN_POINT('Ctrl Pts',(85.0470958625043,-1.39861029772509,7.21832207179135));
#36096=CARTESIAN_POINT('Ctrl Pts',(85.2456074669468,-6.82732506329547,2.72958255766234));
#36097=CARTESIAN_POINT('Ctrl Pts',(85.4110338039816,-6.12952335880773,-3.07457949793802));
#36098=CARTESIAN_POINT('Ctrl Pts',(85.5433748736098,-2.84244201074919,-5.8140229961449));
#36099=CARTESIAN_POINT('Ctrl Pts',(85.6426306758308,0.282630697465553,-6.48412322954603));
#36100=CARTESIAN_POINT('Ctrl Pts',(85.7418864780519,3.3375450925625,-5.54464901858413));
#36101=CARTESIAN_POINT('Ctrl Pts',(85.8742275476799,6.37379824136797,-2.52958330039638));
#36102=CARTESIAN_POINT('Ctrl Pts',(86.0396538847151,6.56392799824454,3.313282012274));
#36103=CARTESIAN_POINT('Ctrl Pts',(86.2381654891571,0.765233081136916,7.31263992198074));
#36104=CARTESIAN_POINT('Ctrl Pts',(86.4366770935993,-5.72732574435958,4.61064248397214));
#36105=CARTESIAN_POINT('Ctrl Pts',(86.6351886980413,-6.97653835085342,-2.321831410346));
#36106=CARTESIAN_POINT('Ctrl Pts',(86.8006150350767,-2.69726124705009,-6.30467108265544));
#36107=CARTESIAN_POINT('Ctrl Pts',(86.9329561047044,1.58159360772959,-6.2754204356491));
#36108=CARTESIAN_POINT('Ctrl Pts',(87.0322119069257,4.40104898481893,-4.77016792160538));
#36109=CARTESIAN_POINT('Ctrl Pts',(87.1314677091467,6.1280180343697,-2.08080151735183));
#36110=CARTESIAN_POINT('Ctrl Pts',(87.2638087787747,6.501043828168,2.18186269951808));
#36111=CARTESIAN_POINT('Ctrl Pts',(87.4292351158099,2.87499030196175,6.76737905120017));
#36112=CARTESIAN_POINT('Ctrl Pts',(87.6277467202519,-4.1354534267282,6.07933460605474));
#36113=CARTESIAN_POINT('Ctrl Pts',(87.8262583246941,-7.35048514532909,-0.175078340491695));
#36114=CARTESIAN_POINT('Ctrl Pts',(88.0247699291361,-3.8300746758159,-6.27642545057859));
#36115=CARTESIAN_POINT('Ctrl Pts',(88.1901962661713,2.00917170803365,-6.55647197377879));
#36116=CARTESIAN_POINT('Ctrl Pts',(88.3225373357994,5.25849341829804,-3.77234502052638));
#36117=CARTESIAN_POINT('Ctrl Pts',(88.4217931380204,6.44043681020296,-0.802812469304661));
#36118=CARTESIAN_POINT('Ctrl Pts',(88.5210489402415,6.02365017597241,2.36600476366407));
#36119=CARTESIAN_POINT('Ctrl Pts',(88.6533900098694,3.55723335538306,5.86260919306929));
#36120=CARTESIAN_POINT('Ctrl Pts',(88.8188163469047,-2.17207643043537,7.02460478883646));
#36121=CARTESIAN_POINT('Ctrl Pts',(89.0173279513466,-7.08257530082506,1.974186264048));
#36122=CARTESIAN_POINT('Ctrl Pts',(89.2158395557889,-5.50131724885063,-4.87809315455458));
#36123=CARTESIAN_POINT('Ctrl Pts',(89.4143511602309,1.12569445119592,-7.26607187285839));
#36124=CARTESIAN_POINT('Ctrl Pts',(89.5797774972661,5.76648339708804,-3.71103286517617));
#36125=CARTESIAN_POINT('Ctrl Pts',(89.7121185668941,6.45131090248977,0.512764686372355));
#36126=CARTESIAN_POINT('Ctrl Pts',(89.8113743691151,5.43739898593206,3.54378701883646));
#36127=CARTESIAN_POINT('Ctrl Pts',(89.9106301713363,3.07374429895899,5.69512387650968));
#36128=CARTESIAN_POINT('Ctrl Pts',(90.0429712409643,-1.06699388433329,6.77389251066956));
#36129=CARTESIAN_POINT('Ctrl Pts',(90.2083975779993,-6.19306663421924,3.96344725247069));
#36130=CARTESIAN_POINT('Ctrl Pts',(90.4069091824416,-6.68392896138932,-3.06355641960676));
#36131=CARTESIAN_POINT('Ctrl Pts',(90.6054207868836,-1.05335843212328,-7.27672455920159));
#36132=CARTESIAN_POINT('Ctrl Pts',(90.8039323913257,5.54969193399755,-4.82326734659396));
#36133=CARTESIAN_POINT('Ctrl Pts',(90.9693587283609,6.79974118846012,0.887477022389232));
#36134=CARTESIAN_POINT('Ctrl Pts',(91.1016997979888,4.59656587779412,4.55564727731113));
#36135=CARTESIAN_POINT('Ctrl Pts',(91.20095560021,1.86576486459037,6.21632171280966));
#36136=CARTESIAN_POINT('Ctrl Pts',(91.300211402431,-1.32818086979205,6.33389892256676));
#36137=CARTESIAN_POINT('Ctrl Pts',(91.432552472059,-5.18717929313224,4.48522760584228));
#36138=CARTESIAN_POINT('Ctrl Pts',(91.5979788090943,-7.28848744989553,-0.970020181085168));
#36139=CARTESIAN_POINT('Ctrl Pts',(91.7964904135362,-3.12783266756751,-6.6540925076761));
#36140=CARTESIAN_POINT('Ctrl Pts',(91.9950020179784,3.89220090559598,-6.23787274697798));
#36141=CARTESIAN_POINT('Ctrl Pts',(92.1935136224206,7.35204657094004,-0.101978810180762));
#36142=CARTESIAN_POINT('Ctrl Pts',(92.3589399594556,4.62083998930958,5.06674782168087));
#36143=CARTESIAN_POINT('Ctrl Pts',(92.4912810290838,0.570429324999648,6.44646805385352));
#36144=CARTESIAN_POINT('Ctrl Pts',(92.5905368313047,-2.58724594711247,5.9523014520636));
#36145=CARTESIAN_POINT('Ctrl Pts',(92.6897926335258,-5.10268096401501,3.98057621000437));
#36146=CARTESIAN_POINT('Ctrl Pts',(92.8221337031539,-6.85697076191429,0.0777667381484085));
#36147=CARTESIAN_POINT('Ctrl Pts',(92.9875600401889,-4.9408683261657,-5.44525560855407));
#36148=CARTESIAN_POINT('Ctrl Pts',(93.1860716446312,1.90583395511156,-7.10127321207659));
#36149=CARTESIAN_POINT('Ctrl Pts',(93.3845832490731,6.99910671440612,-2.25228539429799));
#36150=CARTESIAN_POINT('Ctrl Pts',(93.5830948535154,5.68133630187344,4.66748393505667));
#36151=CARTESIAN_POINT('Ctrl Pts',(93.7485211905503,0.259080310101639,6.85251582181516));
#36152=CARTESIAN_POINT('Ctrl Pts',(93.8808622601785,-3.72517479045193,5.29201405560826));
#36153=CARTESIAN_POINT('Ctrl Pts',(93.9801180623995,-5.81805651628024,2.87644790331024));
#36154=CARTESIAN_POINT('Ctrl Pts',(94.0793738646206,-6.46670364739967,-0.253148021681272));
#36155=CARTESIAN_POINT('Ctrl Pts',(94.2117149342486,-5.2875683157848,-4.36643069350914));
#36156=CARTESIAN_POINT('Ctrl Pts',(94.3771412712839,-0.259211159662201,
-7.34818331519461));
#36157=CARTESIAN_POINT('Ctrl Pts',(94.5756528757259,6.03919547739302,-4.19385291621541));
#36158=CARTESIAN_POINT('Ctrl Pts',(94.7741644801679,6.79967439427966,2.79726874447026));
#36159=CARTESIAN_POINT('Ctrl Pts',(94.9726760846102,1.32679513771092,7.23205386605656));
#36160=CARTESIAN_POINT('Ctrl Pts',(95.1381024216451,-4.22506743128341,5.40119439535534));
#36161=CARTESIAN_POINT('Ctrl Pts',(95.2704434912733,-6.26102756202529,1.63764277293116));
#36162=CARTESIAN_POINT('Ctrl Pts',(95.3696992934943,-6.30045034013798,-1.55822324412883));
#36163=CARTESIAN_POINT('Ctrl Pts',(95.4689550957154,-4.77589237691392,-4.36728657043583));
#36164=CARTESIAN_POINT('Ctrl Pts',(95.6012961653434,-1.22034872738306,-6.74795114674706));
#36165=CARTESIAN_POINT('Ctrl Pts',(95.7667225023786,4.544895881605,-5.77987109582617));
#36166=CARTESIAN_POINT('Ctrl Pts',(95.9652341068206,7.31967546924895,0.694719599470295));
#36167=CARTESIAN_POINT('Ctrl Pts',(96.1637457112627,3.388114636821,6.52540906800271));
#36168=CARTESIAN_POINT('Ctrl Pts',(96.3622573157049,-3.65451648904094,6.38024276108088));
#36169=CARTESIAN_POINT('Ctrl Pts',(96.5276836527399,-6.71331739379509,1.39837951410866));
#36170=CARTESIAN_POINT('Ctrl Pts',(96.6600247223681,-5.83920659045662,-2.79034162391308));
#36171=CARTESIAN_POINT('Ctrl Pts',(96.7592805245889,-3.80654732511578,-5.25679861025155));
#36172=CARTESIAN_POINT('Ctrl Pts',(96.8585363268103,-0.828976761999734,
-6.41834382938761));
#36173=CARTESIAN_POINT('Ctrl Pts',(96.990877396438,3.4233566459321,-5.94177793005278));
#36174=CARTESIAN_POINT('Ctrl Pts',(97.1563037334735,7.20202000654271,-1.48118070617854));
#36175=CARTESIAN_POINT('Ctrl Pts',(97.3548153379154,5.14238247907462,5.25511053508099));
#36176=CARTESIAN_POINT('Ctrl Pts',(97.5533269423575,-1.62397116860792,7.17098333149248));
#36177=CARTESIAN_POINT('Ctrl Pts',(97.7518385467997,-6.90945535086944,2.51444133225228));
#36178=CARTESIAN_POINT('Ctrl Pts',(97.9172648838347,-6.03023447391599,-3.26502188122914));
#36179=CARTESIAN_POINT('Ctrl Pts',(98.0496059534629,-2.65897769905643,-5.90018453779998));
#36180=CARTESIAN_POINT('Ctrl Pts',(98.1488617556838,0.485546955475345,-6.47209226766101));
#36181=CARTESIAN_POINT('Ctrl Pts',(98.2481175579051,3.50954275153179,-5.43741203692939));
#36182=CARTESIAN_POINT('Ctrl Pts',(98.3804586275328,6.44988784699202,-2.32874267718317));
#36183=CARTESIAN_POINT('Ctrl Pts',(98.5458849645682,6.45695091959748,3.51721100886858));
#36184=CARTESIAN_POINT('Ctrl Pts',(98.7443965690102,0.535857308578908,7.33301719906992));
#36185=CARTESIAN_POINT('Ctrl Pts',(98.9429081734524,-5.8689022478471,4.42902593153709));
#36186=CARTESIAN_POINT('Ctrl Pts',(99.1414197778944,-6.90040687703648,-2.5391678539131));
#36187=CARTESIAN_POINT('Ctrl Pts',(99.3068461149296,-2.49850315059143,-6.3860455449202));
#36188=CARTESIAN_POINT('Ctrl Pts',(99.4391871845576,1.77733710574879,-6.22281389700046));
#36189=CARTESIAN_POINT('Ctrl Pts',(99.5384429867787,4.54827162108827,-4.63000641769442));
#36190=CARTESIAN_POINT('Ctrl Pts',(99.6376987889997,6.19017426763678,-1.8878777821833));
#36191=CARTESIAN_POINT('Ctrl Pts',(99.7700398586277,6.4295287824728,2.38437734653381));
#36192=CARTESIAN_POINT('Ctrl Pts',(99.9354661956629,2.66165501182151,6.85409228541916));
#36193=CARTESIAN_POINT('Ctrl Pts',(100.133977800105,-4.32380380101862,5.94684832388633));
#36194=CARTESIAN_POINT('Ctrl Pts',(100.332489404547,-7.34139734791796,-0.405178080596634));
#36195=CARTESIAN_POINT('Ctrl Pts',(100.531001008989,-3.63164551501983,-6.39328861480798));
#36196=CARTESIAN_POINT('Ctrl Pts',(100.696427346024,2.21350682387351,-6.49033768273847));
#36197=CARTESIAN_POINT('Ctrl Pts',(100.828768415652,5.37404798958258,-3.60582143066423));
#36198=CARTESIAN_POINT('Ctrl Pts',(100.928024217873,6.46241869027549,-0.600731919134315));
#36199=CARTESIAN_POINT('Ctrl Pts',(101.027280020095,5.94660273312621,2.55347917918856));
#36200=CARTESIAN_POINT('Ctrl Pts',(101.159621089723,3.3718969584413,5.97113109862479));
#36201=CARTESIAN_POINT('Ctrl Pts',(101.325047426758,-2.39099155665315,6.95313942295208));
#36202=CARTESIAN_POINT('Ctrl Pts',(101.5235590312,-7.1409246333084,1.75142218737291));
#36203=CARTESIAN_POINT('Ctrl Pts',(101.722070635642,-5.34585817425296,-5.04797827627917));
#36204=CARTESIAN_POINT('Ctrl Pts',(101.920582240084,1.3526844941182,-7.22725626488847));
#36205=CARTESIAN_POINT('Ctrl Pts',(102.086008577119,5.87986878794746,-3.52863128306579));
#36206=CARTESIAN_POINT('Ctrl Pts',(102.218349646747,6.43208922602856,0.714540532497019));
#36207=CARTESIAN_POINT('Ctrl Pts',(102.317605448968,5.32375599492072,3.71232491487952));
#36208=CARTESIAN_POINT('Ctrl Pts',(102.416861251189,2.89388995296144,5.78858712677963));
#36209=CARTESIAN_POINT('Ctrl Pts',(102.549202320817,-1.27859977470671,6.73715654497048));
#36210=CARTESIAN_POINT('Ctrl Pts',(102.714628657853,-6.31414733833159,3.76756311809497));
#36211=CARTESIAN_POINT('Ctrl Pts',(102.913140262295,-6.58471335989169,-3.27136581033968));
#36212=CARTESIAN_POINT('Ctrl Pts',(103.111651866737,-0.82496606132839,-7.30614229910194));
#36213=CARTESIAN_POINT('Ctrl Pts',(103.310163471179,5.69801405622591,-4.64710923843941));
#36214=CARTESIAN_POINT('Ctrl Pts',(103.475589808214,6.76861424179842,1.09998042754471));
#36215=CARTESIAN_POINT('Ctrl Pts',(103.607930877842,4.45164816401902,4.69735761978553));
#36216=CARTESIAN_POINT('Ctrl Pts',(103.707186680063,1.67018130387269,6.27170061297181));
#36217=CARTESIAN_POINT('Ctrl Pts',(103.806442482284,-1.52587995074471,6.2891995008118));
#36218=CARTESIAN_POINT('Ctrl Pts',(103.938783551912,-5.32509326013816,4.32058762958816));
#36219=CARTESIAN_POINT('Ctrl Pts',(104.104209888947,-7.2545358971902,-1.19778853474281));
#36220=CARTESIAN_POINT('Ctrl Pts',(104.302721493389,-2.91792101694804,-6.7487792410007));
#36221=CARTESIAN_POINT('Ctrl Pts',(104.501233097831,4.08563531820164,-6.11292633132952));
#36222=CARTESIAN_POINT('Ctrl Pts',(104.699744702274,7.35163424685847,0.128305709641857));
#36223=CARTESIAN_POINT('Ctrl Pts',(104.865171039309,4.4599048978128,5.20896765575043));
#36224=CARTESIAN_POINT('Ctrl Pts',(104.997512108937,0.368273875481132,6.4611697294255));
#36225=CARTESIAN_POINT('Ctrl Pts',(105.096767911158,-2.77237751656084,5.86836069033733));
#36226=CARTESIAN_POINT('Ctrl Pts',(105.196023713379,-5.22483286318278,3.81882984829934));
#36227=CARTESIAN_POINT('Ctrl Pts',(105.328364783007,-6.85604302789201,-0.137002218719652));
#36228=CARTESIAN_POINT('Ctrl Pts',(105.493791120042,-4.76792304793109,-5.59731179744855));
#36229=CARTESIAN_POINT('Ctrl Pts',(105.692302724484,2.12728060596421,-7.03810766777042));
#36230=CARTESIAN_POINT('Ctrl Pts',(105.890814328926,7.06620582008108,-2.03199906838922));
#36231=CARTESIAN_POINT('Ctrl Pts',(106.089325933368,5.53238437901881,4.84311030515874));
#36232=CARTESIAN_POINT('Ctrl Pts',(106.254752270403,0.0443617744349961,
6.85726730780797));
#36233=CARTESIAN_POINT('Ctrl Pts',(106.387093340032,-3.88907072626489,5.1727633873222));
#36234=CARTESIAN_POINT('Ctrl Pts',(106.486349142253,-5.90528136083011,2.69283775413386));
#36235=CARTESIAN_POINT('Ctrl Pts',(106.585604944474,-6.4556038302783,-0.455527979344725));
#36236=CARTESIAN_POINT('Ctrl Pts',(106.717946014101,-5.14823859197666,-4.5298844173743));
#36237=CARTESIAN_POINT('Ctrl Pts',(106.883372351137,-0.0289675534008062,
-7.35267358327051));
#36238=CARTESIAN_POINT('Ctrl Pts',(107.081883955579,6.1675620574163,-4.00271286495399));
#36239=CARTESIAN_POINT('Ctrl Pts',(107.280395560021,6.70875004256005,3.00890426696354));
#36240=CARTESIAN_POINT('Ctrl Pts',(107.478907164463,1.09964973772579,7.26991658020799));
#36241=CARTESIAN_POINT('Ctrl Pts',(107.644333501498,-4.39210610522649,5.26648010085043));
#36242=CARTESIAN_POINT('Ctrl Pts',(107.776674571126,-6.30928449663211,1.44042764539869));
#36243=CARTESIAN_POINT('Ctrl Pts',(107.875930373347,-6.2484678151464,-1.75401181099146));
#36244=CARTESIAN_POINT('Ctrl Pts',(107.975186175568,-4.63696157612732,-4.51609008620458));
#36245=CARTESIAN_POINT('Ctrl Pts',(108.107527245197,-1.00805461892616,-6.77986084607601));
#36246=CARTESIAN_POINT('Ctrl Pts',(108.272953582231,4.72291868063634,-5.64086832996922));
#36247=CARTESIAN_POINT('Ctrl Pts',(108.471465186674,7.29544819300465,0.934110138162679));
#36248=CARTESIAN_POINT('Ctrl Pts',(108.636891523709,3.86681832161873,5.66141617959935));
#36249=CARTESIAN_POINT('Ctrl Pts',(108.769232593337,-0.340764604699964,
6.46373036659584));
#36250=CARTESIAN_POINT('Ctrl Pts',(108.868488395558,-3.38799745293929,5.53147877557648));
#36251=CARTESIAN_POINT('Ctrl Pts',(108.967744197779,-5.62418538167471,3.22542302469746));
#36252=CARTESIAN_POINT('Ctrl Pts',(109.033914732593,-6.19447498791001,1.17358721206399));
#36253=CARTESIAN_POINT('Ctrl Pts',(109.067,-6.21768400249992,0.139557183822751));
#36254=CARTESIAN_POINT('Ctrl Pts',(30.7922774969106,0.678777225891756,-6.42139103611685));
#36255=CARTESIAN_POINT('Ctrl Pts',(30.8253627643176,1.74668468978894,-6.30850719805494));
#36256=CARTESIAN_POINT('Ctrl Pts',(30.8915332991316,3.82068840904174,-5.54208840511827));
#36257=CARTESIAN_POINT('Ctrl Pts',(30.9907891013527,6.01455579796589,-3.03012972641587));
#36258=CARTESIAN_POINT('Ctrl Pts',(31.0900449035738,6.71725437222838,0.202938760700514));
#36259=CARTESIAN_POINT('Ctrl Pts',(31.2223859732018,5.52548610707363,4.48753452027612));
#36260=CARTESIAN_POINT('Ctrl Pts',(31.387812310237,0.339508912956707,7.62882085876798));
#36261=CARTESIAN_POINT('Ctrl Pts',(31.586323914679,-6.24246999589781,4.40195999752177));
#36262=CARTESIAN_POINT('Ctrl Pts',(31.7517502517141,-6.92842770696881,-1.62572047208448));
#36263=CARTESIAN_POINT('Ctrl Pts',(31.8840913213422,-4.27423691538049,-5.18596025794933));
#36264=CARTESIAN_POINT('Ctrl Pts',(31.9833471235632,-1.27783695201738,-6.61598549330334));
#36265=CARTESIAN_POINT('Ctrl Pts',(32.0826029257843,2.03264953710899,-6.40436604028605));
#36266=CARTESIAN_POINT('Ctrl Pts',(32.2149439954124,5.82666197580389,-4.09184779202466));
#36267=CARTESIAN_POINT('Ctrl Pts',(32.3803703324475,7.42761210931129,1.76261098900636));
#36268=CARTESIAN_POINT('Ctrl Pts',(32.5788819368895,2.53670467138675,7.2000873154729));
#36269=CARTESIAN_POINT('Ctrl Pts',(32.7773935413318,-4.67164414538107,6.03751153344729));
#36270=CARTESIAN_POINT('Ctrl Pts',(32.9759051457738,-7.60525981750663,-0.661897697190728));
#36271=CARTESIAN_POINT('Ctrl Pts',(33.1413314828089,-4.24456811261457,-5.71615983348691));
#36272=CARTESIAN_POINT('Ctrl Pts',(33.273672552437,0.083495628675871,-6.7187092468208));
#36273=CARTESIAN_POINT('Ctrl Pts',(33.3729283546581,3.29378569679711,-5.87870906545261));
#36274=CARTESIAN_POINT('Ctrl Pts',(33.4721841568791,5.68646072766973,-3.57941580085851));
#36275=CARTESIAN_POINT('Ctrl Pts',(33.6045252265072,7.09134406091902,0.635248297090446));
#36276=CARTESIAN_POINT('Ctrl Pts',(33.7699515635422,4.53564490764562,6.14055242947785));
#36277=CARTESIAN_POINT('Ctrl Pts',(33.9684631679845,-2.70979707674458,7.13670357848515));
#36278=CARTESIAN_POINT('Ctrl Pts',(34.1669747724264,-7.46509976895978,1.59618946747842));
#36279=CARTESIAN_POINT('Ctrl Pts',(34.3654863768686,-5.38171243595097,-5.4143905431608));
#36280=CARTESIAN_POINT('Ctrl Pts',(34.5309127139037,0.447487280130549,-7.10566462936179));
#36281=CARTESIAN_POINT('Ctrl Pts',(34.6632537835318,4.40035911681068,-5.07788139373532));
#36282=CARTESIAN_POINT('Ctrl Pts',(34.7625095857528,6.31021524910873,-2.36419966135741));
#36283=CARTESIAN_POINT('Ctrl Pts',(34.8617653879739,6.65366662094855,0.936354830793845));
#36284=CARTESIAN_POINT('Ctrl Pts',(34.994106457602,5.00636862977039,5.06231053686134));
#36285=CARTESIAN_POINT('Ctrl Pts',(35.159532794637,-0.499079050747831,7.61770126867609));
#36286=CARTESIAN_POINT('Ctrl Pts',(35.3580443990792,-6.67613314317957,3.70199726504512));
#36287=CARTESIAN_POINT('Ctrl Pts',(35.5565560035213,-6.73212444684914,-3.59917184207896));
#36288=CARTESIAN_POINT('Ctrl Pts',(35.7550676079633,-0.6158509347047,-7.60915107926013));
#36289=CARTESIAN_POINT('Ctrl Pts',(35.9204939449985,4.92814054280995,-5.13849643122668));
#36290=CARTESIAN_POINT('Ctrl Pts',(36.0528350146265,6.63852344254141,-1.03829015457345));
#36291=CARTESIAN_POINT('Ctrl Pts',(36.1520908168476,6.34573214413546,2.26714356729575));
#36292=CARTESIAN_POINT('Ctrl Pts',(36.2513466190686,4.4777196589499,5.00979706149147));
#36293=CARTESIAN_POINT('Ctrl Pts',(36.3836876886968,0.556412225615593,7.09796592129242));
#36294=CARTESIAN_POINT('Ctrl Pts',(36.5491140257318,-5.29804036325235,5.49629155263721));
#36295=CARTESIAN_POINT('Ctrl Pts',(36.747625630174,-7.48870223226711,-1.48151152026111));
#36296=CARTESIAN_POINT('Ctrl Pts',(36.946137234616,-2.81893174721201,-7.09430485056207));
#36297=CARTESIAN_POINT('Ctrl Pts',(37.1446488390581,4.44093494836871,-6.20939202391477));
#36298=CARTESIAN_POINT('Ctrl Pts',(37.3100751760933,7.08076833939991,-0.743931790193501));
#36299=CARTESIAN_POINT('Ctrl Pts',(37.4424162457213,5.74068710172808,3.49178343276199));
#36300=CARTESIAN_POINT('Ctrl Pts',(37.5416720479424,3.38356134522474,5.827501095969));
#36301=CARTESIAN_POINT('Ctrl Pts',(37.6409278501634,0.186523440322275,6.71663970654018));
#36302=CARTESIAN_POINT('Ctrl Pts',(37.7732689197915,-4.15639013967811,5.78058265155737));
#36303=CARTESIAN_POINT('Ctrl Pts',(37.9386952568266,-7.59423760000636,0.778465026161879));
#36304=CARTESIAN_POINT('Ctrl Pts',(38.1372068612687,-4.76365105858751,-5.96516270525666));
#36305=CARTESIAN_POINT('Ctrl Pts',(38.3357184657108,2.42590824614302,-7.23812867317666));
#36306=CARTESIAN_POINT('Ctrl Pts',(38.5342300701529,7.39984846791683,-1.87635155932356));
#36307=CARTESIAN_POINT('Ctrl Pts',(38.6996564071881,5.88848152056962,4.00206198935123));
#36308=CARTESIAN_POINT('Ctrl Pts',(38.8319974768161,2.13098288624362,6.37235842367635));
#36309=CARTESIAN_POINT('Ctrl Pts',(38.9312532790372,-1.17698455269417,6.63498031369624));
#36310=CARTESIAN_POINT('Ctrl Pts',(39.0305090812582,-4.19278538862937,5.25058002759297));
#36311=CARTESIAN_POINT('Ctrl Pts',(39.1628501508863,-6.90573748732343,1.73248507666748));
#36312=CARTESIAN_POINT('Ctrl Pts',(39.3282764879214,-6.30296026868749,-4.30710394275017));
#36313=CARTESIAN_POINT('Ctrl Pts',(39.5267880923636,0.211721730493496,-7.63090501952448));
#36314=CARTESIAN_POINT('Ctrl Pts',(39.7252996968055,6.52476300755405,-3.96270175554772));
#36315=CARTESIAN_POINT('Ctrl Pts',(39.9238113012478,6.86311573771183,3.34306668989407));
#36316=CARTESIAN_POINT('Ctrl Pts',(40.0892376382828,1.91450958570585,6.85750449004156));
#36317=CARTESIAN_POINT('Ctrl Pts',(40.221578707911,-2.4853855017414,6.24266760680046));
#36318=CARTESIAN_POINT('Ctrl Pts',(40.3208345101319,-5.18152965472103,4.30813263928398));
#36319=CARTESIAN_POINT('Ctrl Pts',(40.4200903123531,-6.59144629170504,1.30417626294528));
#36320=CARTESIAN_POINT('Ctrl Pts',(40.552431381981,-6.39285379686092,-3.1340285762355));
#36321=CARTESIAN_POINT('Ctrl Pts',(40.7178577190163,-2.03420042254427,-7.35802155223996));
#36322=CARTESIAN_POINT('Ctrl Pts',(40.9163693234582,5.08707838054148,-5.69185128568854));
#36323=CARTESIAN_POINT('Ctrl Pts',(41.1148809279005,7.54135690419678,1.18468289077305));
#36324=CARTESIAN_POINT('Ctrl Pts',(41.3133925323425,3.08428624104439,6.98323928457356));
#36325=CARTESIAN_POINT('Ctrl Pts',(41.4788188693776,-2.96386576801207,6.47350094569438));
#36326=CARTESIAN_POINT('Ctrl Pts',(41.6111599390057,-5.92767194115434,3.1639761850105));
#36327=CARTESIAN_POINT('Ctrl Pts',(41.7104157412268,-6.738349673723,-0.0538523449313299));
#36328=CARTESIAN_POINT('Ctrl Pts',(41.8096715434477,-5.87634552656026,-3.25831293674151));
#36329=CARTESIAN_POINT('Ctrl Pts',(41.9420126130759,-2.86002240110445,-6.52004498833256));
#36330=CARTESIAN_POINT('Ctrl Pts',(42.1074389501108,3.19550411174225,-6.93305170860172));
#36331=CARTESIAN_POINT('Ctrl Pts',(42.3059505545532,7.55932819127609,-1.06399943832004));
#36332=CARTESIAN_POINT('Ctrl Pts',(42.5044621589951,4.99545677214538,5.77243009016082));
#36333=CARTESIAN_POINT('Ctrl Pts',(42.7029737634373,-2.15154250073096,7.3245694337521));
#36334=CARTESIAN_POINT('Ctrl Pts',(42.8684001004724,-6.44212782189157,3.03145244249525));
#36335=CARTESIAN_POINT('Ctrl Pts',(43.0007411701004,-6.56975993316737,-1.40935955732047));
#36336=CARTESIAN_POINT('Ctrl Pts',(43.0999969723215,-5.1120117039375,-4.39039778826742));
#36337=CARTESIAN_POINT('Ctrl Pts',(43.1992527745426,-2.38529261979699,-6.28159367192785));
#36338=CARTESIAN_POINT('Ctrl Pts',(43.3315938441706,2.02386727969302,-6.82602930105693));
#36339=CARTESIAN_POINT('Ctrl Pts',(43.4970201812058,6.91567071255501,-3.23294774436825));
#36340=CARTESIAN_POINT('Ctrl Pts',(43.6955317856478,6.46059443970595,4.06647968073216));
#36341=CARTESIAN_POINT('Ctrl Pts',(43.8940433900899,0.0897313265003367,
7.63331420794476));
#36342=CARTESIAN_POINT('Ctrl Pts',(44.0925549945321,-6.37099482527689,4.20581471995643));
#36343=CARTESIAN_POINT('Ctrl Pts',(44.2579813315672,-6.8771654018304,-1.84263692043955));
#36344=CARTESIAN_POINT('Ctrl Pts',(44.3903224011952,-4.10833076915798,-5.31692187571454));
#36345=CARTESIAN_POINT('Ctrl Pts',(44.4895782034163,-1.07078853494371,-6.65294433419148));
#36346=CARTESIAN_POINT('Ctrl Pts',(44.5888340056373,2.23255892846622,-6.337485350846));
#36347=CARTESIAN_POINT('Ctrl Pts',(44.7211750752654,5.95169359014882,-3.90743626866535));
#36348=CARTESIAN_POINT('Ctrl Pts',(44.8866014123005,7.368913876263,1.99438231202681));
#36349=CARTESIAN_POINT('Ctrl Pts',(45.0851130167426,2.30991268916776,7.27597697059224));
#36350=CARTESIAN_POINT('Ctrl Pts',(45.2836246211847,-4.85838268646827,5.88826419074352));
#36351=CARTESIAN_POINT('Ctrl Pts',(45.4821362256269,-7.58082549814641,-0.899742901589314));
#36352=CARTESIAN_POINT('Ctrl Pts',(45.6475625626619,-4.06346923403625,-5.84627510204067));
#36353=CARTESIAN_POINT('Ctrl Pts',(45.7799036322901,0.293850439736193,-6.7128005973907));
#36354=CARTESIAN_POINT('Ctrl Pts',(45.879159434511,3.4762690362925,-5.77267788705827));
#36355=CARTESIAN_POINT('Ctrl Pts',(45.9784152367322,5.7957623606931,-3.39958506286211));
#36356=CARTESIAN_POINT('Ctrl Pts',(46.1107563063601,7.06797376310207,0.857007391333677));
#36357=CARTESIAN_POINT('Ctrl Pts',(46.2761826433955,4.34112411504214,6.27957752879176));
#36358=CARTESIAN_POINT('Ctrl Pts',(46.4746942478373,-2.9319586531779,7.04834420018078));
#36359=CARTESIAN_POINT('Ctrl Pts',(46.6732058522796,-7.51142440282901,1.3616317228796));
#36360=CARTESIAN_POINT('Ctrl Pts',(46.8717174567216,-5.20951740344347,-5.58026710342137));
#36361=CARTESIAN_POINT('Ctrl Pts',(47.0371437937567,0.669786645085241,-7.08816623921626));
#36362=CARTESIAN_POINT('Ctrl Pts',(47.1694848633848,4.55721837534439,-4.93759056835269));
#36363=CARTESIAN_POINT('Ctrl Pts',(47.2687406656058,6.38115692357772,-2.16543130047887));
#36364=CARTESIAN_POINT('Ctrl Pts',(47.3679964678269,6.62108067967075,1.14425983699188));
#36365=CARTESIAN_POINT('Ctrl Pts',(47.5003375374549,4.84538340573927,5.21660564314443));
#36366=CARTESIAN_POINT('Ctrl Pts',(47.6657638744901,-0.737387941134879,
7.59833610381744));
#36367=CARTESIAN_POINT('Ctrl Pts',(47.8642754789322,-6.78878943491683,3.4911137931223));
#36368=CARTESIAN_POINT('Ctrl Pts',(48.0627870833743,-6.61611203357758,-3.8082278118985));
#36369=CARTESIAN_POINT('Ctrl Pts',(48.2612986878164,-0.377262972701469,
-7.6247049235846));
#36370=CARTESIAN_POINT('Ctrl Pts',(48.4267250248515,5.08663912970787,-4.98164803542207));
#36371=CARTESIAN_POINT('Ctrl Pts',(48.5590660944796,6.66778231879769,-0.82989089065422));
#36372=CARTESIAN_POINT('Ctrl Pts',(48.6583218967007,6.27162264185577,2.46475269318842));
#36373=CARTESIAN_POINT('Ctrl Pts',(48.7575776989217,4.31863821441834,5.14756291017678));
#36374=CARTESIAN_POINT('Ctrl Pts',(48.8899187685498,0.333861537911319,7.11190911487227));
#36375=CARTESIAN_POINT('Ctrl Pts',(49.0553451055849,-5.46756213577111,5.32768400093223));
#36376=CARTESIAN_POINT('Ctrl Pts',(49.253856710027,-7.43863477210073,-1.71529887642388));
#36377=CARTESIAN_POINT('Ctrl Pts',(49.452368314469,-2.59538604019765,-7.17910222872708));
#36378=CARTESIAN_POINT('Ctrl Pts',(49.6508799189113,4.63320833659035,-6.06727558563615));
#36379=CARTESIAN_POINT('Ctrl Pts',(49.8163062559462,7.10059227460798,-0.521827686576112));
#36380=CARTESIAN_POINT('Ctrl Pts',(49.9486473255744,5.6285238898169,3.66984451482926));
#36381=CARTESIAN_POINT('Ctrl Pts',(50.0479031277954,3.19940956165385,5.93060155947232));
#36382=CARTESIAN_POINT('Ctrl Pts',(50.1471589300164,-0.0239043344667595,
6.71918659690707));
#36383=CARTESIAN_POINT('Ctrl Pts',(50.2794999996446,-4.33537461798565,5.64758724646426));
#36384=CARTESIAN_POINT('Ctrl Pts',(50.4449263366796,-7.61489113323075,0.540264334701967));
#36385=CARTESIAN_POINT('Ctrl Pts',(50.6434379411218,-4.57451143045198,-6.11141413102002));
#36386=CARTESIAN_POINT('Ctrl Pts',(50.8419495455638,2.65138552930593,-7.15860966132069));
#36387=CARTESIAN_POINT('Ctrl Pts',(51.040461150006,7.45497842904763,-1.64369983413683));
#36388=CARTESIAN_POINT('Ctrl Pts',(51.2058874870411,5.76026609022641,4.18450108788224));
#36389=CARTESIAN_POINT('Ctrl Pts',(51.3382285566691,1.93038284825529,6.43596628335045));
#36390=CARTESIAN_POINT('Ctrl Pts',(51.4374843588902,-1.3841863643057,6.59486804335672));
#36391=CARTESIAN_POINT('Ctrl Pts',(51.5367401611112,-4.35515461196362,5.11670482314096));
#36392=CARTESIAN_POINT('Ctrl Pts',(51.6690812307394,-6.95660450857366,1.51537734442372));
#36393=CARTESIAN_POINT('Ctrl Pts',(51.8345075677744,-6.16498895122,-4.50237312465798));
#36394=CARTESIAN_POINT('Ctrl Pts',(52.0330191722166,0.450585044043654,-7.62053217474022));
#36395=CARTESIAN_POINT('Ctrl Pts',(52.2315307766586,6.64565768313247,-3.75643068174953));
#36396=CARTESIAN_POINT('Ctrl Pts',(52.4300423811008,6.75505919226148,3.55635035272829));
#36397=CARTESIAN_POINT('Ctrl Pts',(52.5954687181358,1.698823028496,6.91409539293113));
#36398=CARTESIAN_POINT('Ctrl Pts',(52.727809787764,-2.67966005093835,6.16177425362753));
#36399=CARTESIAN_POINT('Ctrl Pts',(52.8270655899849,-5.31390053926433,4.14375644303857));
#36400=CARTESIAN_POINT('Ctrl Pts',(52.9263213922061,-6.62905466770849,1.09712084739758));
#36401=CARTESIAN_POINT('Ctrl Pts',(53.0586624618341,-6.29157407007032,-3.33268818006107));
#36402=CARTESIAN_POINT('Ctrl Pts',(53.2240887988692,-1.80278111855577,-7.41811517576303));
#36403=CARTESIAN_POINT('Ctrl Pts',(53.4226004033114,5.26282771129787,-5.52975424312528));
#36404=CARTESIAN_POINT('Ctrl Pts',(53.6211120077534,7.50055901634054,1.42026474664386));
#36405=CARTESIAN_POINT('Ctrl Pts',(53.8196236121956,2.864088485346,7.0764008980848));
#36406=CARTESIAN_POINT('Ctrl Pts',(53.9850499492306,-3.16513435150749,6.37751043288894));
#36407=CARTESIAN_POINT('Ctrl Pts',(54.1173910188587,-6.02384681155226,2.97679517807551));
#36408=CARTESIAN_POINT('Ctrl Pts',(54.2166468210798,-6.73335837962768,-0.264842088639801));
#36409=CARTESIAN_POINT('Ctrl Pts',(54.3159026233008,-5.77142707271232,-3.44073676494229));
#36410=CARTESIAN_POINT('Ctrl Pts',(54.448243692929,-2.65443989208741,-6.60641079891305));
#36411=CARTESIAN_POINT('Ctrl Pts',(54.6136700299639,3.41105024174233,-6.82958188841868));
#36412=CARTESIAN_POINT('Ctrl Pts',(54.8121816344061,7.58894055686031,-0.826751917208314));
#36413=CARTESIAN_POINT('Ctrl Pts',(55.0106932388483,4.81223901059941,5.926035201805));
#36414=CARTESIAN_POINT('Ctrl Pts',(55.2092048432903,-2.37986130163657,7.25359998257966));
#36415=CARTESIAN_POINT('Ctrl Pts',(55.3746311803254,-6.53390029971636,2.82822588526208));
#36416=CARTESIAN_POINT('Ctrl Pts',(55.5069722499535,-6.52240266402268,-1.6144049769534));
#36417=CARTESIAN_POINT('Ctrl Pts',(55.6062280521746,-4.97201609009227,-4.54833072679206));
#36418=CARTESIAN_POINT('Ctrl Pts',(55.7054838543956,-2.18741021583949,-6.3532099358437));
#36419=CARTESIAN_POINT('Ctrl Pts',(55.8378249240237,2.23663656514571,-6.75930260161158));
#36420=CARTESIAN_POINT('Ctrl Pts',(56.0032512610587,7.01352090499909,-3.01479303393244));
#36421=CARTESIAN_POINT('Ctrl Pts',(56.2017628655009,6.33008112735583,4.26680330332445));
#36422=CARTESIAN_POINT('Ctrl Pts',(56.400274469943,-0.149355282209104,7.63238039590815));
#36423=CARTESIAN_POINT('Ctrl Pts',(56.5987860743851,-6.49957817086878,4.00423976842957));
#36424=CARTESIAN_POINT('Ctrl Pts',(56.7642124114202,-6.81608897840635,-2.05709645450743));
#36425=CARTESIAN_POINT('Ctrl Pts',(56.8965534810482,-3.93981266455918,-5.44296942021918));
#36426=CARTESIAN_POINT('Ctrl Pts',(56.9958092832694,-0.861921731593391,
-6.68321384732111));
#36427=CARTESIAN_POINT('Ctrl Pts',(57.0950650854903,2.4299267624953,-6.26446293549345));
#36428=CARTESIAN_POINT('Ctrl Pts',(57.2274061551185,6.07113865401073,-3.71913837178403));
#36429=CARTESIAN_POINT('Ctrl Pts',(57.3928324921535,7.30284425781954,2.2241668706146));
#36430=CARTESIAN_POINT('Ctrl Pts',(57.5913440965957,2.08092744393462,7.34474495685501));
#36431=CARTESIAN_POINT('Ctrl Pts',(57.7898557010377,-5.04039499077211,5.73323258251105));
#36432=CARTESIAN_POINT('Ctrl Pts',(57.98836730548,-7.54893134867238,-1.13670049500218));
#36433=CARTESIAN_POINT('Ctrl Pts',(58.1537936425149,-3.87839606375768,-5.97065815110265));
#36434=CARTESIAN_POINT('Ctrl Pts',(58.2861347121431,0.503922387441998,-6.70030612499883));
#36435=CARTESIAN_POINT('Ctrl Pts',(58.3853905143641,3.65533954142928,-5.66098482927496));
#36436=CARTESIAN_POINT('Ctrl Pts',(58.4846463165852,5.89938018465789,-3.21641934115063));
#36437=CARTESIAN_POINT('Ctrl Pts',(58.6169873862132,7.03766943783764,1.07792563214058));
#36438=CARTESIAN_POINT('Ctrl Pts',(58.7824137232483,4.14234559697983,6.41244301943407));
#36439=CARTESIAN_POINT('Ctrl Pts',(58.9809253276904,-3.15124450627053,6.95307094526344));
#36440=CARTESIAN_POINT('Ctrl Pts',(59.1794369321325,-7.55038082733314,1.12573836676515));
#36441=CARTESIAN_POINT('Ctrl Pts',(59.3779485365747,-5.03221237337296,-5.74066992184528));
#36442=CARTESIAN_POINT('Ctrl Pts',(59.5433748736097,0.891429051179542,-7.06371495966627));
#36443=CARTESIAN_POINT('Ctrl Pts',(59.6757159432379,4.70960737511203,-4.79245639662505));
#36444=CARTESIAN_POINT('Ctrl Pts',(59.7749717454588,6.44583924427009,-1.96453883581995));
#36445=CARTESIAN_POINT('Ctrl Pts',(59.8742275476801,6.5820000239748,1.35104242185723));
#36446=CARTESIAN_POINT('Ctrl Pts',(60.0065686173079,4.67964528192059,5.36578370977611));
#36447=CARTESIAN_POINT('Ctrl Pts',(60.1719949543433,-0.974973519581309,
7.57151762584112));
#36448=CARTESIAN_POINT('Ctrl Pts',(60.3705065587851,-6.89478650842269,3.276805839753));
#36449=CARTESIAN_POINT('Ctrl Pts',(60.5690181632275,-6.49360978533135,-4.01354823865563));
#36450=CARTESIAN_POINT('Ctrl Pts',(60.7675297676693,-0.138304947903981,
-7.63277958961821));
#36451=CARTESIAN_POINT('Ctrl Pts',(60.9329561047046,5.24014816196206,-4.81991307238892));
#36452=CARTESIAN_POINT('Ctrl Pts',(61.0652971743326,6.69050067549388,-0.620677575298068));
#36453=CARTESIAN_POINT('Ctrl Pts',(61.1645529765537,6.19136121838743,2.65994410916198));
#36454=CARTESIAN_POINT('Ctrl Pts',(61.2638087787748,4.15532055811943,5.2802794434132));
#36455=CARTESIAN_POINT('Ctrl Pts',(61.3961498484028,0.110983360806127,7.11887613871208));
#36456=CARTESIAN_POINT('Ctrl Pts',(61.5615761854379,-5.63172070117528,5.15385045051374));
#36457=CARTESIAN_POINT('Ctrl Pts',(61.76008778988,-7.38127065249784,-1.94740367226242));
#36458=CARTESIAN_POINT('Ctrl Pts',(61.9585993943222,-2.36929448321922,-7.25685752650235));
#36459=CARTESIAN_POINT('Ctrl Pts',(62.1571109987642,4.82093694685279,-5.91920767305697));
#36460=CARTESIAN_POINT('Ctrl Pts',(62.3225373357993,7.11345114092422,-0.299211714983929));
#36461=CARTESIAN_POINT('Ctrl Pts',(62.4548784054274,5.5108395811942,3.8443057957979));
#36462=CARTESIAN_POINT('Ctrl Pts',(62.5541342076485,3.01211943311833,6.02788461411204));
#36463=CARTESIAN_POINT('Ctrl Pts',(62.6533900098696,-0.234308661164597,
6.71514254447107));
#36464=CARTESIAN_POINT('Ctrl Pts',(62.7857310794975,-4.51010646753767,5.50905204515032));
#36465=CARTESIAN_POINT('Ctrl Pts',(62.9511574165328,-7.62807511471915,0.301533690504745));
#36466=CARTESIAN_POINT('Ctrl Pts',(63.1496690209747,-4.38088460096325,-6.25167078637463));
#36467=CARTESIAN_POINT('Ctrl Pts',(63.348180625417,2.87426203183569,-7.07206867051746));
#36468=CARTESIAN_POINT('Ctrl Pts',(63.546692229859,7.50279569901947,-1.40943578111309));
#36469=CARTESIAN_POINT('Ctrl Pts',(63.7121185668941,5.62640033543055,4.36283555158418));
#36470=CARTESIAN_POINT('Ctrl Pts',(63.8444596365222,1.72788927110751,6.49326101493335));
#36471=CARTESIAN_POINT('Ctrl Pts',(63.9437154387432,-1.59003040842209,6.54828677599809));
#36472=CARTESIAN_POINT('Ctrl Pts',(64.0429712409644,-4.51325180407346,4.97781057235896));
#36473=CARTESIAN_POINT('Ctrl Pts',(64.1753123105923,-7.000647700517,1.29678315764307));
#36474=CARTESIAN_POINT('Ctrl Pts',(64.3407386476275,-6.02097031106359,-4.69322586667211));
#36475=CARTESIAN_POINT('Ctrl Pts',(64.5392502520696,0.689006372509483,-7.60268424484393));
#36476=CARTESIAN_POINT('Ctrl Pts',(64.7377618565116,6.76003354143388,-3.54647487328871));
#36477=CARTESIAN_POINT('Ctrl Pts',(64.9362734609539,6.64037651608413,3.76614554245524));
#36478=CARTESIAN_POINT('Ctrl Pts',(65.1016997979887,1.48147007234857,6.96390416428755));
#36479=CARTESIAN_POINT('Ctrl Pts',(65.2340408676171,-2.8713060846355,6.07483673111265));
#36480=CARTESIAN_POINT('Ctrl Pts',(65.3332966698379,-5.44105894547704,3.97531557893542));
#36481=CARTESIAN_POINT('Ctrl Pts',(65.4325524720591,-6.66016051256749,0.888989250902352));
#36482=CARTESIAN_POINT('Ctrl Pts',(65.5648935416871,-6.1841228514889,-3.52807870413704));
#36483=CARTESIAN_POINT('Ctrl Pts',(65.7303198787223,-1.5695934417308,-7.4709322676986));
#36484=CARTESIAN_POINT('Ctrl Pts',(65.9288314831644,5.43341466181217,-5.36223298852923));
#36485=CARTESIAN_POINT('Ctrl Pts',(66.1273430876064,7.4524037266176,1.65445344554935));
#36486=CARTESIAN_POINT('Ctrl Pts',(66.3258546920486,2.64108130591095,7.16262117174185));
#36487=CARTESIAN_POINT('Ctrl Pts',(66.4912810290836,-3.36329821134536,6.27526413322609));
#36488=CARTESIAN_POINT('Ctrl Pts',(66.6236220987118,-6.11411280714021,2.78669419017976));
#36489=CARTESIAN_POINT('Ctrl Pts',(66.7228779009328,-6.7217622422898,-0.475572041781676));
#36490=CARTESIAN_POINT('Ctrl Pts',(66.8221337031539,-5.6608473448675,-3.61978553310384));
#36491=CARTESIAN_POINT('Ctrl Pts',(66.9544747727819,-2.44625360979039,-6.68629627682944));
#36492=CARTESIAN_POINT('Ctrl Pts',(67.1199011098171,3.62325043248716,-6.71941286407468));
#36493=CARTESIAN_POINT('Ctrl Pts',(67.3184127142591,7.61110881438817,-0.588693378977541));
#36494=CARTESIAN_POINT('Ctrl Pts',(67.5169243187013,4.62430087878972,6.07382730138981));
#36495=CARTESIAN_POINT('Ctrl Pts',(67.7154359231433,-2.60584570588013,7.17551553766098));
#36496=CARTESIAN_POINT('Ctrl Pts',(67.8808622601786,-6.6192635106055,2.6222247966042));
#36497=CARTESIAN_POINT('Ctrl Pts',(68.0132033298065,-6.46864758360768,-1.81786640520943));
#36498=CARTESIAN_POINT('Ctrl Pts',(68.1124591320277,-4.82714313111536,-4.70180301706438));
#36499=CARTESIAN_POINT('Ctrl Pts',(68.2117149342486,-1.98738256811678,-6.41859263889639));
#36500=CARTESIAN_POINT('Ctrl Pts',(68.3440560038768,2.44721280412095,-6.6859490868509));
#36501=CARTESIAN_POINT('Ctrl Pts',(68.5094823409118,7.10448960071639,-2.79367398074271));
#36502=CARTESIAN_POINT('Ctrl Pts',(68.7079939453539,6.1933616077837,4.46292976341907));
#36503=CARTESIAN_POINT('Ctrl Pts',(68.906505549796,-0.388301013108626,7.6239815918582));
#36504=CARTESIAN_POINT('Ctrl Pts',(69.1050171542382,-6.6217748926354,3.79869417354387));
#36505=CARTESIAN_POINT('Ctrl Pts',(69.2704434912732,-6.74834606556275,-2.26946287551695));
#36506=CARTESIAN_POINT('Ctrl Pts',(69.4027845609014,-3.76740267812313,-5.56378310329283));
#36507=CARTESIAN_POINT('Ctrl Pts',(69.5020403631223,-0.652269010159462,
-6.70669787709258));
#36508=CARTESIAN_POINT('Ctrl Pts',(69.6012961653433,2.62502096323833,-6.18571980719947));
#36509=CARTESIAN_POINT('Ctrl Pts',(69.7336372349716,6.18439098099528,-3.52627587749464));
#36510=CARTESIAN_POINT('Ctrl Pts',(69.8990635720066,7.23009515188822,2.44990214044399));
#36511=CARTESIAN_POINT('Ctrl Pts',(70.0975751764487,1.84909688725878,7.4094104631578));
#36512=CARTESIAN_POINT('Ctrl Pts',(70.2960867808908,-5.21599118824087,5.56690523187216));
#36513=CARTESIAN_POINT('Ctrl Pts',(70.4945983853329,-7.51246959013067,-1.36166401884761));
#36514=CARTESIAN_POINT('Ctrl Pts',(70.6931099897751,-2.91938464087065,-7.05530449130318));
#36515=CARTESIAN_POINT('Ctrl Pts',(70.8585363268101,3.12150592612419,-6.40096939299454));
#36516=CARTESIAN_POINT('Ctrl Pts',(70.9908773964382,5.99347114250277,-3.02271415117323));
#36517=CARTESIAN_POINT('Ctrl Pts',(71.1232184660663,7.0011077487275,1.29209572680489));
#36518=CARTESIAN_POINT('Ctrl Pts',(71.2886448031014,3.94386244225407,6.54279353784522));
#36519=CARTESIAN_POINT('Ctrl Pts',(71.4871564075435,-3.3774734808755,6.848092155856));
#36520=CARTESIAN_POINT('Ctrl Pts',(71.6525827445786,-6.86299555174514,1.88573569827787));
#36521=CARTESIAN_POINT('Ctrl Pts',(71.7849238142066,-6.23324656129562,-2.51205469018619));
#36522=CARTESIAN_POINT('Ctrl Pts',(71.8841796164277,-4.28543654678419,-5.19968989554554));
#36523=CARTESIAN_POINT('Ctrl Pts',(71.9834354186487,-1.27646022566982,-6.59696982891652));
#36524=CARTESIAN_POINT('Ctrl Pts',(72.1157764882769,3.16136854322932,-6.37945219356449));
#36525=CARTESIAN_POINT('Ctrl Pts',(72.2812028253119,7.36647591564621,-2.00294299890811));
#36526=CARTESIAN_POINT('Ctrl Pts',(72.4797144297541,5.67025131620974,5.11122006794026));
#36527=CARTESIAN_POINT('Ctrl Pts',(72.6782260341961,-1.2167407171549,7.53625156965662));
#36528=CARTESIAN_POINT('Ctrl Pts',(72.8767376386383,-6.99625824654105,3.05459682075844));
#36529=CARTESIAN_POINT('Ctrl Pts',(73.0421639756734,-6.46086195001876,-2.9913395844494));
#36530=CARTESIAN_POINT('Ctrl Pts',(73.1745050453014,-3.13876262892288,-5.94105822926261));
#36531=CARTESIAN_POINT('Ctrl Pts',(73.2737608475225,0.0824736114544292,
-6.73806046974298));
#36532=CARTESIAN_POINT('Ctrl Pts',(73.3730166497436,3.28324711120387,-5.86245117769648));
#36533=CARTESIAN_POINT('Ctrl Pts',(73.5053577193716,6.53213460317267,-2.83229985644436));
#36534=CARTESIAN_POINT('Ctrl Pts',(73.6707840564068,6.91941525444984,3.22492663651895));
#36535=CARTESIAN_POINT('Ctrl Pts',(73.8692956608488,1.0318779221477,7.56377977437356));
#36536=CARTESIAN_POINT('Ctrl Pts',(74.0678072652908,-5.79359835649274,4.97089069632919));
#36537=CARTESIAN_POINT('Ctrl Pts',(74.2663188697332,-7.31536376747108,-2.18263753902794));
#36538=CARTESIAN_POINT('Ctrl Pts',(74.4317452067681,-3.00405918604541,-6.45494716469223));
#36539=CARTESIAN_POINT('Ctrl Pts',(74.5640862763963,1.43725486725013,-6.56371376365296));
#36540=CARTESIAN_POINT('Ctrl Pts',(74.6633420786172,4.41207377938405,-5.0933153676217));
#36541=CARTESIAN_POINT('Ctrl Pts',(74.7625978808384,6.29166960657197,-2.35858717292915));
#36542=CARTESIAN_POINT('Ctrl Pts',(74.8949389504664,6.81737041885829,2.05284568347206));
#36543=CARTESIAN_POINT('Ctrl Pts',(75.0603652875016,3.20354111649094,6.92934173083288));
#36544=CARTESIAN_POINT('Ctrl Pts',(75.2588768919436,-4.09388730274326,6.44326192662146));
#36545=CARTESIAN_POINT('Ctrl Pts',(75.4573884963858,-7.63362651069499,0.0573045431487054));
#36546=CARTESIAN_POINT('Ctrl Pts',(75.6559001008278,-4.17871307428154,-6.38880345308914));
#36547=CARTESIAN_POINT('Ctrl Pts',(75.8213264378629,1.87183418264915,-6.86927591359667));
#36548=CARTESIAN_POINT('Ctrl Pts',(75.953667507491,5.33432590669687,-4.08570765755734));
#36549=CARTESIAN_POINT('Ctrl Pts',(76.052923309712,6.657432968585,-1.04251746688282));
#36550=CARTESIAN_POINT('Ctrl Pts',(76.1521791119332,6.32794436086292,2.25946013624946));
#36551=CARTESIAN_POINT('Ctrl Pts',(76.2845201815611,3.8821184881069,5.96823850301648));
#36552=CARTESIAN_POINT('Ctrl Pts',(76.4499465185964,-2.02566713052125,7.36037534359628));
#36553=CARTESIAN_POINT('Ctrl Pts',(76.6484581230383,-7.28572372703915,2.27898382650516));
#36554=CARTESIAN_POINT('Ctrl Pts',(76.8469697274806,-5.86757287326853,-4.8833519313097));
#36555=CARTESIAN_POINT('Ctrl Pts',(77.0454813319226,0.931937787573207,-7.57693503221458));
#36556=CARTESIAN_POINT('Ctrl Pts',(77.2109076689577,5.86348378704247,-4.03859785863803));
#36557=CARTESIAN_POINT('Ctrl Pts',(77.3432487385858,6.71149176708757,0.322363461909703));
#36558=CARTESIAN_POINT('Ctrl Pts',(77.4425045408068,5.75785876877837,3.50075974600101));
#36559=CARTESIAN_POINT('Ctrl Pts',(77.5417603430279,3.37493425326742,5.810151351504));
#36560=CARTESIAN_POINT('Ctrl Pts',(77.674101412656,-0.887024091918348,7.06426946294214));
#36561=CARTESIAN_POINT('Ctrl Pts',(77.8395277496911,-6.2979617696608,4.31440958535449));
#36562=CARTESIAN_POINT('Ctrl Pts',(78.0380393541331,-7.03582577797349,-2.96187324681027));
#36563=CARTESIAN_POINT('Ctrl Pts',(78.2365509585753,-1.32971124612974,-7.51714078024904));
#36564=CARTESIAN_POINT('Ctrl Pts',(78.4350625630174,5.60234654932029,-5.18576567766284));
#36565=CARTESIAN_POINT('Ctrl Pts',(78.6004889000525,7.08525706213391,0.699890811613769));
#36566=CARTESIAN_POINT('Ctrl Pts',(78.7328299696805,4.91818716080672,4.57815191890112));
#36567=CARTESIAN_POINT('Ctrl Pts',(78.8320857719017,2.13830489652176,6.39029800321771));
#36568=CARTESIAN_POINT('Ctrl Pts',(78.9313415741226,-1.17237556419702,6.61616017624541));
#36569=CARTESIAN_POINT('Ctrl Pts',(79.0636826437508,-5.23714154545479,4.82317978283739));
#36570=CARTESIAN_POINT('Ctrl Pts',(79.2291089807858,-7.59513515642661,-0.769658676245189));
#36571=CARTESIAN_POINT('Ctrl Pts',(79.4276205852279,-3.46224382358131,-6.80355827594947));
#36572=CARTESIAN_POINT('Ctrl Pts',(79.6261321896702,3.83629839660047,-6.59987515945624));
#36573=CARTESIAN_POINT('Ctrl Pts',(79.8246437941121,7.62623872496982,-0.344870166986757));
#36574=CARTESIAN_POINT('Ctrl Pts',(79.9900701311472,4.95999527493247,5.10775505064086));
#36575=CARTESIAN_POINT('Ctrl Pts',(80.1224112007753,0.8015589650237,6.67124749704671));
#36576=CARTESIAN_POINT('Ctrl Pts',(80.2216670029964,-2.49137202416728,6.26109589749385));
#36577=CARTESIAN_POINT('Ctrl Pts',(80.3209228052174,-5.16586184567227,4.29673263453635));
#36578=CARTESIAN_POINT('Ctrl Pts',(80.4532638748456,-7.11326317567643,0.303647457203498));
#36579=CARTESIAN_POINT('Ctrl Pts',(80.6186902118805,-5.30440997458895,-5.49014456492613));
#36580=CARTESIAN_POINT('Ctrl Pts',(80.8172018163229,1.74688238419706,-7.43128114418698));
#36581=CARTESIAN_POINT('Ctrl Pts',(81.0157134207648,7.19006253712243,-2.56486612134739));
#36582=CARTESIAN_POINT('Ctrl Pts',(81.214225025207,6.04753918347326,4.65894004540328));
#36583=CARTESIAN_POINT('Ctrl Pts',(81.3796513622421,0.491659983350608,7.10274490922151));
#36584=CARTESIAN_POINT('Ctrl Pts',(81.5119924318702,-3.6937211183203,5.61288377229892));
#36585=CARTESIAN_POINT('Ctrl Pts',(81.6112482340912,-5.94413899720338,3.17418776734193));
#36586=CARTESIAN_POINT('Ctrl Pts',(81.7105040363123,-6.7190244278375,-0.0524469196936317));
#36587=CARTESIAN_POINT('Ctrl Pts',(81.8428451059403,-5.62911981515396,-4.3593261969415));
#36588=CARTESIAN_POINT('Ctrl Pts',(82.0082714429754,-0.507911746828754,
-7.61711744557876));
#36589=CARTESIAN_POINT('Ctrl Pts',(82.2067830474175,6.13079130792516,-4.54850914551527));
#36590=CARTESIAN_POINT('Ctrl Pts',(82.4052946518595,7.14728210617843,2.68177105713156));
#36591=CARTESIAN_POINT('Ctrl Pts',(82.603806256302,1.61201659234397,7.46189352834217));
#36592=CARTESIAN_POINT('Ctrl Pts',(82.7692325933366,-4.20893268274398,5.74243854619525));
#36593=CARTESIAN_POINT('Ctrl Pts',(82.901573662965,-6.44410839326842,1.903025737364));
#36594=CARTESIAN_POINT('Ctrl Pts',(83.0008294651858,-6.58892857939596,-1.41218857665568));
#36595=CARTESIAN_POINT('Ctrl Pts',(83.1000852674072,-5.09815815725061,-4.37685084791804));
#36596=CARTESIAN_POINT('Ctrl Pts',(83.2324263370349,-1.48581233031733,-6.96297899636189));
#36597=CARTESIAN_POINT('Ctrl Pts',(83.3978526740704,4.5285210959042,-6.14580744949412));
#36598=CARTESIAN_POINT('Ctrl Pts',(83.5963642785122,7.61854935282431,0.482952654767742));
#36599=CARTESIAN_POINT('Ctrl Pts',(83.7948758829545,3.7281663355713,6.66155486973422));
#36600=CARTESIAN_POINT('Ctrl Pts',(83.9933874873964,-3.58501345126855,6.73989102853529));
#36601=CARTESIAN_POINT('Ctrl Pts',(84.1588138244318,-6.92124953323499,1.66943693603405));
#36602=CARTESIAN_POINT('Ctrl Pts',(84.2911548940596,-6.15033558364338,-2.7058108119069));
#36603=CARTESIAN_POINT('Ctrl Pts',(84.3904106962809,-4.12114584631622,-5.33145508410299));
#36604=CARTESIAN_POINT('Ctrl Pts',(84.4896664985016,-1.06895102396886,-6.63365537615708));
#36605=CARTESIAN_POINT('Ctrl Pts',(84.62200756813,3.3593844327698,-6.27736019498358));
#36606=CARTESIAN_POINT('Ctrl Pts',(84.7874339051648,7.42570637776451,-1.77125303486947));
#36607=CARTESIAN_POINT('Ctrl Pts',(84.9859455096072,5.50734809616266,5.28627037294353));
#36608=CARTESIAN_POINT('Ctrl Pts',(85.1844571140491,-1.4521139677821,7.49445812135466));
#36609=CARTESIAN_POINT('Ctrl Pts',(85.3829687184914,-7.08850356895284,2.83400241271063));
#36610=CARTESIAN_POINT('Ctrl Pts',(85.5483950555264,-6.36400754352169,-3.19219716977184));
#36611=CARTESIAN_POINT('Ctrl Pts',(85.6807361251545,-2.9511792907089,-6.03643775213103));
#36612=CARTESIAN_POINT('Ctrl Pts',(85.7799919273754,0.293442701073721,-6.73217259000419));
#36613=CARTESIAN_POINT('Ctrl Pts',(85.8792477295966,3.46522248184149,-5.75675890520026));
#36614=CARTESIAN_POINT('Ctrl Pts',(86.0115887992246,6.61762713256751,-2.62635220772195));
#36615=CARTESIAN_POINT('Ctrl Pts',(86.1770151362598,6.81503028060682,3.44003122031167));
#36616=CARTESIAN_POINT('Ctrl Pts',(86.3755267407018,0.794506981347646,7.5923840896491));
#36617=CARTESIAN_POINT('Ctrl Pts',(86.574038345144,-5.94642390732348,4.78702206205264));
#36618=CARTESIAN_POINT('Ctrl Pts',(86.7725499495861,-7.24342499302197,-2.41065279390719));
#36619=CARTESIAN_POINT('Ctrl Pts',(86.9379762866213,-2.80044465421751,-6.54585552264672));
#36620=CARTESIAN_POINT('Ctrl Pts',(87.0703173562492,1.64209728247714,-6.51548589562918));
#36621=CARTESIAN_POINT('Ctrl Pts',(87.1695731584704,4.56941058859847,-4.95265012626795));
#36622=CARTESIAN_POINT('Ctrl Pts',(87.2688289606913,6.36244463307709,-2.16040233111586));
#36623=CARTESIAN_POINT('Ctrl Pts',(87.4011700303195,6.7497404841074,2.26532959674766));
#36624=CARTESIAN_POINT('Ctrl Pts',(87.5665963673546,2.98497271291811,7.02626432931763));
#36625=CARTESIAN_POINT('Ctrl Pts',(87.7651079717966,-4.29365470412399,6.31189882602065));
#36626=CARTESIAN_POINT('Ctrl Pts',(87.9636195762388,-7.63167707750089,-0.181775941517044));
#36627=CARTESIAN_POINT('Ctrl Pts',(88.1621311806808,-3.97659372553301,-6.51652935728508));
#36628=CARTESIAN_POINT('Ctrl Pts',(88.327557517716,2.08603233198955,-6.80728902681484));
#36629=CARTESIAN_POINT('Ctrl Pts',(88.459898587344,5.45965645656968,-3.91665562916875));
#36630=CARTESIAN_POINT('Ctrl Pts',(88.5591543895652,6.68681495190187,-0.833523964525788));
#36631=CARTESIAN_POINT('Ctrl Pts',(88.658410191786,6.25408419470987,2.45651599358564));
#36632=CARTESIAN_POINT('Ctrl Pts',(88.7907512614142,3.69331489294256,6.08688260822147));
#36633=CARTESIAN_POINT('Ctrl Pts',(88.9561775984493,-2.25516895510891,7.29333020685474));
#36634=CARTESIAN_POINT('Ctrl Pts',(89.1546892028914,-7.35351837386254,2.04970852401823));
#36635=CARTESIAN_POINT('Ctrl Pts',(89.3532008073335,-5.71176948378593,-5.06470402612628));
#36636=CARTESIAN_POINT('Ctrl Pts',(89.5517124117756,1.16875775810838,-7.54403458536402));
#36637=CARTESIAN_POINT('Ctrl Pts',(89.7171387488108,5.98707953138472,-3.85299798463139));
#36638=CARTESIAN_POINT('Ctrl Pts',(89.8494798184388,6.69810503129157,0.532380438266475));
#36639=CARTESIAN_POINT('Ctrl Pts',(89.9487356206599,5.6454060353462,3.67935416839618));
#36640=CARTESIAN_POINT('Ctrl Pts',(90.047991422881,3.1913300203551,5.91299016086127));
#36641=CARTESIAN_POINT('Ctrl Pts',(90.1803324925089,-1.10781160806457,7.03302696040168));
#36642=CARTESIAN_POINT('Ctrl Pts',(90.3457588295443,-6.4299816593523,4.11506845419367));
#36643=CARTESIAN_POINT('Ctrl Pts',(90.544270433986,-6.93962186627816,-3.18075240489431));
#36644=CARTESIAN_POINT('Ctrl Pts',(90.7427820384285,-1.09365453325676,-7.55509478895228));
#36645=CARTESIAN_POINT('Ctrl Pts',(90.9412936428702,5.76199473674139,-5.00778086342357));
#36646=CARTESIAN_POINT('Ctrl Pts',(91.1067199799058,7.05986447627686,0.921427349986869));
#36647=CARTESIAN_POINT('Ctrl Pts',(91.2390610495334,4.77240695698494,4.72992302032322));
#36648=CARTESIAN_POINT('Ctrl Pts',(91.3383168517549,1.93713947686126,6.45412635819934));
#36649=CARTESIAN_POINT('Ctrl Pts',(91.4375726539756,-1.3789902704871,6.57620147008622));
#36650=CARTESIAN_POINT('Ctrl Pts',(91.5699137236039,-5.38561421805492,4.65680945272449));
#36651=CARTESIAN_POINT('Ctrl Pts',(91.7353400606388,-7.56730766762608,-1.00712818736965));
#36652=CARTESIAN_POINT('Ctrl Pts',(91.9338516650811,-3.24748753305086,-6.90864402258845));
#36653=CARTESIAN_POINT('Ctrl Pts',(92.132363269523,4.04109658682085,-6.47650182460808));
#36654=CARTESIAN_POINT('Ctrl Pts',(92.3308748739652,7.63329823526228,-0.105879997395819));
#36655=CARTESIAN_POINT('Ctrl Pts',(92.4963012110003,4.79760967174002,5.26057565503311));
#36656=CARTESIAN_POINT('Ctrl Pts',(92.6286422806284,0.592251030763429,6.69307692005863));
#36657=CARTESIAN_POINT('Ctrl Pts',(92.7278980828495,-2.68622073210826,6.18000603388127));
#36658=CARTESIAN_POINT('Ctrl Pts',(92.8271538850704,-5.29788341543967,4.132852677954));
#36659=CARTESIAN_POINT('Ctrl Pts',(92.9594949546987,-7.1192833602349,0.0807416954368796));
#36660=CARTESIAN_POINT('Ctrl Pts',(93.1249212917336,-5.12988065443664,-5.65356321212946));
#36661=CARTESIAN_POINT('Ctrl Pts',(93.3234328961759,1.97874140565975,-7.37293157147783));
#36662=CARTESIAN_POINT('Ctrl Pts',(93.5219445006178,7.26685670662967,-2.33844630331303));
#36663=CARTESIAN_POINT('Ctrl Pts',(93.7204561050601,5.89867514420218,4.84603797606646));
#36664=CARTESIAN_POINT('Ctrl Pts',(93.8858824420949,0.268991396450776,7.11465799693386));
#36665=CARTESIAN_POINT('Ctrl Pts',(94.0182235117233,-3.86768090757155,5.49445942186024));
#36666=CARTESIAN_POINT('Ctrl Pts',(94.1174793139442,-6.04062557409786,2.98648607463229));
#36667=CARTESIAN_POINT('Ctrl Pts',(94.2167351161653,-6.71408662382135,-0.262832169045199));
#36668=CARTESIAN_POINT('Ctrl Pts',(94.3490761857933,-5.48984361079027,-4.5334679786853));
#36669=CARTESIAN_POINT('Ctrl Pts',(94.5145025228285,-0.26912725164565,-7.62928719112931));
#36670=CARTESIAN_POINT('Ctrl Pts',(94.7130141272706,6.27022417978169,-4.35428825911284));
#36671=CARTESIAN_POINT('Ctrl Pts',(94.9115257317125,7.05979512689293,2.90427792651901));
#36672=CARTESIAN_POINT('Ctrl Pts',(95.110037336155,1.37755152739009,7.50871522377111));
#36673=CARTESIAN_POINT('Ctrl Pts',(95.2754636731897,-4.38669688173065,5.60781644247689));
#36674=CARTESIAN_POINT('Ctrl Pts',(95.4078047428181,-6.50054242434237,1.70029060180525));
#36675=CARTESIAN_POINT('Ctrl Pts',(95.5070605450389,-6.54147331612773,-1.61783288840539));
#36676=CARTESIAN_POINT('Ctrl Pts',(95.6063163472602,-4.95859356993127,-4.53435659708169));
#36677=CARTESIAN_POINT('Ctrl Pts',(95.738657416888,-1.26703302233638,-7.00609321269774));
#36678=CARTESIAN_POINT('Ctrl Pts',(95.9040837539233,4.71876033125727,-6.00097937494037));
#36679=CARTESIAN_POINT('Ctrl Pts',(96.1025953583653,7.5996887809385,0.721296014854075));
#36680=CARTESIAN_POINT('Ctrl Pts',(96.3011069628075,3.5177265579812,6.77503781328492));
#36681=CARTESIAN_POINT('Ctrl Pts',(96.4996185672496,-3.79431958127109,6.62431818661284));
#36682=CARTESIAN_POINT('Ctrl Pts',(96.6650449042846,-6.97013454965913,1.45187435556547));
#36683=CARTESIAN_POINT('Ctrl Pts',(96.7973859739128,-6.06258474183803,-2.89708580979144));
#36684=CARTESIAN_POINT('Ctrl Pts',(96.8966417761337,-3.95216633883919,-5.45789681384359));
#36685=CARTESIAN_POINT('Ctrl Pts',(96.995897578355,-0.860689169115976,-6.66387680674158));
#36686=CARTESIAN_POINT('Ctrl Pts',(97.1282386479826,3.55431674594619,-6.16907993579157));
#36687=CARTESIAN_POINT('Ctrl Pts',(97.2936649850182,7.47753242254522,-1.53784309735809));
#36688=CARTESIAN_POINT('Ctrl Pts',(97.4921765894599,5.33910370722034,5.45614416155886));
#36689=CARTESIAN_POINT('Ctrl Pts',(97.6906881939024,-1.68609599189039,7.44530844319415));
#36690=CARTESIAN_POINT('Ctrl Pts',(97.8891997983443,-7.17377574087814,2.61063098539322));
#36691=CARTESIAN_POINT('Ctrl Pts',(98.0546261353794,-6.26092037418559,-3.38992490371209));
#36692=CARTESIAN_POINT('Ctrl Pts',(98.1869672050076,-2.76069657366338,-6.1258953932813));
#36693=CARTESIAN_POINT('Ctrl Pts',(98.2862230072284,0.50412149632163,-6.7196813851078));
#36694=CARTESIAN_POINT('Ctrl Pts',(98.3854788094498,3.64379989073183,-5.64541958560787));
#36695=CARTESIAN_POINT('Ctrl Pts',(98.5178198790776,6.69662753697565,-2.4178284504321));
#36696=CARTESIAN_POINT('Ctrl Pts',(98.6832462161129,6.70396080658066,3.65176149633809));
#36697=CARTESIAN_POINT('Ctrl Pts',(98.8817578205549,0.556356465979633,7.6135408970419));
#36698=CARTESIAN_POINT('Ctrl Pts',(99.080269424997,-6.09341640305894,4.59845779007474));
#36699=CARTESIAN_POINT('Ctrl Pts',(99.2787810294392,-7.16438111875819,-2.63630341719029));
#36700=CARTESIAN_POINT('Ctrl Pts',(99.4442073664741,-2.59408309049471,-6.63034295525578));
#36701=CARTESIAN_POINT('Ctrl Pts',(99.5765484361025,1.84532892465688,-6.46086690012156));
#36702=CARTESIAN_POINT('Ctrl Pts',(99.6758042383233,4.72226520925161,-4.80712676074899));
#36703=CARTESIAN_POINT('Ctrl Pts',(99.7750600405444,6.42697864563129,-1.96009832147819));
#36704=CARTESIAN_POINT('Ctrl Pts',(99.9074011101725,6.67548963887232,2.47559141742086));
#36705=CARTESIAN_POINT('Ctrl Pts',(100.072827447207,2.7634763067088,7.11629476796499));
#36706=CARTESIAN_POINT('Ctrl Pts',(100.27133905165,-4.48921039950884,6.1743442969362));
#36707=CARTESIAN_POINT('Ctrl Pts',(100.469850656092,-7.62224162748416,-0.420678119724112));
#36708=CARTESIAN_POINT('Ctrl Pts',(100.668362260534,-3.77057368086733,-6.6378631079179));
#36709=CARTESIAN_POINT('Ctrl Pts',(100.833788597569,2.29818426330452,-6.73862477636194));
#36710=CARTESIAN_POINT('Ctrl Pts',(100.966129667197,5.57963155419069,-3.74376169924608));
#36711=CARTESIAN_POINT('Ctrl Pts',(101.065385469418,6.70963774617368,-0.623712847021004));
#36712=CARTESIAN_POINT('Ctrl Pts',(101.164641271639,6.1740893111309,2.65116222050649));
#36713=CARTESIAN_POINT('Ctrl Pts',(101.296982341267,3.50088847425021,6.19955600632511));
#36714=CARTESIAN_POINT('Ctrl Pts',(101.462408678302,-2.48245865335913,7.21913094192572));
#36715=CARTESIAN_POINT('Ctrl Pts',(101.660920282745,-7.41409985309775,1.81842263417024));
#36716=CARTESIAN_POINT('Ctrl Pts',(101.859431887186,-5.55036334083896,-5.24108808291169));
#36717=CARTESIAN_POINT('Ctrl Pts',(102.057943491629,1.40443127803811,-7.50373409094269));
#36718=CARTESIAN_POINT('Ctrl Pts',(102.223369828664,6.10480246684229,-3.66361865176161));
#36719=CARTESIAN_POINT('Ctrl Pts',(102.355710898292,6.67814803189086,0.741875195308663));
#36720=CARTESIAN_POINT('Ctrl Pts',(102.454966700513,5.52741564527365,3.85433946154237));
#36721=CARTESIAN_POINT('Ctrl Pts',(102.554222502734,3.00459536781169,6.01002883661822));
#36722=CARTESIAN_POINT('Ctrl Pts',(102.686563572362,-1.32751245652532,6.99488566471813));
#36723=CARTESIAN_POINT('Ctrl Pts',(102.851989909397,-6.55569429135308,3.91169079563038));
#36724=CARTESIAN_POINT('Ctrl Pts',(103.050501513839,-6.83661078378366,-3.39651151907381));
#36725=CARTESIAN_POINT('Ctrl Pts',(103.249013118281,-0.856525039568993,
-7.58563790098237));
#36726=CARTESIAN_POINT('Ctrl Pts',(103.447524722723,5.91599090405775,-4.82488384786082));
#36727=CARTESIAN_POINT('Ctrl Pts',(103.612951059759,7.02754677198468,1.14206004755057));
#36728=CARTESIAN_POINT('Ctrl Pts',(103.745292129387,4.62194543336102,4.87705447504003));
#36729=CARTESIAN_POINT('Ctrl Pts',(103.844547931608,1.73407389036543,6.51162377157935));
#36730=CARTESIAN_POINT('Ctrl Pts',(103.943803733829,-1.58425230619208,6.52979207728556));
#36731=CARTESIAN_POINT('Ctrl Pts',(104.076144803457,-5.5288040674127,4.48587119382367));
#36732=CARTESIAN_POINT('Ctrl Pts',(104.241571140492,-7.53205730232312,-1.24360979221905));
#36733=CARTESIAN_POINT('Ctrl Pts',(104.440082744934,-3.02954573728368,-7.00695298559832));
#36734=CARTESIAN_POINT('Ctrl Pts',(104.638594349376,4.24193080980006,-6.34677559873763));
#36735=CARTESIAN_POINT('Ctrl Pts',(104.837105953818,7.63287013777217,0.133214029254973));
#36736=CARTESIAN_POINT('Ctrl Pts',(105.002532290853,4.63051802752086,5.40823609188528));
#36737=CARTESIAN_POINT('Ctrl Pts',(105.134873360481,0.382362148644849,6.70834100647539));
#36738=CARTESIAN_POINT('Ctrl Pts',(105.234129162702,-2.87843448765591,6.092854128331));
#36739=CARTESIAN_POINT('Ctrl Pts',(105.333384964924,-5.42470822093489,3.96491872848158));
#36740=CARTESIAN_POINT('Ctrl Pts',(105.465726034552,-7.11832013585827,-0.142243222249852));
#36741=CARTESIAN_POINT('Ctrl Pts',(105.631152371587,-4.95031937521908,-5.81143629238669));
#36742=CARTESIAN_POINT('Ctrl Pts',(105.829663976029,2.20865947171768,-7.30734963681115));
#36743=CARTESIAN_POINT('Ctrl Pts',(106.028175580471,7.33652268058591,-2.10973295029129));
#36744=CARTESIAN_POINT('Ctrl Pts',(106.226687184913,5.74402508331175,5.02838291200097));
#36745=CARTESIAN_POINT('Ctrl Pts',(106.392113521948,0.0460588288224911,
7.11959125045635));
#36746=CARTESIAN_POINT('Ctrl Pts',(106.524454591576,-4.03784666285289,5.37064683348793));
#36747=CARTESIAN_POINT('Ctrl Pts',(106.623710393797,-6.1311871946683,2.7958519411076));
#36748=CARTESIAN_POINT('Ctrl Pts',(106.722966196018,-6.70256218452041,-0.47295414784101));
#36749=CARTESIAN_POINT('Ctrl Pts',(106.855307265646,-5.34518384502274,-4.70317460525356));
#36750=CARTESIAN_POINT('Ctrl Pts',(107.020733602681,-0.0300757036994695,
-7.63394923387465));
#36751=CARTESIAN_POINT('Ctrl Pts',(107.219245207124,6.40350140800699,-4.15583616799732));
#36752=CARTESIAN_POINT('Ctrl Pts',(107.417756811565,6.96539247494741,3.12400954067283));
#36753=CARTESIAN_POINT('Ctrl Pts',(107.616268416008,1.1417167072316,7.54802637153462));
#36754=CARTESIAN_POINT('Ctrl Pts',(107.781694753043,-4.5601256002143,5.46794866870985));
#36755=CARTESIAN_POINT('Ctrl Pts',(107.914035822671,-6.55064542222453,1.49553103310081));
#36756=CARTESIAN_POINT('Ctrl Pts',(108.013291624892,-6.48750220584516,-1.82111132353179));
#36757=CARTESIAN_POINT('Ctrl Pts',(108.112547427113,-4.81434798793785,-4.68885257359087));
#36758=CARTESIAN_POINT('Ctrl Pts',(108.244888496741,-1.04661762809148,-7.03922361376705));
#36759=CARTESIAN_POINT('Ctrl Pts',(108.410314833777,4.90359337122379,-5.85665907486141));
#36760=CARTESIAN_POINT('Ctrl Pts',(108.608826438218,7.57453469313228,0.969844410039962));
#36761=CARTESIAN_POINT('Ctrl Pts',(108.774252775254,4.0147429951218,5.87799298002767));
#36762=CARTESIAN_POINT('Ctrl Pts',(108.906593844881,-0.353800513992823,
6.71099960051513));
#36763=CARTESIAN_POINT('Ctrl Pts',(109.005849647103,-3.5176048912445,5.74308483611783));
#36764=CARTESIAN_POINT('Ctrl Pts',(109.105105449324,-5.8393379223708,3.34881119764833));
#36765=CARTESIAN_POINT('Ctrl Pts',(109.171275984138,-6.43144388944538,1.2184826508284));
#36766=CARTESIAN_POINT('Ctrl Pts',(109.204361251545,-6.45554076211909,0.144895927237655));
#36767=CARTESIAN_POINT('Ctrl Pts',(30.9296387484553,0.703787020950697,-6.6579895365958));
#36768=CARTESIAN_POINT('Ctrl Pts',(30.9627240158623,1.81104192579756,-6.5409464522485));
#36769=CARTESIAN_POINT('Ctrl Pts',(31.0288945506763,3.9614630703719,-5.74628867867225));
#36770=CARTESIAN_POINT('Ctrl Pts',(31.1281503528974,6.23616430535044,-3.14177596404463));
#36771=CARTESIAN_POINT('Ctrl Pts',(31.2274061551185,6.96475406549829,0.21041611353608));
#36772=CARTESIAN_POINT('Ctrl Pts',(31.3597472247465,5.72907466288608,4.65287937038327));
#36773=CARTESIAN_POINT('Ctrl Pts',(31.5251735617817,0.352018242983719,7.90990755251631));
#36774=CARTESIAN_POINT('Ctrl Pts',(31.7236851662237,-6.47247608523396,4.56415182305037));
#36775=CARTESIAN_POINT('Ctrl Pts',(31.8891115032589,-7.18370815896518,-1.68562073726553));
#36776=CARTESIAN_POINT('Ctrl Pts',(32.0214525728869,-4.43172273725023,-5.37703885971554));
#36777=CARTESIAN_POINT('Ctrl Pts',(32.120708375108,-1.32491932170987,-6.85975389770393));
#36778=CARTESIAN_POINT('Ctrl Pts',(32.219964177329,2.10754325246999,-6.64033724856899));
#36779=CARTESIAN_POINT('Ctrl Pts',(32.3523052469572,6.04134746661423,-4.24261341996023));
#36780=CARTESIAN_POINT('Ctrl Pts',(32.5177315839921,7.70128519312101,1.82755503533256));
#36781=CARTESIAN_POINT('Ctrl Pts',(32.7162431884343,2.6301704824596,7.46537716506742));
#36782=CARTESIAN_POINT('Ctrl Pts',(32.9147547928764,-4.84377258193836,6.25996585329837));
#36783=CARTESIAN_POINT('Ctrl Pts',(33.1132663973185,-7.8854783960754,-0.686285559843319));
#36784=CARTESIAN_POINT('Ctrl Pts',(33.2786927343536,-4.40096077659904,-5.92677383246242));
#36785=CARTESIAN_POINT('Ctrl Pts',(33.4110338039817,0.0865720556418617,
-6.96626254547699));
#36786=CARTESIAN_POINT('Ctrl Pts',(33.5102896062028,3.41514643505138,-6.09531225030999));
#36787=CARTESIAN_POINT('Ctrl Pts',(33.6095454084238,5.89598045223297,-3.71130068472704));
#36788=CARTESIAN_POINT('Ctrl Pts',(33.7418864780519,7.35262722554128,0.65865425285292));
#36789=CARTESIAN_POINT('Ctrl Pts',(33.9073128150869,4.70276240256489,6.36680332881671));
#36790=CARTESIAN_POINT('Ctrl Pts',(34.1058244195291,-2.8096405407784,7.39965803111618));
#36791=CARTESIAN_POINT('Ctrl Pts',(34.3043360239712,-7.74015409929537,1.65500165199733));
#36792=CARTESIAN_POINT('Ctrl Pts',(34.5028476284133,-5.58000359828515,-5.61388574230308));
#36793=CARTESIAN_POINT('Ctrl Pts',(34.6682739654484,0.463975112574999,-7.36747544056416));
#36794=CARTESIAN_POINT('Ctrl Pts',(34.8006150350764,4.56249195730454,-5.26497779023408));
#36795=CARTESIAN_POINT('Ctrl Pts',(34.8998708372975,6.542717437068,-2.45130946226545));
#36796=CARTESIAN_POINT('Ctrl Pts',(34.9991266395185,6.89882340027391,0.970855166879508));
#36797=CARTESIAN_POINT('Ctrl Pts',(35.1314677091467,5.19083011233475,5.24883321944595));
#36798=CARTESIAN_POINT('Ctrl Pts',(35.2968940461817,-0.517467800843383,
7.89837825706199));
#36799=CARTESIAN_POINT('Ctrl Pts',(35.4954056506239,-6.92211770973079,3.83839870777912));
#36800=CARTESIAN_POINT('Ctrl Pts',(35.693917255066,-6.98017203345505,-3.73178464450976));
#36801=CARTESIAN_POINT('Ctrl Pts',(35.8924288595081,-0.638542187557634,
-7.88951303279094));
#36802=CARTESIAN_POINT('Ctrl Pts',(36.0578551965432,5.10971968290926,-5.32782621094353));
#36803=CARTESIAN_POINT('Ctrl Pts',(36.1901962661712,6.88312226592188,-1.07654633493236));
#36804=CARTESIAN_POINT('Ctrl Pts',(36.2894520683923,6.57954296507732,2.35067730093337));
#36805=CARTESIAN_POINT('Ctrl Pts',(36.3887078706133,4.64270287690269,5.19438486587639));
#36806=CARTESIAN_POINT('Ctrl Pts',(36.5210489402414,0.576913437500505,7.35949307078124));
#36807=CARTESIAN_POINT('Ctrl Pts',(36.6864752772765,-5.49324859747658,5.69880442441749));
#36808=CARTESIAN_POINT('Ctrl Pts',(36.8849868817186,-7.76462620399256,-1.53609835388737));
#36809=CARTESIAN_POINT('Ctrl Pts',(37.0834984861608,-2.92279631807994,-7.35569710656138));
#36810=CARTESIAN_POINT('Ctrl Pts',(37.2820100906028,4.60456282021147,-6.43817934327911));
#36811=CARTESIAN_POINT('Ctrl Pts',(37.4474364276379,7.34166183769624,-0.771342228995147));
#36812=CARTESIAN_POINT('Ctrl Pts',(37.5797774972661,5.9522048168692,3.62043946998871));
#36813=CARTESIAN_POINT('Ctrl Pts',(37.679033299487,3.50822990006823,6.0422175044686));
#36814=CARTESIAN_POINT('Ctrl Pts',(37.7782891017082,0.19339596467639,6.96411675222807));
#36815=CARTESIAN_POINT('Ctrl Pts',(37.9106301713363,-4.30953385401096,5.99357033281832));
#36816=CARTESIAN_POINT('Ctrl Pts',(38.0760565083712,-7.8740500609415,0.807147854668614));
#36817=CARTESIAN_POINT('Ctrl Pts',(38.2745681128135,-4.93916952350055,-6.18495130608158));
#36818=CARTESIAN_POINT('Ctrl Pts',(38.4730797172554,2.51529172241946,-7.50482017050409));
#36819=CARTESIAN_POINT('Ctrl Pts',(38.6715913216977,7.67249859020869,-1.94548641854781));
#36820=CARTESIAN_POINT('Ctrl Pts',(38.8370176587327,6.10544477510872,4.1495194265607));
#36821=CARTESIAN_POINT('Ctrl Pts',(38.9693587283608,2.20949972980517,6.60715029962298));
#36822=CARTESIAN_POINT('Ctrl Pts',(39.0686145305819,-1.22035097886095,6.87944858919891));
#36823=CARTESIAN_POINT('Ctrl Pts',(39.1678703328029,-4.34727009921643,5.44403956839734));
#36824=CARTESIAN_POINT('Ctrl Pts',(39.300211402431,-7.16018190988124,1.79631912273862));
#36825=CARTESIAN_POINT('Ctrl Pts',(39.465637739466,-6.53519514424037,-4.46580076226038));
#36826=CARTESIAN_POINT('Ctrl Pts',(39.6641493439083,0.219522695062288,-7.91206850493787));
#36827=CARTESIAN_POINT('Ctrl Pts',(39.8626609483503,6.76517028611504,-4.10870895055163));
#36828=CARTESIAN_POINT('Ctrl Pts',(40.0611725527925,7.11598974632188,3.46624320435687));
#36829=CARTESIAN_POINT('Ctrl Pts',(40.2265988898275,1.98505039136329,7.11017175017984));
#36830=CARTESIAN_POINT('Ctrl Pts',(40.3589399594556,-2.57696043924608,6.47268097718231));
#36831=CARTESIAN_POINT('Ctrl Pts',(40.4581957616766,-5.37244500929141,4.46686736149371));
#36832=CARTESIAN_POINT('Ctrl Pts',(40.5574515638977,-6.83431054025086,1.35222911417895));
#36833=CARTESIAN_POINT('Ctrl Pts',(40.6897926335258,-6.62840083232579,-3.24950300497319));
#36834=CARTESIAN_POINT('Ctrl Pts',(40.8552189705609,-2.10915128084571,-7.62913054653119));
#36835=CARTESIAN_POINT('Ctrl Pts',(41.053730575003,5.27451364338199,-5.90156962733256));
#36836=CARTESIAN_POINT('Ctrl Pts',(41.2522421794451,7.81922095656082,1.22833296502099));
#36837=CARTESIAN_POINT('Ctrl Pts',(41.4507537838873,3.197927895255,7.24053928918684));
#36838=CARTESIAN_POINT('Ctrl Pts',(41.6161801209223,-3.07307048586679,6.71201945484378));
#36839=CARTESIAN_POINT('Ctrl Pts',(41.7485211905504,-6.14607918106869,3.28055404434237));
#36840=CARTESIAN_POINT('Ctrl Pts',(41.8477769927714,-6.98662663108923,-0.0558365542697342));
#36841=CARTESIAN_POINT('Ctrl Pts',(41.9470327949925,-6.09286162596302,-3.37836666818218));
#36842=CARTESIAN_POINT('Ctrl Pts',(42.0793738646206,-2.9654009721384,-6.76027842975032));
#36843=CARTESIAN_POINT('Ctrl Pts',(42.2448002016556,3.31324362906204,-7.18850253362882));
#36844=CARTESIAN_POINT('Ctrl Pts',(42.4433118060978,7.83785440228319,-1.10320288663825));
#36845=CARTESIAN_POINT('Ctrl Pts',(42.6418234105398,5.17951620332599,5.98511738731672));
#36846=CARTESIAN_POINT('Ctrl Pts',(42.840335014982,-2.23081687080563,7.59444587250693));
#36847=CARTESIAN_POINT('Ctrl Pts',(43.005761352017,-6.67949037682418,3.14314741608154));
#36848=CARTESIAN_POINT('Ctrl Pts',(43.1381024216452,-6.81182513990394,-1.46128792549235));
#36849=CARTESIAN_POINT('Ctrl Pts',(43.2373582238662,-5.3003656441942,-4.5521635999691));
#36850=CARTESIAN_POINT('Ctrl Pts',(43.3366140260873,-2.47317959847062,-6.51304128741142));
#36851=CARTESIAN_POINT('Ctrl Pts',(43.4689550957153,2.09843740956863,-7.07753684634914));
#36852=CARTESIAN_POINT('Ctrl Pts',(43.6343814327504,7.17048112842823,-3.35206688602163));
#36853=CARTESIAN_POINT('Ctrl Pts',(43.8328930371925,6.69863740392336,4.2163106113326));
#36854=CARTESIAN_POINT('Ctrl Pts',(44.0314046416347,0.0930375100320632,
7.91456646078634));
#36855=CARTESIAN_POINT('Ctrl Pts',(44.2299162460768,-6.60573645894203,4.36077950101958));
#36856=CARTESIAN_POINT('Ctrl Pts',(44.3953425831118,-7.13055707545171,-1.91052955146803));
#36857=CARTESIAN_POINT('Ctrl Pts',(44.52768365274,-4.25970371841246,-5.51282580616876));
#36858=CARTESIAN_POINT('Ctrl Pts',(44.626939454961,-1.11024213000924,-6.89807450059728));
#36859=CARTESIAN_POINT('Ctrl Pts',(44.726195257182,2.31481837844153,-6.57099231567397));
#36860=CARTESIAN_POINT('Ctrl Pts',(44.8585363268101,6.17098591650305,-4.05140718659923));
#36861=CARTESIAN_POINT('Ctrl Pts',(45.0239626638452,7.64042420221512,2.06786605748864));
#36862=CARTESIAN_POINT('Ctrl Pts',(45.2224742682873,2.39502226673733,7.54406300227598));
#36863=CARTESIAN_POINT('Ctrl Pts',(45.4209858727294,-5.03739157284622,6.10521943768569));
#36864=CARTESIAN_POINT('Ctrl Pts',(45.6194974771716,-7.86014378528482,-0.932894257757612));
#36865=CARTESIAN_POINT('Ctrl Pts',(45.7849238142066,-4.21318924362712,-6.06168324565806));
#36866=CARTESIAN_POINT('Ctrl Pts',(45.9172648838348,0.304677466624451,-6.96013618969833));
#36867=CARTESIAN_POINT('Ctrl Pts',(46.0165206860557,3.60435343990901,-5.98537431438118));
#36868=CARTESIAN_POINT('Ctrl Pts',(46.1157764882769,6.00930934388733,-3.52484401744044));
#36869=CARTESIAN_POINT('Ctrl Pts',(46.2481175579048,7.32839584055675,0.888584142001863));
#36870=CARTESIAN_POINT('Ctrl Pts',(46.4135438949401,4.50107442023831,6.51095085874442));
#36871=CARTESIAN_POINT('Ctrl Pts',(46.6120554993821,-3.03998774172088,7.30804301921271));
#36872=CARTESIAN_POINT('Ctrl Pts',(46.8105671038243,-7.78818558123646,1.41180154154107));
#36873=CARTESIAN_POINT('Ctrl Pts',(47.0090787082663,-5.40146397684792,-5.7858740850733));
#36874=CARTESIAN_POINT('Ctrl Pts',(47.1745050453014,0.694465178907303,-7.34933231583605));
#36875=CARTESIAN_POINT('Ctrl Pts',(47.3068461149295,4.72513075256893,-5.11951789809788));
#36876=CARTESIAN_POINT('Ctrl Pts',(47.4061019171506,6.61627298347009,-2.24521740845774));
#36877=CARTESIAN_POINT('Ctrl Pts',(47.5053577193716,6.86503681807585,1.18642050904397));
#36878=CARTESIAN_POINT('Ctrl Pts',(47.6376987889997,5.02391332886568,5.40881338533256));
#36879=CARTESIAN_POINT('Ctrl Pts',(47.8031251260348,-0.764557269425916,
7.87829957562393));
#36880=CARTESIAN_POINT('Ctrl Pts',(48.0016367304769,-7.03892486372586,3.61974515723125));
#36881=CARTESIAN_POINT('Ctrl Pts',(48.200148334919,-6.85988510040067,-3.94854335797116));
#36882=CARTESIAN_POINT('Ctrl Pts',(48.3986599393611,-0.391163364863194,
-7.90563996419626));
#36883=CARTESIAN_POINT('Ctrl Pts',(48.5640862763962,5.27405820819081,-5.16519867864946));
#36884=CARTESIAN_POINT('Ctrl Pts',(48.6964273460243,6.91345919617128,-0.860468523940247));
#36885=CARTESIAN_POINT('Ctrl Pts',(48.7956831482453,6.50270287109063,2.55556740731831));
#36886=CARTESIAN_POINT('Ctrl Pts',(48.8949389504664,4.47776001838488,5.33722674762568));
#36887=CARTESIAN_POINT('Ctrl Pts',(49.0272800200945,0.346162788340026,7.37395000642637));
#36888=CARTESIAN_POINT('Ctrl Pts',(49.1927063571296,-5.66901646168339,5.52398446582457));
#36889=CARTESIAN_POINT('Ctrl Pts',(49.3912179615717,-7.71271398995097,-1.77849969066399));
#36890=CARTESIAN_POINT('Ctrl Pts',(49.5897295660138,-2.69101398775909,-7.44361887512801));
#36891=CARTESIAN_POINT('Ctrl Pts',(49.7882411704559,4.80392059172006,-6.29082657287229));
#36892=CARTESIAN_POINT('Ctrl Pts',(49.9536675074909,7.36221619304494,-0.541054618475516));
#36893=CARTESIAN_POINT('Ctrl Pts',(50.0860085771191,5.83590891040666,3.80506127772645));
#36894=CARTESIAN_POINT('Ctrl Pts',(50.1852643793401,3.31729297670311,6.1491167422447));
#36895=CARTESIAN_POINT('Ctrl Pts',(50.2845201815612,-0.0247850984101731,
6.96675748370172));
#36896=CARTESIAN_POINT('Ctrl Pts',(50.4168612511893,-4.49511308086105,5.85567466339949));
#36897=CARTESIAN_POINT('Ctrl Pts',(50.5822875882243,-7.89546458114876,0.560170571642261));
#36898=CARTESIAN_POINT('Ctrl Pts',(50.7807991926664,-4.74306097661419,-6.33659141909883));
#36899=CARTESIAN_POINT('Ctrl Pts',(50.9793107971086,2.74907679851826,-7.42237125158298));
#36900=CARTESIAN_POINT('Ctrl Pts',(51.1778224015507,7.72965983491366,-1.70426255548574));
#36901=CARTESIAN_POINT('Ctrl Pts',(51.3432487385858,5.97250520035709,4.33868056037944));
#36902=CARTESIAN_POINT('Ctrl Pts',(51.4755898082138,2.00150851007487,6.67310181414272));
#36903=CARTESIAN_POINT('Ctrl Pts',(51.5748456104349,-1.43518721697726,6.8378583675931));
#36904=CARTESIAN_POINT('Ctrl Pts',(51.6741014126559,-4.51562187594898,5.30523168309059));
#36905=CARTESIAN_POINT('Ctrl Pts',(51.806442482284,-7.21292314512711,1.57121197672262));
#36906=CARTESIAN_POINT('Ctrl Pts',(51.9718688193191,-6.39214022313651,-4.66826470856881));
#36907=CARTESIAN_POINT('Ctrl Pts',(52.1703804237613,0.467187014732091,-7.90131346889507));
#36908=CARTESIAN_POINT('Ctrl Pts',(52.3688920282033,6.89051937021597,-3.89483774362364));
#36909=CARTESIAN_POINT('Ctrl Pts',(52.5674036326456,7.00395181794738,3.68738538172778));
#36910=CARTESIAN_POINT('Ctrl Pts',(52.7328299696805,1.76141678409493,7.16884776557682));
#36911=CARTESIAN_POINT('Ctrl Pts',(52.8651710393087,-2.77839310523777,6.38880707883594));
#36912=CARTESIAN_POINT('Ctrl Pts',(52.9644268415297,-5.5096931474724,4.29643466419932));
#36913=CARTESIAN_POINT('Ctrl Pts',(53.0636826437507,-6.87330461061831,1.13754466614294));
#36914=CARTESIAN_POINT('Ctrl Pts',(53.1960237133789,-6.52338941697225,-3.45548229453452));
#36915=CARTESIAN_POINT('Ctrl Pts',(53.3614500504139,-1.86920524799151,-7.69143834158405));
#36916=CARTESIAN_POINT('Ctrl Pts',(53.5599616548561,5.45673852248659,-5.73350005997104));
#36917=CARTESIAN_POINT('Ctrl Pts',(53.7584732592981,7.7769198556102,1.47259492050349));
#36918=CARTESIAN_POINT('Ctrl Pts',(53.9569848637403,2.96961687274043,7.33713347640913));
#36919=CARTESIAN_POINT('Ctrl Pts',(54.1224112007753,-3.28175488390779,6.6124921364985));
#36920=CARTESIAN_POINT('Ctrl Pts',(54.2547522704034,-6.24579764972934,3.08647628477079));
#36921=CARTESIAN_POINT('Ctrl Pts',(54.3540080726245,-6.98145143093807,-0.274600292226041));
#36922=CARTESIAN_POINT('Ctrl Pts',(54.4532638748455,-5.98407741332333,-3.5675119690298));
#36923=CARTESIAN_POINT('Ctrl Pts',(54.5856049444736,-2.7522437004127,-6.84982642019823));
#36924=CARTESIAN_POINT('Ctrl Pts',(54.7510312815086,3.53673163502875,-7.08122033009106));
#36925=CARTESIAN_POINT('Ctrl Pts',(54.9495428859509,7.86855784630405,-0.857213893870046));
#36926=CARTESIAN_POINT('Ctrl Pts',(55.1480544903928,4.98954771636879,6.14438213545968));
#36927=CARTESIAN_POINT('Ctrl Pts',(55.3465660948351,-2.46754816140723,7.52086152595857));
#36928=CARTESIAN_POINT('Ctrl Pts',(55.5119924318701,-6.77464424514777,2.93243290204456));
#36929=CARTESIAN_POINT('Ctrl Pts',(55.6443335014982,-6.76272297486308,-1.67388831857923));
#36930=CARTESIAN_POINT('Ctrl Pts',(55.7435893037193,-5.15521184077243,-4.71591563535623));
#36931=CARTESIAN_POINT('Ctrl Pts',(55.8428451059403,-2.26800614499064,-6.58729627875518));
#36932=CARTESIAN_POINT('Ctrl Pts',(55.9751861755684,2.31904625713534,-7.00835157726648));
#36933=CARTESIAN_POINT('Ctrl Pts',(56.1406125126034,7.27193664698836,-3.12587418551931));
#36934=CARTESIAN_POINT('Ctrl Pts',(56.3391241170457,6.56331528086214,4.42401523104052));
#36935=CARTESIAN_POINT('Ctrl Pts',(56.5376357214876,-0.154858332188795,
7.91359824210381));
#36936=CARTESIAN_POINT('Ctrl Pts',(56.7361473259299,-6.73905750491416,4.151777446705));
#36937=CARTESIAN_POINT('Ctrl Pts',(56.9015736629648,-7.06723026887618,-2.13289092547814));
#36938=CARTESIAN_POINT('Ctrl Pts',(57.033914732593,-4.08497650263706,-5.64351761853546));
#36939=CARTESIAN_POINT('Ctrl Pts',(57.133170534814,-0.893679552924759,-6.92945930500514));
#36940=CARTESIAN_POINT('Ctrl Pts',(57.2324263370351,2.51945830247594,-6.49527936272969));
#36941=CARTESIAN_POINT('Ctrl Pts',(57.3647674066631,6.2948319774138,-3.8561713848629));
#36942=CARTESIAN_POINT('Ctrl Pts',(57.5301937436983,7.5719202245241,2.30611711215016));
#36943=CARTESIAN_POINT('Ctrl Pts',(57.7287053481404,2.15759997642325,7.61536477013516));
#36944=CARTESIAN_POINT('Ctrl Pts',(57.9272169525825,-5.22611018704844,5.94447563316609));
#36945=CARTESIAN_POINT('Ctrl Pts',(58.1257285570246,-7.82707448421245,-1.17858264033489));
#36946=CARTESIAN_POINT('Ctrl Pts',(58.2911548940597,-4.02129698472421,-6.19064923363895));
#36947=CARTESIAN_POINT('Ctrl Pts',(58.4234959636878,0.522489592048809,-6.94718135390302));
#36948=CARTESIAN_POINT('Ctrl Pts',(58.5227517659088,3.79002186327833,-5.86956588504724));
#36949=CARTESIAN_POINT('Ctrl Pts',(58.6220075681298,6.11674500446027,-3.33492948774446));
#36950=CARTESIAN_POINT('Ctrl Pts',(58.754348637758,7.29697494134825,1.11764219616219));
#36951=CARTESIAN_POINT('Ctrl Pts',(58.919774974793,4.29497183500168,6.64871182696699));
#36952=CARTESIAN_POINT('Ctrl Pts',(59.1182865792352,-3.26735326224477,7.20925938638466));
#36953=CARTESIAN_POINT('Ctrl Pts',(59.3167981836772,-7.82857736944446,1.16721660847457));
#36954=CARTESIAN_POINT('Ctrl Pts',(59.5153097881194,-5.21762607811918,-5.95218700398761));
#36955=CARTESIAN_POINT('Ctrl Pts',(59.6807361251544,0.924274080489811,-7.32398011995129));
#36956=CARTESIAN_POINT('Ctrl Pts',(59.8130771947825,4.88313458074863,-4.96903620474978));
#36957=CARTESIAN_POINT('Ctrl Pts',(59.9123329970036,6.68333854791715,-2.03692298748928));
#36958=CARTESIAN_POINT('Ctrl Pts',(60.0115887992246,6.82451622133231,1.40082207385138));
#36959=CARTESIAN_POINT('Ctrl Pts',(60.1439298688527,4.85206852327865,5.56348797237094));
#36960=CARTESIAN_POINT('Ctrl Pts',(60.3093562058879,-1.01089677537493,7.85049296102132));
#36961=CARTESIAN_POINT('Ctrl Pts',(60.5078678103299,-7.14882743815909,3.39754094896599));
#36962=CARTESIAN_POINT('Ctrl Pts',(60.7063794147721,-6.73286921202922,-4.16142889092029));
#36963=CARTESIAN_POINT('Ctrl Pts',(60.9048910192141,-0.143400844275535,
-7.91401214425207));
#36964=CARTESIAN_POINT('Ctrl Pts',(61.0703173562493,5.4332233368635,-4.99750453177072));
#36965=CARTESIAN_POINT('Ctrl Pts',(61.2026584258773,6.9370146190261,-0.643546667488384));
#36966=CARTESIAN_POINT('Ctrl Pts',(61.3019142280984,6.41948418612984,2.75795072237821));
#36967=CARTESIAN_POINT('Ctrl Pts',(61.4011700303195,4.30842486332835,5.47483327005227));
#36968=CARTESIAN_POINT('Ctrl Pts',(61.5335110999474,0.11507258331191,7.3811737328068));
#36969=CARTESIAN_POINT('Ctrl Pts',(61.6989374369827,-5.83922350944862,5.34374595468485));
#36970=CARTESIAN_POINT('Ctrl Pts',(61.8974490414247,-7.65323626838815,-2.01915647256606));
#36971=CARTESIAN_POINT('Ctrl Pts',(62.0959606458669,-2.45659200470146,-7.52423909527826));
#36972=CARTESIAN_POINT('Ctrl Pts',(62.2944722503089,4.9985661312639,-6.13730304391836));
#36973=CARTESIAN_POINT('Ctrl Pts',(62.4598985873441,7.37554884899199,-0.310236280018402));
#36974=CARTESIAN_POINT('Ctrl Pts',(62.592239656972,5.71388848040567,3.98595064837794));
#36975=CARTESIAN_POINT('Ctrl Pts',(62.6914954591932,3.12310207490572,6.24998422660072));
#36976=CARTESIAN_POINT('Ctrl Pts',(62.7907512614142,-0.242941849452053,
6.96256442667514));
#36977=CARTESIAN_POINT('Ctrl Pts',(62.9230923310423,-4.6762829892943,5.71203508194268));
#36978=CARTESIAN_POINT('Ctrl Pts',(63.0885186680774,-7.90913433125535,0.31264380957621));
#36979=CARTESIAN_POINT('Ctrl Pts',(63.2870302725194,-4.54229989580018,-6.48201588219981));
#36980=CARTESIAN_POINT('Ctrl Pts',(63.4855418769616,2.98016526727059,-7.33264162633296));
#36981=CARTESIAN_POINT('Ctrl Pts',(63.6840534814037,7.77923894968028,-1.46136695777802));
#36982=CARTESIAN_POINT('Ctrl Pts',(63.8494798184388,5.83370711288252,4.52358582259813));
#36983=CARTESIAN_POINT('Ctrl Pts',(63.9818208880669,1.79155398304252,6.73250759105857));
#36984=CARTESIAN_POINT('Ctrl Pts',(64.0810766902879,-1.64861566015868,6.78956079640785));
#36985=CARTESIAN_POINT('Ctrl Pts',(64.180332492509,-4.6795442169047,5.16121982285677));
#36986=CARTESIAN_POINT('Ctrl Pts',(64.3126735621371,-7.25858912458045,1.34456360720884));
#36987=CARTESIAN_POINT('Ctrl Pts',(64.4780998991721,-6.24281516352822,-4.86614948964095));
#36988=CARTESIAN_POINT('Ctrl Pts',(64.6766115036143,0.714393064215512,-7.88280792549629));
#36989=CARTESIAN_POINT('Ctrl Pts',(64.8751231080564,7.00910944883397,-3.67714603663721));
#36990=CARTESIAN_POINT('Ctrl Pts',(65.0736347124984,6.88504361663661,3.90491055192439));
#36991=CARTESIAN_POINT('Ctrl Pts',(65.2390610495337,1.53605537881087,7.22049175932465));
#36992=CARTESIAN_POINT('Ctrl Pts',(65.3714021191617,-2.97710040711504,6.2986663115184));
#36993=CARTESIAN_POINT('Ctrl Pts',(65.4706579213827,-5.64153675165296,4.12178753487387));
#36994=CARTESIAN_POINT('Ctrl Pts',(65.5699137236038,-6.90555656170388,0.921744384878935));
#36995=CARTESIAN_POINT('Ctrl Pts',(65.7022547932318,-6.41197911895647,-3.65807205390767));
#36996=CARTESIAN_POINT('Ctrl Pts',(65.8676811302669,-1.62742568595715,-7.74620149858267));
#36997=CARTESIAN_POINT('Ctrl Pts',(66.0661927347091,5.63361081156164,-5.55980642350118));
#36998=CARTESIAN_POINT('Ctrl Pts',(66.2647043391511,7.72699026663113,1.71541238764292));
#36999=CARTESIAN_POINT('Ctrl Pts',(66.4632159435934,2.73839291224447,7.42653056757245));
#37000=CARTESIAN_POINT('Ctrl Pts',(66.6286422806283,-3.48722016361297,6.50647853454183));
#37001=CARTESIAN_POINT('Ctrl Pts',(66.7609833502565,-6.33938952892727,2.88937095647236));
#37002=CARTESIAN_POINT('Ctrl Pts',(66.8602391524775,-6.96942802968025,-0.493094667537342));
#37003=CARTESIAN_POINT('Ctrl Pts',(66.9594949546985,-5.86942333497652,-3.75315785451707));
#37004=CARTESIAN_POINT('Ctrl Pts',(67.0918360243268,-2.53638671842853,-6.93265530775572));
#37005=CARTESIAN_POINT('Ctrl Pts',(67.2572623613616,3.75675041938502,-6.96699208776573));
#37006=CARTESIAN_POINT('Ctrl Pts',(67.4557739658039,7.89154290138557,-0.610384001760516));
#37007=CARTESIAN_POINT('Ctrl Pts',(67.6542855702459,4.79468493537967,6.2976196889886));
#37008=CARTESIAN_POINT('Ctrl Pts',(67.8527971746882,-2.70185904364832,7.43990003111806));
#37009=CARTESIAN_POINT('Ctrl Pts',(68.0182235117231,-6.86315269475213,2.7188416279581));
#37010=CARTESIAN_POINT('Ctrl Pts',(68.1505645813512,-6.70698726885656,-1.88484635754777));
#37011=CARTESIAN_POINT('Ctrl Pts',(68.2498203835723,-5.00500098465436,-4.87504266827532));
#37012=CARTESIAN_POINT('Ctrl Pts',(68.3490761857934,-2.06060840545458,-6.6550880314067));
#37013=CARTESIAN_POINT('Ctrl Pts',(68.4814172554214,2.53738125462533,-6.93229532543533));
#37014=CARTESIAN_POINT('Ctrl Pts',(68.6468435924565,7.36625711755882,-2.89660791997047));
#37015=CARTESIAN_POINT('Ctrl Pts',(68.8453551968987,6.42155828060474,4.62736804226398));
#37016=CARTESIAN_POINT('Ctrl Pts',(69.0438668013406,-0.402608105905313,
7.90488998104792));
#37017=CARTESIAN_POINT('Ctrl Pts',(69.242378405783,-6.86575660957116,3.9386584492253));
#37018=CARTESIAN_POINT('Ctrl Pts',(69.4078047428178,-6.99699134364105,-2.35308206491398));
#37019=CARTESIAN_POINT('Ctrl Pts',(69.5401458124461,-3.9062140072152,-5.76878272593319));
#37020=CARTESIAN_POINT('Ctrl Pts',(69.6394016146671,-0.67630210031753,-6.95380861243962));
#37021=CARTESIAN_POINT('Ctrl Pts',(69.7386574168881,2.72174082037459,-6.41363491508409));
#37022=CARTESIAN_POINT('Ctrl Pts',(69.8709984865163,6.41225712779278,-3.65620280145809));
#37023=CARTESIAN_POINT('Ctrl Pts',(70.0364248235513,7.4964906511866,2.54016968052848));
#37024=CARTESIAN_POINT('Ctrl Pts',(70.2349364279935,1.91722753812611,7.68241290066031));
#37025=CARTESIAN_POINT('Ctrl Pts',(70.4334480324354,-5.40817629061345,5.77201989048123));
#37026=CARTESIAN_POINT('Ctrl Pts',(70.6319596368777,-7.78926927884629,-1.41183502746632));
#37027=CARTESIAN_POINT('Ctrl Pts',(70.8304712413197,-3.02695043533247,-7.31525976480649));
#37028=CARTESIAN_POINT('Ctrl Pts',(70.9958975783549,3.23651895324008,-6.63681545056612));
#37029=CARTESIAN_POINT('Ctrl Pts',(71.1282386479829,6.21430277804793,-3.13408715922093));
#37030=CARTESIAN_POINT('Ctrl Pts',(71.260579717611,7.25906612343537,1.33970346626809));
#37031=CARTESIAN_POINT('Ctrl Pts',(71.4260060546461,4.08917549587174,6.78386515788701));
#37032=CARTESIAN_POINT('Ctrl Pts',(71.6245176590882,-3.50191772613163,7.10041261509974));
#37033=CARTESIAN_POINT('Ctrl Pts',(71.7899439961233,-7.11586513205948,1.95521631953288));
#37034=CARTESIAN_POINT('Ctrl Pts',(71.9222850657513,-6.4629128098114,-2.60461226368976));
#37035=CARTESIAN_POINT('Ctrl Pts',(72.0215408679724,-4.44333502316774,-5.39127437082873));
#37036=CARTESIAN_POINT('Ctrl Pts',(72.1207966701935,-1.3234918693767,-6.84003759421039));
#37037=CARTESIAN_POINT('Ctrl Pts',(72.2531377398215,3.27785032304679,-6.61450544205606));
#37038=CARTESIAN_POINT('Ctrl Pts',(72.4185640768567,7.63789641404816,-2.07674216600752));
#37039=CARTESIAN_POINT('Ctrl Pts',(72.6170756812987,5.87917379908106,5.29954484007954));
#37040=CARTESIAN_POINT('Ctrl Pts',(72.815587285741,-1.26157197373669,7.81392751410292));
#37041=CARTESIAN_POINT('Ctrl Pts',(73.0140988901829,-7.25403793956794,3.16714455742375));
#37042=CARTESIAN_POINT('Ctrl Pts',(73.1795252272182,-6.6989147707515,-3.10155658511558));
#37043=CARTESIAN_POINT('Ctrl Pts',(73.3118662968461,-3.25441148556226,-6.15995869185653));
#37044=CARTESIAN_POINT('Ctrl Pts',(73.4111220990672,0.0855123818222237,
-6.98632677128281));
#37045=CARTESIAN_POINT('Ctrl Pts',(73.5103779012882,3.40421955141891,-6.07845533473538));
#37046=CARTESIAN_POINT('Ctrl Pts',(73.6427189709164,6.77281349086935,-2.93665698018454));
#37047=CARTESIAN_POINT('Ctrl Pts',(73.8081453079514,7.17436363933803,3.34375023752143));
#37048=CARTESIAN_POINT('Ctrl Pts',(74.0066569123935,1.06989784145846,7.84247000558746));
#37049=CARTESIAN_POINT('Ctrl Pts',(74.2051685168357,-6.00706560616107,5.15404498146463));
#37050=CARTESIAN_POINT('Ctrl Pts',(74.4036801212777,-7.58490102008606,-2.26305761715745));
#37051=CARTESIAN_POINT('Ctrl Pts',(74.5691064583128,-3.11474484508245,-6.69278205299726));
#37052=CARTESIAN_POINT('Ctrl Pts',(74.7014475279409,1.4902110483153,-6.8055561970632));
#37053=CARTESIAN_POINT('Ctrl Pts',(74.8007033301619,4.57463825090347,-5.28098043453118));
#37054=CARTESIAN_POINT('Ctrl Pts',(74.8999591323831,6.52348847355142,-2.44549017964904));
#37055=CARTESIAN_POINT('Ctrl Pts',(75.0323002020111,7.06855892447008,2.12848353322983));
#37056=CARTESIAN_POINT('Ctrl Pts',(75.1977265390462,3.3215767601887,7.18465586037287));
#37057=CARTESIAN_POINT('Ctrl Pts',(75.3962381434883,-4.24472807719733,6.68066626805726));
#37058=CARTESIAN_POINT('Ctrl Pts',(75.5947497479305,-7.91489027044559,0.0594159499921341));
#37059=CARTESIAN_POINT('Ctrl Pts',(75.7932613523725,-4.33267928530105,-6.6242012521571));
#37060=CARTESIAN_POINT('Ctrl Pts',(75.9586876894076,1.94080259747868,-7.1223768961395));
#37061=CARTESIAN_POINT('Ctrl Pts',(76.0910287590358,5.53087109503579,-4.23624704999356));
#37062=CARTESIAN_POINT('Ctrl Pts',(76.1902845612566,6.90272852036613,-1.08092940410934));
#37063=CARTESIAN_POINT('Ctrl Pts',(76.289540363478,6.56109978442663,2.34271077106102));
#37064=CARTESIAN_POINT('Ctrl Pts',(76.4218814331058,4.02515656315956,6.18814043273438));
#37065=CARTESIAN_POINT('Ctrl Pts',(76.587307770141,-2.10030357655869,7.63157106419049));
#37066=CARTESIAN_POINT('Ctrl Pts',(76.7858193745831,-7.55416888152773,2.36295381882188));
#37067=CARTESIAN_POINT('Ctrl Pts',(76.9843309790252,-6.08376574105329,-5.06328081864295));
#37068=CARTESIAN_POINT('Ctrl Pts',(77.1828425834674,0.966275376086498,-7.8561099737133));
#37069=CARTESIAN_POINT('Ctrl Pts',(77.3482689205024,6.07952599095048,-4.18740147330903));
#37070=CARTESIAN_POINT('Ctrl Pts',(77.4806099901305,6.95877913506417,0.334241061524722));
#37071=CARTESIAN_POINT('Ctrl Pts',(77.5798657923515,5.97000918027016,3.6297465187709));
#37072=CARTESIAN_POINT('Ctrl Pts',(77.6791215945727,3.49928493975354,6.02422850232547));
#37073=CARTESIAN_POINT('Ctrl Pts',(77.8114626642005,-0.919706818894118,
7.32455505410309));
#37074=CARTESIAN_POINT('Ctrl Pts',(77.9768890012359,-6.53001247368982,4.4733755839371));
#37075=CARTESIAN_POINT('Ctrl Pts',(78.1754006056778,-7.29506335116228,-3.07100454949284));
#37076=CARTESIAN_POINT('Ctrl Pts',(78.37391221012,-1.37870494315477,-7.79411258067252));
#37077=CARTESIAN_POINT('Ctrl Pts',(78.5724238145621,5.80876705622893,-5.37683711004694));
#37078=CARTESIAN_POINT('Ctrl Pts',(78.7378501515972,7.34631594906046,0.725678544458096));
#37079=CARTESIAN_POINT('Ctrl Pts',(78.8701912212252,5.09939956490671,4.74683560019161));
#37080=CARTESIAN_POINT('Ctrl Pts',(78.9694470234464,2.21709152222903,6.62575086953153));
#37081=CARTESIAN_POINT('Ctrl Pts',(79.0687028256673,-1.2155721704975,6.85993501690279));
#37082=CARTESIAN_POINT('Ctrl Pts',(79.2010438952956,-5.43010594047177,5.00089160536001));
#37083=CARTESIAN_POINT('Ctrl Pts',(79.3664702323305,-7.87498068815616,-0.798017031570015));
#37084=CARTESIAN_POINT('Ctrl Pts',(79.5649818367727,-3.58981146310726,-7.05423786810604));
#37085=CARTESIAN_POINT('Ctrl Pts',(79.7634934412146,3.9776482136295,-6.8430499727159));
#37086=CARTESIAN_POINT('Ctrl Pts',(79.9620050456571,7.90723027905429,-0.357577034378644));
#37087=CARTESIAN_POINT('Ctrl Pts',(80.1274313826919,5.14274811428306,5.29595215295085));
#37088=CARTESIAN_POINT('Ctrl Pts',(80.2597724523201,0.831092698151305,6.91705205017979));
#37089=CARTESIAN_POINT('Ctrl Pts',(80.3590282545412,-2.5831675372795,6.49178826498396));
#37090=CARTESIAN_POINT('Ctrl Pts',(80.4582840567621,-5.35619991408986,4.45504731940314));
#37091=CARTESIAN_POINT('Ctrl Pts',(80.5906251263903,-7.37535395809592,0.314835458781826));
#37092=CARTESIAN_POINT('Ctrl Pts',(80.7560514634253,-5.49985289947136,-5.69243094869711));
#37093=CARTESIAN_POINT('Ctrl Pts',(80.9545630678674,1.81124690432845,-7.70508941492813));
#37094=CARTESIAN_POINT('Ctrl Pts',(81.1530746723097,7.45498302009343,-2.65936955134027));
#37095=CARTESIAN_POINT('Ctrl Pts',(81.3515862767515,6.27036297575581,4.83060039475208));
#37096=CARTESIAN_POINT('Ctrl Pts',(81.5170126137868,0.509775375194911,7.36444814226785));
#37097=CARTESIAN_POINT('Ctrl Pts',(81.6493536834148,-3.82981762340274,5.81969252704047));
#37098=CARTESIAN_POINT('Ctrl Pts',(81.7486094856359,-6.16315297181846,3.29114187615832));
#37099=CARTESIAN_POINT('Ctrl Pts',(81.8478652878569,-6.96658933945347,-0.0543793456253106));
#37100=CARTESIAN_POINT('Ctrl Pts',(81.980206357485,-5.83652679283063,-4.51994716450058));
#37101=CARTESIAN_POINT('Ctrl Pts',(82.1456326945201,-0.526625940840279,
-7.8977729227892));
#37102=CARTESIAN_POINT('Ctrl Pts',(82.3441442989623,6.35668255517161,-4.71610062798219));
#37103=CARTESIAN_POINT('Ctrl Pts',(82.5426559034043,7.41062632852998,2.78058189222602));
#37104=CARTESIAN_POINT('Ctrl Pts',(82.7411675078465,1.67141193306518,7.73682972356996));
#37105=CARTESIAN_POINT('Ctrl Pts',(82.9065938448815,-4.36401234628641,5.9540207939481));
#37106=CARTESIAN_POINT('Ctrl Pts',(83.0389349145097,-6.68154392307749,1.97314341643064));
#37107=CARTESIAN_POINT('Ctrl Pts',(83.1381907167306,-6.83170006191115,-1.46422118107929));
#37108=CARTESIAN_POINT('Ctrl Pts',(83.2374465189518,-5.28600165851457,-4.5381175176496));
#37109=CARTESIAN_POINT('Ctrl Pts',(83.3697875885797,-1.54055762886207,-7.2195325032485));
#37110=CARTESIAN_POINT('Ctrl Pts',(83.5352139256149,4.69537611137566,-6.37225197196651));
#37111=CARTESIAN_POINT('Ctrl Pts',(83.733725530057,7.89925758918072,0.500747221907372));
#37112=CARTESIAN_POINT('Ctrl Pts',(83.9322371344991,3.86553198727663,6.90700229447031));
#37113=CARTESIAN_POINT('Ctrl Pts',(84.1307487389412,-3.71710458261341,6.98822477768299));
#37114=CARTESIAN_POINT('Ctrl Pts',(84.2961750759764,-7.17626550279582,1.73094795031224));
#37115=CARTESIAN_POINT('Ctrl Pts',(84.4285161456044,-6.3769469468741,-2.8055074005553));
#37116=CARTESIAN_POINT('Ctrl Pts',(84.5277719478254,-4.27299097177398,-5.52789449593384));
#37117=CARTESIAN_POINT('Ctrl Pts',(84.6270277500466,-1.1083369152707,-6.87807483385178));
#37118=CARTESIAN_POINT('Ctrl Pts',(84.7593688196745,3.48316218043484,-6.50865182646114));
#37119=CARTESIAN_POINT('Ctrl Pts',(84.9247951567098,7.69930924419873,-1.83651550053466));
#37120=CARTESIAN_POINT('Ctrl Pts',(85.1233067611518,5.71026835033156,5.48104493757155));
#37121=CARTESIAN_POINT('Ctrl Pts',(85.3218183655939,-1.5056176378391,7.770594170918));
#37122=CARTESIAN_POINT('Ctrl Pts',(85.5203299700361,-7.34968207461022,2.9384222677589));
#37123=CARTESIAN_POINT('Ctrl Pts',(85.685756307071,-6.59849172823567,-3.30981484160565));
#37124=CARTESIAN_POINT('Ctrl Pts',(85.8180973766992,-3.05991657066862,-6.25885250811717));
#37125=CARTESIAN_POINT('Ctrl Pts',(85.9173531789202,0.304254704681881,-6.98022195046236));
#37126=CARTESIAN_POINT('Ctrl Pts',(86.0166089811413,3.5928998711205,-5.9688687918164));
#37127=CARTESIAN_POINT('Ctrl Pts',(86.1489500507693,6.86145602376702,-2.72312111504753));
#37128=CARTESIAN_POINT('Ctrl Pts',(86.3143763878044,7.06613256296911,3.56678042834934));
#37129=CARTESIAN_POINT('Ctrl Pts',(86.5128879922466,0.823780881558363,7.87212825731745));
#37130=CARTESIAN_POINT('Ctrl Pts',(86.7113995966886,-6.16552207028737,4.96340164013314));
#37131=CARTESIAN_POINT('Ctrl Pts',(86.9099112011308,-7.51031163519052,-2.4994741774684));
#37132=CARTESIAN_POINT('Ctrl Pts',(87.0753375381659,-2.90362806138492,-6.78703996263797));
#37133=CARTESIAN_POINT('Ctrl Pts',(87.2076786077939,1.70260095722469,-6.75555135560928));
#37134=CARTESIAN_POINT('Ctrl Pts',(87.3069344100151,4.73777219237801,-5.1351323309305));
#37135=CARTESIAN_POINT('Ctrl Pts',(87.4061902122361,6.59687123178447,-2.2400031448799));
#37136=CARTESIAN_POINT('Ctrl Pts',(87.5385312818641,6.99843714004682,2.34879649397724));
#37137=CARTESIAN_POINT('Ctrl Pts',(87.7039576188994,3.09495512387445,7.28514960743508));
#37138=CARTESIAN_POINT('Ctrl Pts',(87.9024692233413,-4.45185598151977,6.54446304598655));
#37139=CARTESIAN_POINT('Ctrl Pts',(88.1009808277835,-7.91286900967269,-0.188473542542395));
#37140=CARTESIAN_POINT('Ctrl Pts',(88.2994924322255,-4.12311277525013,-6.75663326399157));
#37141=CARTESIAN_POINT('Ctrl Pts',(88.4649187692607,2.16289295594546,-7.05810607985089));
#37142=CARTESIAN_POINT('Ctrl Pts',(88.5972598388886,5.66081949484133,-4.06096623781112));
#37143=CARTESIAN_POINT('Ctrl Pts',(88.6965156411099,6.93319309360078,-0.864235459746917));
#37144=CARTESIAN_POINT('Ctrl Pts',(88.7957714433308,6.48451821344733,2.54702722350721));
#37145=CARTESIAN_POINT('Ctrl Pts',(88.9281125129589,3.82939643050207,6.31115602337365));
#37146=CARTESIAN_POINT('Ctrl Pts',(89.093538849994,-2.33826147978246,7.56205562487302));
#37147=CARTESIAN_POINT('Ctrl Pts',(89.2920504544362,-7.62446144690003,2.12523078398847));
#37148=CARTESIAN_POINT('Ctrl Pts',(89.4905620588781,-5.92222171872122,-5.25131489769799));
#37149=CARTESIAN_POINT('Ctrl Pts',(89.6890736633205,1.21182106502083,-7.82199729786965));
#37150=CARTESIAN_POINT('Ctrl Pts',(89.8545000003553,6.20767566568141,-3.99496310408662));
#37151=CARTESIAN_POINT('Ctrl Pts',(89.9868410699837,6.94489916009337,0.551996190160592));
#37152=CARTESIAN_POINT('Ctrl Pts',(90.0860968722044,5.85341308476034,3.81492131795592));
#37153=CARTESIAN_POINT('Ctrl Pts',(90.1853526744257,3.30891574175122,6.13085644521284));
#37154=CARTESIAN_POINT('Ctrl Pts',(90.3176937440536,-1.14862933179586,7.29216141013383));
#37155=CARTESIAN_POINT('Ctrl Pts',(90.4831200810889,-6.66689668448537,4.26668965591664));
#37156=CARTESIAN_POINT('Ctrl Pts',(90.6816316855308,-7.19531477116699,-3.29794839018185));
#37157=CARTESIAN_POINT('Ctrl Pts',(90.8801432899731,-1.13395063439024,-7.83346501870296));
#37158=CARTESIAN_POINT('Ctrl Pts',(91.0786548944152,5.97429753948523,-5.1922943802532));
#37159=CARTESIAN_POINT('Ctrl Pts',(91.2440812314501,7.31998776409361,0.955377677584506));
#37160=CARTESIAN_POINT('Ctrl Pts',(91.3764223010784,4.94824803617576,4.90419876333531));
#37161=CARTESIAN_POINT('Ctrl Pts',(91.4756781032993,2.00851408913216,6.691931003589));
#37162=CARTESIAN_POINT('Ctrl Pts',(91.5749339055204,-1.42979967118216,6.81850401760568));
#37163=CARTESIAN_POINT('Ctrl Pts',(91.7072749751485,-5.58404914297759,4.82839129960669));
#37164=CARTESIAN_POINT('Ctrl Pts',(91.8727013121836,-7.84612788535665,-1.04423619365413));
#37165=CARTESIAN_POINT('Ctrl Pts',(92.0712129166257,-3.36714239853421,-7.1631955375008));
#37166=CARTESIAN_POINT('Ctrl Pts',(92.2697245210679,4.18999226804572,-6.71513090223818));
#37167=CARTESIAN_POINT('Ctrl Pts',(92.4682361255099,7.91454989958454,-0.109781184610879));
#37168=CARTESIAN_POINT('Ctrl Pts',(92.633662462545,4.97437935417045,5.45440348838535));
#37169=CARTESIAN_POINT('Ctrl Pts',(92.7660035321731,0.614072736527218,6.93968578626373));
#37170=CARTESIAN_POINT('Ctrl Pts',(92.8652593343941,-2.78519551710407,6.40771061569896));
#37171=CARTESIAN_POINT('Ctrl Pts',(92.9645151366152,-5.49308586686432,4.28512914590364));
#37172=CARTESIAN_POINT('Ctrl Pts',(93.0968562062433,-7.38159595855551,0.0837166527253544));
#37173=CARTESIAN_POINT('Ctrl Pts',(93.2622825432784,-5.31889298270758,-5.86187081570485));
#37174=CARTESIAN_POINT('Ctrl Pts',(93.4607941477204,2.05164885620794,-7.64458993087906));
#37175=CARTESIAN_POINT('Ctrl Pts',(93.6593057521627,7.53460669885321,-2.42460721232809));
#37176=CARTESIAN_POINT('Ctrl Pts',(93.8578173566046,6.11601398653092,5.02459201707624));
#37177=CARTESIAN_POINT('Ctrl Pts',(94.0232436936398,0.278902482799911,7.37680017205256));
#37178=CARTESIAN_POINT('Ctrl Pts',(94.1555847632679,-4.01018702469117,5.69690478811222));
#37179=CARTESIAN_POINT('Ctrl Pts',(94.2548405654889,-6.26319463191549,3.09652424595433));
#37180=CARTESIAN_POINT('Ctrl Pts',(94.3540963677101,-6.96146960024302,-0.27251631640912));
#37181=CARTESIAN_POINT('Ctrl Pts',(94.486437437338,-5.69211890579575,-4.70050526386146));
#37182=CARTESIAN_POINT('Ctrl Pts',(94.6518637743733,-0.279043343629097,
-7.91039106706398));
#37183=CARTESIAN_POINT('Ctrl Pts',(94.8503753788152,6.50125288217034,-4.51472360201029));
#37184=CARTESIAN_POINT('Ctrl Pts',(95.0488869832574,7.31991585950621,3.01128710856776));
#37185=CARTESIAN_POINT('Ctrl Pts',(95.2473985876994,1.42830791706925,7.78537658148567));
#37186=CARTESIAN_POINT('Ctrl Pts',(95.4128249247347,-4.5483263321779,5.81443848959844));
#37187=CARTESIAN_POINT('Ctrl Pts',(95.5451659943625,-6.74005728665945,1.76293843067934));
#37188=CARTESIAN_POINT('Ctrl Pts',(95.6444217965838,-6.78249629211747,-1.67744253268196));
#37189=CARTESIAN_POINT('Ctrl Pts',(95.7436775988047,-5.14129476294861,-4.70142662372754));
#37190=CARTESIAN_POINT('Ctrl Pts',(95.8760186684329,-1.3137173172897,-7.26423527864844));
#37191=CARTESIAN_POINT('Ctrl Pts',(96.0414450054678,4.89262478090952,-6.22208765405457));
#37192=CARTESIAN_POINT('Ctrl Pts',(96.2399566099102,7.87970209262807,0.747872430237851));
#37193=CARTESIAN_POINT('Ctrl Pts',(96.4384682143521,3.64733847914141,7.02466655856714));
#37194=CARTESIAN_POINT('Ctrl Pts',(96.6369798187943,-3.93412267350125,6.8683936121448));
#37195=CARTESIAN_POINT('Ctrl Pts',(96.8024061558295,-7.22695170552315,1.50536919702228));
#37196=CARTESIAN_POINT('Ctrl Pts',(96.9347472254574,-6.28596289321945,-3.00382999566979));
#37197=CARTESIAN_POINT('Ctrl Pts',(97.0340030276785,-4.0977853525626,-5.65899501743564));
#37198=CARTESIAN_POINT('Ctrl Pts',(97.1332588298995,-0.89240157623222,-6.90940978409554));
#37199=CARTESIAN_POINT('Ctrl Pts',(97.2655998995276,3.68527684596027,-6.39638194153036));
#37200=CARTESIAN_POINT('Ctrl Pts',(97.4310262365628,7.75304483854773,-1.59450548853764));
#37201=CARTESIAN_POINT('Ctrl Pts',(97.6295378410048,5.53582493536608,5.65717778803673));
#37202=CARTESIAN_POINT('Ctrl Pts',(97.8280494454469,-1.74822081517287,7.71963355489581));
#37203=CARTESIAN_POINT('Ctrl Pts',(98.0265610498892,-7.43809613088684,2.70682063853417));
#37204=CARTESIAN_POINT('Ctrl Pts',(98.191987386924,-6.49160627445521,-3.51482792619504));
#37205=CARTESIAN_POINT('Ctrl Pts',(98.3243284565523,-2.86241544827032,-6.35160624876261));
#37206=CARTESIAN_POINT('Ctrl Pts',(98.4235842587731,0.522696037167918,-6.96727050255458));
#37207=CARTESIAN_POINT('Ctrl Pts',(98.5228400609945,3.77805702993185,-5.85342713428637));
#37208=CARTESIAN_POINT('Ctrl Pts',(98.6551811306222,6.94336722695929,-2.50691422368103));
#37209=CARTESIAN_POINT('Ctrl Pts',(98.8206074676577,6.95097069356383,3.78631198380759));
#37210=CARTESIAN_POINT('Ctrl Pts',(99.0191190720994,0.576855623380361,7.89406459501387));
#37211=CARTESIAN_POINT('Ctrl Pts',(99.2176306765419,-6.31793055827079,4.76788964861238));
#37212=CARTESIAN_POINT('Ctrl Pts',(99.4161422809836,-7.42835536047989,-2.73343898046748));
#37213=CARTESIAN_POINT('Ctrl Pts',(99.581568618019,-2.68966303039799,-6.87464036559134));
#37214=CARTESIAN_POINT('Ctrl Pts',(99.713909687647,1.91332074356496,-6.69891990324268));
#37215=CARTESIAN_POINT('Ctrl Pts',(99.8131654898681,4.89625879741496,-4.98424710380356));
#37216=CARTESIAN_POINT('Ctrl Pts',(99.9124212920891,6.6637830236258,-2.03231886077308));
#37217=CARTESIAN_POINT('Ctrl Pts',(100.044762361717,6.92145049527186,2.5668054883079));
#37218=CARTESIAN_POINT('Ctrl Pts',(100.210188698752,2.86529760159607,7.37849725051084));
#37219=CARTESIAN_POINT('Ctrl Pts',(100.408700303194,-4.65461699799906,6.40184026998606));
#37220=CARTESIAN_POINT('Ctrl Pts',(100.607211907637,-7.90308590705035,-0.436178158851584));
#37221=CARTESIAN_POINT('Ctrl Pts',(100.805723512079,-3.90950184671483,-6.88243760102782));
#37222=CARTESIAN_POINT('Ctrl Pts',(100.971149849114,2.38286170273553,-6.9869118699854));
#37223=CARTESIAN_POINT('Ctrl Pts',(101.103490918742,5.7852151187988,-3.88170196782793));
#37224=CARTESIAN_POINT('Ctrl Pts',(101.202746720963,6.95685680207187,-0.6466937749077));
#37225=CARTESIAN_POINT('Ctrl Pts',(101.302002523184,6.40157588913561,2.74884526182444));
#37226=CARTESIAN_POINT('Ctrl Pts',(101.434343592812,3.6298799900591,6.42798091402542));
#37227=CARTESIAN_POINT('Ctrl Pts',(101.599769929847,-2.57392575006508,7.48512246089938));
#37228=CARTESIAN_POINT('Ctrl Pts',(101.798281534289,-7.68727507288713,1.88542308096755));
#37229=CARTESIAN_POINT('Ctrl Pts',(101.996793138731,-5.75486850742494,-5.43419788954419));
#37230=CARTESIAN_POINT('Ctrl Pts',(102.195304743174,1.45617806195801,-7.78021191699693));
#37231=CARTESIAN_POINT('Ctrl Pts',(102.360731080208,6.3297361457371,-3.79860602045742));
#37232=CARTESIAN_POINT('Ctrl Pts',(102.493072149837,6.92420683775317,0.769209858120306));
#37233=CARTESIAN_POINT('Ctrl Pts',(102.592327952058,5.73107529562657,3.99635400820522));
#37234=CARTESIAN_POINT('Ctrl Pts',(102.691583754279,3.11530078266195,6.2314705464568));
#37235=CARTESIAN_POINT('Ctrl Pts',(102.823924823907,-1.37642513834393,7.25261478446579));
#37236=CARTESIAN_POINT('Ctrl Pts',(102.989351160942,-6.79724124437457,4.05581847316578));
#37237=CARTESIAN_POINT('Ctrl Pts',(103.187862765384,-7.08850820767564,-3.52165722780795));
#37238=CARTESIAN_POINT('Ctrl Pts',(103.386374369826,-0.888084017809581,
-7.86513350286279));
#37239=CARTESIAN_POINT('Ctrl Pts',(103.584885974268,6.13396775188958,-5.00265845728224));
#37240=CARTESIAN_POINT('Ctrl Pts',(103.750312311303,7.28647930217096,1.18413966755644));
#37241=CARTESIAN_POINT('Ctrl Pts',(103.882653380931,4.792242702703,5.05675133029455));
#37242=CARTESIAN_POINT('Ctrl Pts',(103.981909183152,1.79796647685818,6.75154693018687));
#37243=CARTESIAN_POINT('Ctrl Pts',(104.081164985374,-1.64262466163945,6.77038465375933));
#37244=CARTESIAN_POINT('Ctrl Pts',(104.213506055001,-5.73251487468722,4.65115475805918));
#37245=CARTESIAN_POINT('Ctrl Pts',(104.378932392037,-7.80957870745604,-1.28943104969529));
#37246=CARTESIAN_POINT('Ctrl Pts',(104.577443996479,-3.14117045761931,-7.26512673019593));
#37247=CARTESIAN_POINT('Ctrl Pts',(104.775955600921,4.39822630139848,-6.58062486614574));
#37248=CARTESIAN_POINT('Ctrl Pts',(104.974467205363,7.91410602868588,0.138122348868092));
#37249=CARTESIAN_POINT('Ctrl Pts',(105.139893542398,4.80113115722892,5.60750452802011));
#37250=CARTESIAN_POINT('Ctrl Pts',(105.272234612026,0.396450421808572,6.95551228352529));
#37251=CARTESIAN_POINT('Ctrl Pts',(105.371490414247,-2.98449145875099,6.31734756632467));
#37252=CARTESIAN_POINT('Ctrl Pts',(105.470746216468,-5.62458357868699,4.11100760866382));
#37253=CARTESIAN_POINT('Ctrl Pts',(105.603087286096,-7.38059724382454,-0.147484225780056));
#37254=CARTESIAN_POINT('Ctrl Pts',(105.768513623131,-5.13271570250706,-6.02556078732482));
#37255=CARTESIAN_POINT('Ctrl Pts',(105.967025227573,2.29003833747114,-7.57659160585189));
#37256=CARTESIAN_POINT('Ctrl Pts',(106.165536832016,7.60683954109075,-2.18746683219334));
#37257=CARTESIAN_POINT('Ctrl Pts',(106.364048436458,5.95566578760469,5.2136555188432));
#37258=CARTESIAN_POINT('Ctrl Pts',(106.529474773493,0.0477558832100018,
7.38191519310475));
#37259=CARTESIAN_POINT('Ctrl Pts',(106.661815843121,-4.1866225994409,5.56853027965365));
#37260=CARTESIAN_POINT('Ctrl Pts',(106.761071645342,-6.35709302850648,2.89886612808133));
#37261=CARTESIAN_POINT('Ctrl Pts',(106.860327447563,-6.94952053876253,-0.490380316337293));
#37262=CARTESIAN_POINT('Ctrl Pts',(106.992668517191,-5.54212909806882,-4.87646479313282));
#37263=CARTESIAN_POINT('Ctrl Pts',(107.158094854226,-0.0311838539981387,
-7.91522488447879));
#37264=CARTESIAN_POINT('Ctrl Pts',(107.356606458668,6.63944075859768,-4.30895947104066));
#37265=CARTESIAN_POINT('Ctrl Pts',(107.55511806311,7.22203490733478,3.23911481438212));
#37266=CARTESIAN_POINT('Ctrl Pts',(107.753629667553,1.18378367673741,7.82613616286123));
#37267=CARTESIAN_POINT('Ctrl Pts',(107.919056004588,-4.72814509520211,5.66941723656927));
#37268=CARTESIAN_POINT('Ctrl Pts',(108.051397074216,-6.79200634781696,1.55063442080293));
#37269=CARTESIAN_POINT('Ctrl Pts',(108.150652876437,-6.72653659654391,-1.88821083607211));
#37270=CARTESIAN_POINT('Ctrl Pts',(108.249908678658,-4.99173439974838,-4.86161506097717));
#37271=CARTESIAN_POINT('Ctrl Pts',(108.382249748286,-1.08518063725679,-7.29858638145808));
#37272=CARTESIAN_POINT('Ctrl Pts',(108.547676085321,5.08426806181123,-6.07244981975362));
#37273=CARTESIAN_POINT('Ctrl Pts',(108.746187689763,7.85362119325993,1.00557868191725));
#37274=CARTESIAN_POINT('Ctrl Pts',(108.911614026798,4.16266766862485,6.094569780456));
#37275=CARTESIAN_POINT('Ctrl Pts',(109.043955096426,-0.366836423285678,
6.95826883443441));
#37276=CARTESIAN_POINT('Ctrl Pts',(109.143210898647,-3.64721232954971,5.9546908966592));
#37277=CARTESIAN_POINT('Ctrl Pts',(109.242466700868,-6.05449046306688,3.4721993705992));
#37278=CARTESIAN_POINT('Ctrl Pts',(109.308637235682,-6.66841279098075,1.26337808959281));
#37279=CARTESIAN_POINT('Ctrl Pts',(109.341722503089,-6.69339752173825,0.15023467065256));
#37280=CARTESIAN_POINT('Ctrl Pts',(31.067,0.728796816009639,-6.89458803707475));
#37281=CARTESIAN_POINT('Ctrl Pts',(31.100085267407,1.87539916180617,-6.77338570644206));
#37282=CARTESIAN_POINT('Ctrl Pts',(31.166255802221,4.10223773170205,-5.95048895222621));
#37283=CARTESIAN_POINT('Ctrl Pts',(31.2655116044422,6.457772812735,-3.25342220167339));
#37284=CARTESIAN_POINT('Ctrl Pts',(31.3647674066631,7.21225375876819,0.217893466371651));
#37285=CARTESIAN_POINT('Ctrl Pts',(31.4971084762913,5.93266321869853,4.81822422049041));
#37286=CARTESIAN_POINT('Ctrl Pts',(31.6625348133263,0.364527573010722,8.19099424626465));
#37287=CARTESIAN_POINT('Ctrl Pts',(31.8610464177684,-6.70248217457009,4.72634364857896));
#37288=CARTESIAN_POINT('Ctrl Pts',(32.0264727548035,-7.43898861096156,-1.74552100244657));
#37289=CARTESIAN_POINT('Ctrl Pts',(32.1588138244316,-4.58920855911997,-5.56811746148175));
#37290=CARTESIAN_POINT('Ctrl Pts',(32.2580696266526,-1.37200169140237,-7.10352230210452));
#37291=CARTESIAN_POINT('Ctrl Pts',(32.3573254288737,2.18243696783098,-6.87630845685192));
#37292=CARTESIAN_POINT('Ctrl Pts',(32.4896664985018,6.25603295742458,-4.39337904789581));
#37293=CARTESIAN_POINT('Ctrl Pts',(32.6550928355369,7.97495827693072,1.89249908165876));
#37294=CARTESIAN_POINT('Ctrl Pts',(32.853604439979,2.72363629353246,7.73066701466195));
#37295=CARTESIAN_POINT('Ctrl Pts',(33.0521160444211,-5.01590101849566,6.48242017314943));
#37296=CARTESIAN_POINT('Ctrl Pts',(33.2506276488632,-8.16569697464416,-0.710673422495908));
#37297=CARTESIAN_POINT('Ctrl Pts',(33.4160539858983,-4.55735344058351,-6.13738783143792));
#37298=CARTESIAN_POINT('Ctrl Pts',(33.5483950555264,0.0896484826078498,
-7.21381584413317));
#37299=CARTESIAN_POINT('Ctrl Pts',(33.6476508577474,3.53650717330565,-6.31191543516737));
#37300=CARTESIAN_POINT('Ctrl Pts',(33.7469066599685,6.10550017679619,-3.84318556859557));
#37301=CARTESIAN_POINT('Ctrl Pts',(33.8792477295966,7.61391039016358,0.682060208615401));
#37302=CARTESIAN_POINT('Ctrl Pts',(34.0446740666317,4.86987989748413,6.59305422815555));
#37303=CARTESIAN_POINT('Ctrl Pts',(34.2431856710737,-2.9094840048122,7.66261248374723));
#37304=CARTESIAN_POINT('Ctrl Pts',(34.4416972755159,-8.01520842963098,1.71381383651624));
#37305=CARTESIAN_POINT('Ctrl Pts',(34.640208879958,-5.77829476061933,-5.81338094144534));
#37306=CARTESIAN_POINT('Ctrl Pts',(34.8056352169931,0.480462945019444,-7.62928625176653));
#37307=CARTESIAN_POINT('Ctrl Pts',(34.9379762866211,4.72462479779841,-5.45207418673285));
#37308=CARTESIAN_POINT('Ctrl Pts',(35.0372320888422,6.77521962502725,-2.53841926317347));
#37309=CARTESIAN_POINT('Ctrl Pts',(35.1364878910633,7.14398017959929,1.00535550296516));
#37310=CARTESIAN_POINT('Ctrl Pts',(35.2688289606914,5.3752915948991,5.43535590203058));
#37311=CARTESIAN_POINT('Ctrl Pts',(35.4342552977264,-0.535856550938932,
8.17905524544786));
#37312=CARTESIAN_POINT('Ctrl Pts',(35.6327669021686,-7.16810227628201,3.97480015051313));
#37313=CARTESIAN_POINT('Ctrl Pts',(35.8312785066107,-7.22821962006094,-3.86439744694054));
#37314=CARTESIAN_POINT('Ctrl Pts',(36.0297901110528,-0.66123344041058,-8.16987498632177));
#37315=CARTESIAN_POINT('Ctrl Pts',(36.1952164480879,5.29129882300858,-5.51715599066038));
#37316=CARTESIAN_POINT('Ctrl Pts',(36.327557517716,7.12772108930233,-1.11480251529127));
#37317=CARTESIAN_POINT('Ctrl Pts',(36.426813319937,6.81335378601919,2.434211034571));
#37318=CARTESIAN_POINT('Ctrl Pts',(36.5260691221581,4.80768609485547,5.37897267026131));
#37319=CARTESIAN_POINT('Ctrl Pts',(36.6584101917861,0.597414649385422,7.62102022027007));
#37320=CARTESIAN_POINT('Ctrl Pts',(36.8238365288213,-5.68845683170082,5.90131729619776));
#37321=CARTESIAN_POINT('Ctrl Pts',(37.0223481332633,-8.04055017571803,-1.59068518751364));
#37322=CARTESIAN_POINT('Ctrl Pts',(37.2208597377055,-3.02666088894786,-7.61708936256067));
#37323=CARTESIAN_POINT('Ctrl Pts',(37.4193713421476,4.76819069205422,-6.66696666264346));
#37324=CARTESIAN_POINT('Ctrl Pts',(37.5847976791826,7.60255533599256,-0.798752667796797));
#37325=CARTESIAN_POINT('Ctrl Pts',(37.7171387488107,6.16372253201031,3.74909550721544));
#37326=CARTESIAN_POINT('Ctrl Pts',(37.8163945510318,3.63289845491171,6.25693391296819));
#37327=CARTESIAN_POINT('Ctrl Pts',(37.9156503532529,0.200268489030504,7.21159379791598));
#37328=CARTESIAN_POINT('Ctrl Pts',(38.0479914228809,-4.46267756834381,6.20655801407927));
#37329=CARTESIAN_POINT('Ctrl Pts',(38.213417759916,-8.15386252187664,0.835830683175351));
#37330=CARTESIAN_POINT('Ctrl Pts',(38.4119293643581,-5.1146879884136,-6.4047399069065));
#37331=CARTESIAN_POINT('Ctrl Pts',(38.6104409688002,2.60467519869591,-7.77151166783153));
#37332=CARTESIAN_POINT('Ctrl Pts',(38.8089525732423,7.94514871250055,-2.01462127777205));
#37333=CARTESIAN_POINT('Ctrl Pts',(38.9743789102775,6.32240802964781,4.29697686377015));
#37334=CARTESIAN_POINT('Ctrl Pts',(39.1067199799055,2.2880165733667,6.84194217556962));
#37335=CARTESIAN_POINT('Ctrl Pts',(39.2059757821266,-1.26371740502772,7.12391686470159));
#37336=CARTESIAN_POINT('Ctrl Pts',(39.3052315843476,-4.50175480980351,5.6374991092017));
#37337=CARTESIAN_POINT('Ctrl Pts',(39.4375726539757,-7.41462633243902,1.86015316880977));
#37338=CARTESIAN_POINT('Ctrl Pts',(39.6029989910108,-6.76743001979327,-4.62449758177058));
#37339=CARTESIAN_POINT('Ctrl Pts',(39.8015105954529,0.22732365963109,-8.19323199035126));
#37340=CARTESIAN_POINT('Ctrl Pts',(40.000022199895,7.00557756467603,-4.25471614555553));
#37341=CARTESIAN_POINT('Ctrl Pts',(40.1985338043371,7.36886375493194,3.58941971881967));
#37342=CARTESIAN_POINT('Ctrl Pts',(40.3639601413722,2.05559119702074,7.3628390103181));
#37343=CARTESIAN_POINT('Ctrl Pts',(40.4963012110003,-2.66853537675076,6.70269434756417));
#37344=CARTESIAN_POINT('Ctrl Pts',(40.5955570132213,-5.56336036386177,4.62560208370343));
#37345=CARTESIAN_POINT('Ctrl Pts',(40.6948128154424,-7.07717478879668,1.40028196541262));
#37346=CARTESIAN_POINT('Ctrl Pts',(40.8271538850705,-6.86394786779064,-3.36497743371087));
#37347=CARTESIAN_POINT('Ctrl Pts',(40.9925802221056,-2.18410213914716,-7.90023954082243));
#37348=CARTESIAN_POINT('Ctrl Pts',(41.1910918265477,5.46194890622252,-6.11128796897657));
#37349=CARTESIAN_POINT('Ctrl Pts',(41.3896034309898,8.09708500892483,1.27198303926893));
#37350=CARTESIAN_POINT('Ctrl Pts',(41.5881150354319,3.31156954946564,7.49783929380012));
#37351=CARTESIAN_POINT('Ctrl Pts',(41.753541372467,-3.18227520372151,6.95053796399318));
#37352=CARTESIAN_POINT('Ctrl Pts',(41.8858824420951,-6.36448642098304,3.39713190367425));
#37353=CARTESIAN_POINT('Ctrl Pts',(41.9851382443162,-7.23490358845545,-0.0578207636081432));
#37354=CARTESIAN_POINT('Ctrl Pts',(42.0843940465372,-6.30937772536576,-3.49842039962285));
#37355=CARTESIAN_POINT('Ctrl Pts',(42.2167351161653,-3.07077954317236,-7.00051187116809));
#37356=CARTESIAN_POINT('Ctrl Pts',(42.3821614532003,3.43098314638184,-7.44395335865592));
#37357=CARTESIAN_POINT('Ctrl Pts',(42.5806730576425,8.11638061329028,-1.14240633495646));
#37358=CARTESIAN_POINT('Ctrl Pts',(42.7791846620846,5.3635756345066,6.19780468447261));
#37359=CARTESIAN_POINT('Ctrl Pts',(42.9776962665267,-2.31009124088029,7.86432231126175));
#37360=CARTESIAN_POINT('Ctrl Pts',(43.1431226035618,-6.91685293175678,3.25484238966784));
#37361=CARTESIAN_POINT('Ctrl Pts',(43.2754636731899,-7.05389034664051,-1.51321629366424));
#37362=CARTESIAN_POINT('Ctrl Pts',(43.3747194754109,-5.48871958445089,-4.71392941167078));
#37363=CARTESIAN_POINT('Ctrl Pts',(43.473975277632,-2.56106657714424,-6.74448890289501));
#37364=CARTESIAN_POINT('Ctrl Pts',(43.6063163472601,2.17300753944422,-7.32904439164134));
#37365=CARTESIAN_POINT('Ctrl Pts',(43.7717426842951,7.42529154430146,-3.47118602767502));
#37366=CARTESIAN_POINT('Ctrl Pts',(43.9702542887373,6.93668036814076,4.36614154193306));
#37367=CARTESIAN_POINT('Ctrl Pts',(44.1687658931793,0.0963436935637944,
8.19581871362791));
#37368=CARTESIAN_POINT('Ctrl Pts',(44.3672774976216,-6.84047809260716,4.51574428208274));
#37369=CARTESIAN_POINT('Ctrl Pts',(44.5327038346565,-7.38394874907302,-1.9784221824965));
#37370=CARTESIAN_POINT('Ctrl Pts',(44.6650449042847,-4.41107666766695,-5.70872973662297));
#37371=CARTESIAN_POINT('Ctrl Pts',(44.7643007065056,-1.14969572507477,-7.14320466700307));
#37372=CARTESIAN_POINT('Ctrl Pts',(44.8635565087267,2.39707782841684,-6.80449928050194));
#37373=CARTESIAN_POINT('Ctrl Pts',(44.9958975783549,6.3902782428573,-4.19537810453311));
#37374=CARTESIAN_POINT('Ctrl Pts',(45.1613239153898,7.91193452816724,2.14134980295047));
#37375=CARTESIAN_POINT('Ctrl Pts',(45.3598355198321,2.4801318443069,7.81214903395972));
#37376=CARTESIAN_POINT('Ctrl Pts',(45.5583471242741,-5.21640045922418,6.32217468462786));
#37377=CARTESIAN_POINT('Ctrl Pts',(45.7568587287163,-8.1394620724232,-0.966045613925907));
#37378=CARTESIAN_POINT('Ctrl Pts',(45.9222850657513,-4.362909253218,-6.27709138927544));
#37379=CARTESIAN_POINT('Ctrl Pts',(46.0546261353795,0.315504493512712,-7.20747178200597));
#37380=CARTESIAN_POINT('Ctrl Pts',(46.1538819376004,3.73243784352554,-6.19807074170408));
#37381=CARTESIAN_POINT('Ctrl Pts',(46.2531377398216,6.22285632708154,-3.65010297201878));
#37382=CARTESIAN_POINT('Ctrl Pts',(46.3854788094495,7.58881791801145,0.920160892670061));
#37383=CARTESIAN_POINT('Ctrl Pts',(46.5509051464848,4.66102472543446,6.74232418869707));
#37384=CARTESIAN_POINT('Ctrl Pts',(46.7494167509267,-3.14801683026386,7.56774183824466));
#37385=CARTESIAN_POINT('Ctrl Pts',(46.947928355369,-8.06494675964391,1.46197136020253));
#37386=CARTESIAN_POINT('Ctrl Pts',(47.146439959811,-5.59341055025238,-5.99148106672523));
#37387=CARTESIAN_POINT('Ctrl Pts',(47.3118662968461,0.719143712729369,-7.61049839245583));
#37388=CARTESIAN_POINT('Ctrl Pts',(47.4442073664742,4.89304312979347,-5.30144522784307));
#37389=CARTESIAN_POINT('Ctrl Pts',(47.5434631686953,6.85138904336245,-2.32500351643662));
#37390=CARTESIAN_POINT('Ctrl Pts',(47.6427189709163,7.10899295648094,1.22858118109606));
#37391=CARTESIAN_POINT('Ctrl Pts',(47.7750600405444,5.20244325199208,5.60102112752069));
#37392=CARTESIAN_POINT('Ctrl Pts',(47.9404863775795,-0.791726597716949,
8.15826304743041));
#37393=CARTESIAN_POINT('Ctrl Pts',(48.1389979820216,-7.28906029253489,3.74837652134022));
#37394=CARTESIAN_POINT('Ctrl Pts',(48.3375095864638,-7.10365816722376,-4.08885890404384));
#37395=CARTESIAN_POINT('Ctrl Pts',(48.5360211909057,-0.405063757024925,
-8.18657500480791));
#37396=CARTESIAN_POINT('Ctrl Pts',(48.701447527941,5.46147728667374,-5.34874932187685));
#37397=CARTESIAN_POINT('Ctrl Pts',(48.833788597569,7.15913607354485,-0.891046157226271));
#37398=CARTESIAN_POINT('Ctrl Pts',(48.93304439979,6.73378310032549,2.64638212144819));
#37399=CARTESIAN_POINT('Ctrl Pts',(49.0323002020111,4.63688182235142,5.52689058507458));
#37400=CARTESIAN_POINT('Ctrl Pts',(49.1646412716391,0.358464038768738,7.63599089798048));
#37401=CARTESIAN_POINT('Ctrl Pts',(49.3300676086743,-5.87047078759569,5.72028493071691));
#37402=CARTESIAN_POINT('Ctrl Pts',(49.5285792131163,-7.9867932078012,-1.84170050490409));
#37403=CARTESIAN_POINT('Ctrl Pts',(49.7270908175585,-2.78664193532054,-7.70813552152894));
#37404=CARTESIAN_POINT('Ctrl Pts',(49.9256024220006,4.97463284684977,-6.51437756010842));
#37405=CARTESIAN_POINT('Ctrl Pts',(50.0910287590356,7.62384011148192,-0.560281550374918));
#37406=CARTESIAN_POINT('Ctrl Pts',(50.2233698286638,6.04329393099642,3.94027804062365));
#37407=CARTESIAN_POINT('Ctrl Pts',(50.3226256308848,3.43517639175237,6.36763192501709));
#37408=CARTESIAN_POINT('Ctrl Pts',(50.4218814331059,-0.0256658623535902,
7.21432837049636));
#37409=CARTESIAN_POINT('Ctrl Pts',(50.554222502734,-4.65485154373645,6.06376208033474));
#37410=CARTESIAN_POINT('Ctrl Pts',(50.719648839769,-8.17603802906677,0.580076808582549));
#37411=CARTESIAN_POINT('Ctrl Pts',(50.9181604442112,-4.9116105227764,-6.56176870717763));
#37412=CARTESIAN_POINT('Ctrl Pts',(51.1166720486532,2.84676806773059,-7.68613284184527));
#37413=CARTESIAN_POINT('Ctrl Pts',(51.3151836530954,8.00434124077968,-1.76482527683466));
#37414=CARTESIAN_POINT('Ctrl Pts',(51.4806099901304,6.18474431048777,4.49286003287664));
#37415=CARTESIAN_POINT('Ctrl Pts',(51.6129510597586,2.07263417189446,6.91023734493501));
#37416=CARTESIAN_POINT('Ctrl Pts',(51.7122068619796,-1.48618806964884,7.08084869182948));
#37417=CARTESIAN_POINT('Ctrl Pts',(51.8114626642006,-4.67608913993433,5.4937585430402));
#37418=CARTESIAN_POINT('Ctrl Pts',(51.9438037338288,-7.46924178168058,1.62704660902152));
#37419=CARTESIAN_POINT('Ctrl Pts',(52.1092300708638,-6.61929149505301,-4.83415629247963));
#37420=CARTESIAN_POINT('Ctrl Pts',(52.307741675306,0.483788985420524,-8.18209476304991));
#37421=CARTESIAN_POINT('Ctrl Pts',(52.506253279748,7.13538105729948,-4.03324480549778));
#37422=CARTESIAN_POINT('Ctrl Pts',(52.7047648841902,7.25284444363329,3.81842041072731));
#37423=CARTESIAN_POINT('Ctrl Pts',(52.8701912212252,1.82401053969385,7.42360013822247));
#37424=CARTESIAN_POINT('Ctrl Pts',(53.0025322908534,-2.87712615953718,6.61583990404437));
#37425=CARTESIAN_POINT('Ctrl Pts',(53.1017880930744,-5.70548575568047,4.44911288536006));
#37426=CARTESIAN_POINT('Ctrl Pts',(53.2010438952954,-7.11755455352814,1.17796848488831));
#37427=CARTESIAN_POINT('Ctrl Pts',(53.3333849649235,-6.75520476387417,-3.57827640900797));
#37428=CARTESIAN_POINT('Ctrl Pts',(53.4988113019586,-1.93562937742725,-7.96476150740508));
#37429=CARTESIAN_POINT('Ctrl Pts',(53.6973229064007,5.65064933367531,-5.93724587681677));
#37430=CARTESIAN_POINT('Ctrl Pts',(53.8958345108428,8.05328069487987,1.52492509436311));
#37431=CARTESIAN_POINT('Ctrl Pts',(54.094346115285,3.07514526013486,7.59786605473347));
#37432=CARTESIAN_POINT('Ctrl Pts',(54.25977245232,-3.39837541630809,6.84747384010805));
#37433=CARTESIAN_POINT('Ctrl Pts',(54.3921135219481,-6.46774848790643,3.19615739146608));
#37434=CARTESIAN_POINT('Ctrl Pts',(54.4913693241692,-7.22954448224845,-0.284358495812285));
#37435=CARTESIAN_POINT('Ctrl Pts',(54.5906251263902,-6.19672775393435,-3.69428717311731));
#37436=CARTESIAN_POINT('Ctrl Pts',(54.7229661960184,-2.85004750873798,-7.09324204148341));
#37437=CARTESIAN_POINT('Ctrl Pts',(54.8883925330533,3.66241302831517,-7.33285877176346));
#37438=CARTESIAN_POINT('Ctrl Pts',(55.0869041374955,8.1481751357478,-0.887675870531769));
#37439=CARTESIAN_POINT('Ctrl Pts',(55.2854157419376,5.16685642213818,6.36272906911433));
#37440=CARTESIAN_POINT('Ctrl Pts',(55.4839273463797,-2.55523502117791,7.7881230693375));
#37441=CARTESIAN_POINT('Ctrl Pts',(55.6493536834148,-7.01538819057916,3.03663991882703));
#37442=CARTESIAN_POINT('Ctrl Pts',(55.7816947530428,-7.0030432857035,-1.73337166020505));
#37443=CARTESIAN_POINT('Ctrl Pts',(55.880950555264,-5.33840759145258,-4.88350054392042));
#37444=CARTESIAN_POINT('Ctrl Pts',(55.980206357485,-2.34860207414178,-6.82138262166666));
#37445=CARTESIAN_POINT('Ctrl Pts',(56.1125474271131,2.40145594912496,-7.25740055292139));
#37446=CARTESIAN_POINT('Ctrl Pts',(56.2779737641482,7.53035238897762,-3.23695533710616));
#37447=CARTESIAN_POINT('Ctrl Pts',(56.4764853685902,6.79654943436846,4.58122715875659));
#37448=CARTESIAN_POINT('Ctrl Pts',(56.6749969730324,-0.160361382168487,
8.19481608829948));
#37449=CARTESIAN_POINT('Ctrl Pts',(56.8735085774745,-6.97853683895954,4.29931512498043));
#37450=CARTESIAN_POINT('Ctrl Pts',(57.0389349145096,-7.31837155934601,-2.20868539644884));
#37451=CARTESIAN_POINT('Ctrl Pts',(57.1712759841377,-4.23014034071495,-5.84406581685175));
#37452=CARTESIAN_POINT('Ctrl Pts',(57.2705317863588,-0.925437374256124,
-7.17570476268915));
#37453=CARTESIAN_POINT('Ctrl Pts',(57.3697875885798,2.60898984245657,-6.72609578996594));
#37454=CARTESIAN_POINT('Ctrl Pts',(57.5021286582079,6.51852530081687,-3.99320439794175));
#37455=CARTESIAN_POINT('Ctrl Pts',(57.667554995243,7.84099619122865,2.38806735368569));
#37456=CARTESIAN_POINT('Ctrl Pts',(57.8660665996851,2.2342725089119,7.88598458341533));
#37457=CARTESIAN_POINT('Ctrl Pts',(58.0645782041272,-5.41182538332481,6.15571868382113));
#37458=CARTESIAN_POINT('Ctrl Pts',(58.2630898085693,-8.10521761975249,-1.2204647856676));
#37459=CARTESIAN_POINT('Ctrl Pts',(58.4285161456044,-4.16419790569076,-6.41064031617526));
#37460=CARTESIAN_POINT('Ctrl Pts',(58.5608572152325,0.54105679665563,-7.19405658280721));
#37461=CARTESIAN_POINT('Ctrl Pts',(58.6601130174535,3.92470418512737,-6.07814694081951));
#37462=CARTESIAN_POINT('Ctrl Pts',(58.7593688196745,6.33410982426262,-3.4534396343383));
#37463=CARTESIAN_POINT('Ctrl Pts',(58.8917098893027,7.55628044485889,1.15735876018381));
#37464=CARTESIAN_POINT('Ctrl Pts',(59.0571362263377,4.44759807302352,6.88498063449988));
#37465=CARTESIAN_POINT('Ctrl Pts',(59.2556478307798,-3.383462018219,7.4654478275059));
#37466=CARTESIAN_POINT('Ctrl Pts',(59.454159435222,-8.10677391155581,1.20869485018397));
#37467=CARTESIAN_POINT('Ctrl Pts',(59.6526710396641,-5.40303978286539,-6.16370408612994));
#37468=CARTESIAN_POINT('Ctrl Pts',(59.8180973766991,0.957119109800075,-7.58424528023631));
#37469=CARTESIAN_POINT('Ctrl Pts',(59.9504384463273,5.05666178638522,-5.14561601287451));
#37470=CARTESIAN_POINT('Ctrl Pts',(60.0496942485483,6.92083785156421,-2.10930713915861));
#37471=CARTESIAN_POINT('Ctrl Pts',(60.1489500507693,7.06703241868983,1.45060172584553));
#37472=CARTESIAN_POINT('Ctrl Pts',(60.2812911203974,5.02449176463669,5.76119223496576));
#37473=CARTESIAN_POINT('Ctrl Pts',(60.4467174574326,-1.04682003116853,8.12946829620154));
#37474=CARTESIAN_POINT('Ctrl Pts',(60.6452290618746,-7.4028683678955,3.51827605817898));
#37475=CARTESIAN_POINT('Ctrl Pts',(60.8437406663167,-6.97212863872708,-4.30930954318493));
#37476=CARTESIAN_POINT('Ctrl Pts',(61.0422522707589,-0.148496740647099,
-8.19524469888595));
#37477=CARTESIAN_POINT('Ctrl Pts',(61.2076786077939,5.62629851176496,-5.1750959911525));
#37478=CARTESIAN_POINT('Ctrl Pts',(61.340019677422,7.1835285625583,-0.666415759678704));
#37479=CARTESIAN_POINT('Ctrl Pts',(61.4392754796431,6.64760715387227,2.85595733559444));
#37480=CARTESIAN_POINT('Ctrl Pts',(61.5385312818641,4.46152916853726,5.66938709669134));
#37481=CARTESIAN_POINT('Ctrl Pts',(61.6708723514923,0.119161805817699,7.64347132690151));
#37482=CARTESIAN_POINT('Ctrl Pts',(61.8362986885272,-6.04672631772197,5.53364145885595));
#37483=CARTESIAN_POINT('Ctrl Pts',(62.0348102929695,-7.92520188427845,-2.09090927286969));
#37484=CARTESIAN_POINT('Ctrl Pts',(62.2333218974115,-2.5438895261837,-7.79162066405417));
#37485=CARTESIAN_POINT('Ctrl Pts',(62.4318335018536,5.17619531567503,-6.35539841477975));
#37486=CARTESIAN_POINT('Ctrl Pts',(62.5972598388888,7.63764655705976,-0.321260845052877));
#37487=CARTESIAN_POINT('Ctrl Pts',(62.7296009085168,5.91693737961713,4.12759550095798));
#37488=CARTESIAN_POINT('Ctrl Pts',(62.8288567107379,3.23408471669311,6.47208383908938));
#37489=CARTESIAN_POINT('Ctrl Pts',(62.9281125129589,-0.251575037739509,
7.20998630887921));
#37490=CARTESIAN_POINT('Ctrl Pts',(63.060453582587,-4.84245951105093,5.91501811873503));
#37491=CARTESIAN_POINT('Ctrl Pts',(63.2258799196221,-8.19019354779154,0.323753928647688));
#37492=CARTESIAN_POINT('Ctrl Pts',(63.4243915240641,-4.70371519063712,-6.71236097802501));
#37493=CARTESIAN_POINT('Ctrl Pts',(63.6229031285063,3.0860685027055,-7.59321458214847));
#37494=CARTESIAN_POINT('Ctrl Pts',(63.8214147329484,8.05568220034109,-1.51329813444295));
#37495=CARTESIAN_POINT('Ctrl Pts',(63.9868410699835,6.04101389033449,4.68433609361207));
#37496=CARTESIAN_POINT('Ctrl Pts',(64.1191821396116,1.85521869497751,6.9717541671838));
#37497=CARTESIAN_POINT('Ctrl Pts',(64.2184379418327,-1.70720091189527,7.0308348168176));
#37498=CARTESIAN_POINT('Ctrl Pts',(64.3176937440536,-4.84583662973596,5.34462907335459));
#37499=CARTESIAN_POINT('Ctrl Pts',(64.4500348136819,-7.51653054864387,1.39234405677461));
#37500=CARTESIAN_POINT('Ctrl Pts',(64.6154611507168,-6.46466001599287,-5.0390731126098));
#37501=CARTESIAN_POINT('Ctrl Pts',(64.813972755159,0.739779755921552,-8.16293160614863));
#37502=CARTESIAN_POINT('Ctrl Pts',(65.012484359601,7.25818535623405,-3.80781719998572));
#37503=CARTESIAN_POINT('Ctrl Pts',(65.2109959640432,7.12971071718912,4.04367556139354));
#37504=CARTESIAN_POINT('Ctrl Pts',(65.3764223010783,1.59064068527316,7.47707935436174));
#37505=CARTESIAN_POINT('Ctrl Pts',(65.5087633707064,-3.08289472959458,6.52249589192415));
#37506=CARTESIAN_POINT('Ctrl Pts',(65.6080191729274,-5.84201455782888,4.26825949081232));
#37507=CARTESIAN_POINT('Ctrl Pts',(65.7072749751485,-7.15095261084027,0.95449951885552));
#37508=CARTESIAN_POINT('Ctrl Pts',(65.8396160447767,-6.63983538642403,-3.7880654036783));
#37509=CARTESIAN_POINT('Ctrl Pts',(66.0050423818115,-1.6852579301835,-8.02147072946674));
#37510=CARTESIAN_POINT('Ctrl Pts',(66.2035539862539,5.83380696131112,-5.75737985847315));
#37511=CARTESIAN_POINT('Ctrl Pts',(66.4020655906958,8.00157680664466,1.77637132973648));
#37512=CARTESIAN_POINT('Ctrl Pts',(66.600577195138,2.83570451857797,7.69043996340305));
#37513=CARTESIAN_POINT('Ctrl Pts',(66.7660035321731,-3.61114211588056,6.73769293585757));
#37514=CARTESIAN_POINT('Ctrl Pts',(66.8983446018012,-6.56466625071433,2.99204772276496));
#37515=CARTESIAN_POINT('Ctrl Pts',(66.9976004040222,-7.2170938170707,-0.510617293293015));
#37516=CARTESIAN_POINT('Ctrl Pts',(67.0968562062432,-6.07799932508554,-3.88653017593029));
#37517=CARTESIAN_POINT('Ctrl Pts',(67.2291972758714,-2.62651982706667,-7.17901433868201));
#37518=CARTESIAN_POINT('Ctrl Pts',(67.3946236129064,3.89025040628289,-7.21457131145677));
#37519=CARTESIAN_POINT('Ctrl Pts',(67.5931352173485,8.17197698838295,-0.632074624543493));
#37520=CARTESIAN_POINT('Ctrl Pts',(67.7916468217907,4.96506899196963,6.52141207658738));
#37521=CARTESIAN_POINT('Ctrl Pts',(67.9901584262327,-2.79787238141651,7.70428452457515));
#37522=CARTESIAN_POINT('Ctrl Pts',(68.1555847632679,-7.10704187889876,2.81545845931199));
#37523=CARTESIAN_POINT('Ctrl Pts',(68.2879258328959,-6.94532695410545,-1.95182630988612));
#37524=CARTESIAN_POINT('Ctrl Pts',(68.3871816351171,-5.18285883819335,-5.04828231948625));
#37525=CARTESIAN_POINT('Ctrl Pts',(68.486437437338,-2.13383424279239,-6.89158342391702));
#37526=CARTESIAN_POINT('Ctrl Pts',(68.6187785069662,2.62754970512971,-7.17864156401975));
#37527=CARTESIAN_POINT('Ctrl Pts',(68.7842048440012,7.62802463440124,-2.99954185919825));
#37528=CARTESIAN_POINT('Ctrl Pts',(68.9827164484433,6.64975495342578,4.7918063211089));
#37529=CARTESIAN_POINT('Ctrl Pts',(69.1812280528854,-0.416915198702002,
8.18579837023763));
#37530=CARTESIAN_POINT('Ctrl Pts',(69.3797396573275,-7.10973832650691,4.07862272490673));
#37531=CARTESIAN_POINT('Ctrl Pts',(69.5451659943627,-7.24563662171936,-2.43670125431101));
#37532=CARTESIAN_POINT('Ctrl Pts',(69.6775070639907,-4.04502533630726,-5.97378234857353));
#37533=CARTESIAN_POINT('Ctrl Pts',(69.7767628662118,-0.7003351904756,-7.20091934778666));
#37534=CARTESIAN_POINT('Ctrl Pts',(69.8760186684328,2.81846067751086,-6.64155002296871));
#37535=CARTESIAN_POINT('Ctrl Pts',(70.008359738061,6.64012327459028,-3.78612972542153));
#37536=CARTESIAN_POINT('Ctrl Pts',(70.1737860750959,7.76288615048499,2.63043722061295));
#37537=CARTESIAN_POINT('Ctrl Pts',(70.3722976795382,1.98535818899343,7.95541533816283));
#37538=CARTESIAN_POINT('Ctrl Pts',(70.5708092839802,-5.60036139298603,5.97713454909029));
#37539=CARTESIAN_POINT('Ctrl Pts',(70.7693208884224,-8.06606896756193,-1.46200603608502));
#37540=CARTESIAN_POINT('Ctrl Pts',(70.9678324928645,-3.13451622979428,-7.5752150383098));
#37541=CARTESIAN_POINT('Ctrl Pts',(71.1332588298995,3.35153198035595,-6.87266150813771));
#37542=CARTESIAN_POINT('Ctrl Pts',(71.2655998995277,6.4351344135931,-3.24546016726863));
#37543=CARTESIAN_POINT('Ctrl Pts',(71.3979409691556,7.51702449814323,1.38731120573129));
#37544=CARTESIAN_POINT('Ctrl Pts',(71.5633673061908,4.23448854948942,7.02493677792881));
#37545=CARTESIAN_POINT('Ctrl Pts',(71.7618789106328,-3.62636197138777,7.35273307434348));
#37546=CARTESIAN_POINT('Ctrl Pts',(71.9273052476681,-7.36873471237381,2.0246969407879));
#37547=CARTESIAN_POINT('Ctrl Pts',(72.0596463172959,-6.69257905832717,-2.69716983719333));
#37548=CARTESIAN_POINT('Ctrl Pts',(72.1589021195172,-4.60123349955128,-5.58285884611192));
#37549=CARTESIAN_POINT('Ctrl Pts',(72.2581579217382,-1.37052351308357,-7.08310535950425));
#37550=CARTESIAN_POINT('Ctrl Pts',(72.3904989913663,3.39433210286424,-6.84955869054765));
#37551=CARTESIAN_POINT('Ctrl Pts',(72.5559253284013,7.90931691245014,-2.15054133310692));
#37552=CARTESIAN_POINT('Ctrl Pts',(72.7544369328434,6.08809628195235,5.48786961221882));
#37553=CARTESIAN_POINT('Ctrl Pts',(72.9529485372855,-1.30640323031847,8.09160345854923));
#37554=CARTESIAN_POINT('Ctrl Pts',(73.1514601417277,-7.51181763259486,3.27969229408906));
#37555=CARTESIAN_POINT('Ctrl Pts',(73.3168864787628,-6.93696759148421,-3.21177358578175));
#37556=CARTESIAN_POINT('Ctrl Pts',(73.4492275483909,-3.37006034220166,-6.37885915445045));
#37557=CARTESIAN_POINT('Ctrl Pts',(73.5484833506119,0.0885511521900275,
-7.23459307282265));
#37558=CARTESIAN_POINT('Ctrl Pts',(73.647739152833,3.52519199163394,-6.29445949177426));
#37559=CARTESIAN_POINT('Ctrl Pts',(73.780080222461,7.01349237856603,-3.04101410392474));
#37560=CARTESIAN_POINT('Ctrl Pts',(73.9455065594961,7.42931202422622,3.46257383852393));
#37561=CARTESIAN_POINT('Ctrl Pts',(74.1440181639383,1.10791776076921,8.12116023680133));
#37562=CARTESIAN_POINT('Ctrl Pts',(74.3425297683803,-6.22053285582939,5.33719926660008));
#37563=CARTESIAN_POINT('Ctrl Pts',(74.5410413728225,-7.85443827270103,-2.34347769528696));
#37564=CARTESIAN_POINT('Ctrl Pts',(74.7064677098574,-3.22543050411949,-6.9306169413023));
#37565=CARTESIAN_POINT('Ctrl Pts',(74.8388087794857,1.54316722938047,-7.04739863047344));
#37566=CARTESIAN_POINT('Ctrl Pts',(74.9380645817065,4.73720272242289,-5.46864550144068));
#37567=CARTESIAN_POINT('Ctrl Pts',(75.0373203839278,6.75530734053086,-2.53239318636892));
#37568=CARTESIAN_POINT('Ctrl Pts',(75.1696614535558,7.31974743008187,2.20412138298759));
#37569=CARTESIAN_POINT('Ctrl Pts',(75.3350877905909,3.43961240388645,7.43996998991286));
#37570=CARTESIAN_POINT('Ctrl Pts',(75.533599395033,-4.39556885165141,6.91807060949306));
#37571=CARTESIAN_POINT('Ctrl Pts',(75.7321109994751,-8.19615403019618,0.0615273568355724));
#37572=CARTESIAN_POINT('Ctrl Pts',(75.9306226039173,-4.48664549632056,-6.85959905122507));
#37573=CARTESIAN_POINT('Ctrl Pts',(76.0960489409522,2.0097710123082,-7.37547787868233));
#37574=CARTESIAN_POINT('Ctrl Pts',(76.2283900105805,5.72741628337472,-4.38678644242978));
#37575=CARTESIAN_POINT('Ctrl Pts',(76.3276458128014,7.14802407214726,-1.11934134133585));
#37576=CARTESIAN_POINT('Ctrl Pts',(76.4269016150226,6.79425520799035,2.42596140587257));
#37577=CARTESIAN_POINT('Ctrl Pts',(76.5592426846505,4.16819463821222,6.40804236245229));
#37578=CARTESIAN_POINT('Ctrl Pts',(76.7246690216857,-2.17494002259612,7.90276678478469));
#37579=CARTESIAN_POINT('Ctrl Pts',(76.9231806261278,-7.82261403601631,2.44692381113861));
#37580=CARTESIAN_POINT('Ctrl Pts',(77.1216922305699,-6.29995860883805,-5.24320970597619));
#37581=CARTESIAN_POINT('Ctrl Pts',(77.320203835012,1.00061296459978,-8.13528491521204));
#37582=CARTESIAN_POINT('Ctrl Pts',(77.4856301720472,6.2955681948585,-4.33620508798002));
#37583=CARTESIAN_POINT('Ctrl Pts',(77.6179712416751,7.20606650304075,0.346118661139733));
#37584=CARTESIAN_POINT('Ctrl Pts',(77.7172270438963,6.18215959176197,3.75873329154079));
#37585=CARTESIAN_POINT('Ctrl Pts',(77.8164828461173,3.62363562623967,6.23830565314694));
#37586=CARTESIAN_POINT('Ctrl Pts',(77.9488239157453,-0.95238954586989,7.58484064526405));
#37587=CARTESIAN_POINT('Ctrl Pts',(78.1142502527805,-6.76206317771884,4.63234158251969));
#37588=CARTESIAN_POINT('Ctrl Pts',(78.3127618572225,-7.55430092435108,-3.1801358521754));
#37589=CARTESIAN_POINT('Ctrl Pts',(78.5112734616647,-1.4276986401798,-8.071084381096));
#37590=CARTESIAN_POINT('Ctrl Pts',(78.7097850661068,6.01518756313756,-5.56790854243103));
#37591=CARTESIAN_POINT('Ctrl Pts',(78.8752114031419,7.60737483598701,0.751466277302418));
#37592=CARTESIAN_POINT('Ctrl Pts',(79.00755247277,5.28061196900669,4.9155192814821));
#37593=CARTESIAN_POINT('Ctrl Pts',(79.106808274991,2.29587814793631,6.86120373584534));
#37594=CARTESIAN_POINT('Ctrl Pts',(79.2060640772122,-1.25876877679799,7.10370985756017));
#37595=CARTESIAN_POINT('Ctrl Pts',(79.33840514684,-5.62307033548875,5.17860342788263));
#37596=CARTESIAN_POINT('Ctrl Pts',(79.5038314838753,-8.1548262198857,-0.826375386894838));
#37597=CARTESIAN_POINT('Ctrl Pts',(79.7023430883173,-3.71737910263321,-7.30491746026261));
#37598=CARTESIAN_POINT('Ctrl Pts',(79.9008546927595,4.11899803065852,-7.08622478597556));
#37599=CARTESIAN_POINT('Ctrl Pts',(80.0993662972016,8.18822183313877,-0.370283901770539));
#37600=CARTESIAN_POINT('Ctrl Pts',(80.2647926342367,5.32550095363364,5.48414925526085));
#37601=CARTESIAN_POINT('Ctrl Pts',(80.3971337038647,0.860626431278914,7.16285660331288));
#37602=CARTESIAN_POINT('Ctrl Pts',(80.496389506086,-2.67496305039171,6.72248063247407));
#37603=CARTESIAN_POINT('Ctrl Pts',(80.5956453083067,-5.54653798250745,4.61336200426993));
#37604=CARTESIAN_POINT('Ctrl Pts',(80.7279863779351,-7.63744474051541,0.326023460360154));
#37605=CARTESIAN_POINT('Ctrl Pts',(80.8934127149699,-5.69529582435376,-5.89471733246808));
#37606=CARTESIAN_POINT('Ctrl Pts',(81.0919243194123,1.87561142445985,-7.97889768566929));
#37607=CARTESIAN_POINT('Ctrl Pts',(81.2904359238541,7.71990350306442,-2.75387298133316));
#37608=CARTESIAN_POINT('Ctrl Pts',(81.4889475282964,6.49318676803834,5.00226074410088));
#37609=CARTESIAN_POINT('Ctrl Pts',(81.6543738653314,0.527890767039223,7.62615137531419));
#37610=CARTESIAN_POINT('Ctrl Pts',(81.7867149349596,-3.96591412848519,6.02650128178202));
#37611=CARTESIAN_POINT('Ctrl Pts',(81.8859707371805,-6.38216694643353,3.4080959849747));
#37612=CARTESIAN_POINT('Ctrl Pts',(81.9852265394017,-7.21415425106946,-0.0563117715569949));
#37613=CARTESIAN_POINT('Ctrl Pts',(82.1175676090296,-6.04393377050729,-4.68056813205964));
#37614=CARTESIAN_POINT('Ctrl Pts',(82.2829939460648,-0.5453401348518,-8.17842839999966));
#37615=CARTESIAN_POINT('Ctrl Pts',(82.4815055505069,6.58257380241805,-4.88369211044909));
#37616=CARTESIAN_POINT('Ctrl Pts',(82.6800171549491,7.67397055088154,2.87939272732047));
#37617=CARTESIAN_POINT('Ctrl Pts',(82.8785287593911,1.73080727378638,8.01176591879775));
#37618=CARTESIAN_POINT('Ctrl Pts',(83.0439550964263,-4.51909200982883,6.16560304170094));
#37619=CARTESIAN_POINT('Ctrl Pts',(83.1762961660543,-6.91897945288657,2.04326109549728));
#37620=CARTESIAN_POINT('Ctrl Pts',(83.2755519682754,-7.07447154442634,-1.5162537855029));
#37621=CARTESIAN_POINT('Ctrl Pts',(83.3748077704965,-5.47384515977853,-4.69938418738115));
#37622=CARTESIAN_POINT('Ctrl Pts',(83.5071488401244,-1.59530292740683,-7.47608601013512));
#37623=CARTESIAN_POINT('Ctrl Pts',(83.6725751771596,4.86223112684713,-6.59869649443888));
#37624=CARTESIAN_POINT('Ctrl Pts',(83.8710867816016,8.17996582553711,0.518541789046997));
#37625=CARTESIAN_POINT('Ctrl Pts',(84.0695983860439,4.00289763898197,7.1524497192064));
#37626=CARTESIAN_POINT('Ctrl Pts',(84.2681099904858,-3.84919571395828,7.2365585268307));
#37627=CARTESIAN_POINT('Ctrl Pts',(84.433536327521,-7.43128147235665,1.79245896459043));
#37628=CARTESIAN_POINT('Ctrl Pts',(84.5658773971491,-6.60355831010481,-2.90520398920369));
#37629=CARTESIAN_POINT('Ctrl Pts',(84.6651331993701,-4.42483609723173,-5.72433390776467));
#37630=CARTESIAN_POINT('Ctrl Pts',(84.7643890015913,-1.14772280657254,-7.12249429154648));
#37631=CARTESIAN_POINT('Ctrl Pts',(84.8967300712191,3.60693992809988,-6.73994345793868));
#37632=CARTESIAN_POINT('Ctrl Pts',(85.0621564082546,7.97291211063296,-1.90177796619987));
#37633=CARTESIAN_POINT('Ctrl Pts',(85.2606680126964,5.91318860450045,5.67581950219958));
#37634=CARTESIAN_POINT('Ctrl Pts',(85.4591796171386,-1.5591213078961,8.04673022048133));
#37635=CARTESIAN_POINT('Ctrl Pts',(85.6576912215807,-7.6108605802676,3.04284212280718));
#37636=CARTESIAN_POINT('Ctrl Pts',(85.8231175586158,-6.83297591294963,-3.42743251343945));
#37637=CARTESIAN_POINT('Ctrl Pts',(85.9554586282438,-3.16865385062834,-6.4812672641033));
#37638=CARTESIAN_POINT('Ctrl Pts',(86.054714430465,0.315066708290052,-7.22827131092052));
#37639=CARTESIAN_POINT('Ctrl Pts',(86.153970232686,3.72057726039948,-6.18097867843254));
#37640=CARTESIAN_POINT('Ctrl Pts',(86.286311302314,7.10528491496656,-2.81989002237311));
#37641=CARTESIAN_POINT('Ctrl Pts',(86.4517376393491,7.31723484533139,3.69352963638701));
#37642=CARTESIAN_POINT('Ctrl Pts',(86.6502492437914,0.853054781769095,8.1518724249858));
#37643=CARTESIAN_POINT('Ctrl Pts',(86.8487608482333,-6.38462023325127,5.13978121821364));
#37644=CARTESIAN_POINT('Ctrl Pts',(87.0472724526756,-7.77719827735906,-2.58829556102961));
#37645=CARTESIAN_POINT('Ctrl Pts',(87.2126987897105,-3.00681146855234,-7.02822440262923));
#37646=CARTESIAN_POINT('Ctrl Pts',(87.3450398593387,1.76310463197224,-6.99561681558938));
#37647=CARTESIAN_POINT('Ctrl Pts',(87.4442956615597,4.90613379615755,-5.31761453559306));
#37648=CARTESIAN_POINT('Ctrl Pts',(87.5435514637808,6.83129783049185,-2.31960395864394));
#37649=CARTESIAN_POINT('Ctrl Pts',(87.6758925334088,7.24713379598624,2.43226339120684));
#37650=CARTESIAN_POINT('Ctrl Pts',(87.8413188704439,3.20493753483079,7.54403488555254));
#37651=CARTESIAN_POINT('Ctrl Pts',(88.0398304748861,-4.61005725891556,6.77702726595246));
#37652=CARTESIAN_POINT('Ctrl Pts',(88.238342079328,-8.1940609418445,-0.195171143567751));
#37653=CARTESIAN_POINT('Ctrl Pts',(88.4368536837704,-4.26963182496724,-6.99673717069805));
#37654=CARTESIAN_POINT('Ctrl Pts',(88.6022800208052,2.23975357990136,-7.30892313288694));
#37655=CARTESIAN_POINT('Ctrl Pts',(88.7346210904336,5.86198253311296,-4.2052768464535));
#37656=CARTESIAN_POINT('Ctrl Pts',(88.8338768926543,7.1795712352997,-0.894946954968044));
#37657=CARTESIAN_POINT('Ctrl Pts',(88.9331326948758,6.71495223218478,2.63753845342878));
#37658=CARTESIAN_POINT('Ctrl Pts',(89.0654737645034,3.96547796806157,6.53542943852582));
#37659=CARTESIAN_POINT('Ctrl Pts',(89.2309001015389,-2.421354004456,7.8307810428913));
#37660=CARTESIAN_POINT('Ctrl Pts',(89.4294117059807,-7.89540451993751,2.2007530439587));
#37661=CARTESIAN_POINT('Ctrl Pts',(89.627923310423,-6.13267395365651,-5.43792576926969));
#37662=CARTESIAN_POINT('Ctrl Pts',(89.8264349148651,1.25488437193329,-8.09996001037527));
#37663=CARTESIAN_POINT('Ctrl Pts',(89.9918612519001,6.42827179997809,-4.13692822354185));
#37664=CARTESIAN_POINT('Ctrl Pts',(90.1242023215283,7.19169328889517,0.571611942054712));
#37665=CARTESIAN_POINT('Ctrl Pts',(90.2234581237492,6.06142013417448,3.95048846751564));
#37666=CARTESIAN_POINT('Ctrl Pts',(90.3227139259704,3.42650146314732,6.34872272956444));
#37667=CARTESIAN_POINT('Ctrl Pts',(90.4550549955983,-1.18944705552714,7.55129585986596));
#37668=CARTESIAN_POINT('Ctrl Pts',(90.6204813326335,-6.90381170961845,4.41831085763963));
#37669=CARTESIAN_POINT('Ctrl Pts',(90.8189929370757,-7.45100767605583,-3.4151443754694));
#37670=CARTESIAN_POINT('Ctrl Pts',(91.0175045415177,-1.17424673552373,-8.11183524845364));
#37671=CARTESIAN_POINT('Ctrl Pts',(91.2160161459598,6.18660034222907,-5.37680789708281));
#37672=CARTESIAN_POINT('Ctrl Pts',(91.381442482995,7.58011105191034,0.989328005182139));
#37673=CARTESIAN_POINT('Ctrl Pts',(91.513783552623,5.12408911536659,5.0784745063474));
#37674=CARTESIAN_POINT('Ctrl Pts',(91.6130393548441,2.07988870140306,6.92973564897867));
#37675=CARTESIAN_POINT('Ctrl Pts',(91.7122951570651,-1.48060907187722,7.06080656512513));
#37676=CARTESIAN_POINT('Ctrl Pts',(91.8446362266932,-5.78248406790028,4.99997314648891));
#37677=CARTESIAN_POINT('Ctrl Pts',(92.0100625637283,-8.12494810308719,-1.08134419993861));
#37678=CARTESIAN_POINT('Ctrl Pts',(92.2085741681704,-3.48679726401757,-7.41774705241314));
#37679=CARTESIAN_POINT('Ctrl Pts',(92.4070857726126,4.33888794927058,-6.95375997986828));
#37680=CARTESIAN_POINT('Ctrl Pts',(92.6055973770546,8.19580156390679,-0.113682371825931));
#37681=CARTESIAN_POINT('Ctrl Pts',(92.7710237140897,5.15114903660088,5.64823132173759));
#37682=CARTESIAN_POINT('Ctrl Pts',(92.9033647837178,0.635894442291002,7.18629465246884));
#37683=CARTESIAN_POINT('Ctrl Pts',(93.0026205859388,-2.88417030209986,6.63541519751662));
#37684=CARTESIAN_POINT('Ctrl Pts',(93.10187638816,-5.68828831828898,4.43740561385328));
#37685=CARTESIAN_POINT('Ctrl Pts',(93.2342174577878,-7.64390855687611,0.0866916100138159));
#37686=CARTESIAN_POINT('Ctrl Pts',(93.3996437948232,-5.50790531097854,-6.07017841928023));
#37687=CARTESIAN_POINT('Ctrl Pts',(93.5981553992651,2.12455630675614,-7.9162482902803));
#37688=CARTESIAN_POINT('Ctrl Pts',(93.7966670037073,7.80235669107675,-2.51076812134315));
#37689=CARTESIAN_POINT('Ctrl Pts',(93.9951786081494,6.33335282885967,5.20314605808604));
#37690=CARTESIAN_POINT('Ctrl Pts',(94.1606049451845,0.288813569149044,7.63894234717125));
#37691=CARTESIAN_POINT('Ctrl Pts',(94.2929460148125,-4.15269314181078,5.89935015436421));
#37692=CARTESIAN_POINT('Ctrl Pts',(94.3922018170336,-6.48576368973312,3.20656241727638));
#37693=CARTESIAN_POINT('Ctrl Pts',(94.4914576192548,-7.20885257666468,-0.282200463773047));
#37694=CARTESIAN_POINT('Ctrl Pts',(94.6237986888826,-5.89439420080124,-4.86754254903762));
#37695=CARTESIAN_POINT('Ctrl Pts',(94.789225025918,-0.28895943561254,-8.19149494299867));
#37696=CARTESIAN_POINT('Ctrl Pts',(94.9877366303599,6.73228158455901,-4.67515894490773));
#37697=CARTESIAN_POINT('Ctrl Pts',(95.1862482348021,7.58003659211948,3.11829629061651));
#37698=CARTESIAN_POINT('Ctrl Pts',(95.3847598392441,1.47906430674842,8.06203793920023));
#37699=CARTESIAN_POINT('Ctrl Pts',(95.5501861762794,-4.70995578262514,6.02106053671999));
#37700=CARTESIAN_POINT('Ctrl Pts',(95.6825272459072,-6.97957214897654,1.82558625955343));
#37701=CARTESIAN_POINT('Ctrl Pts',(95.7817830481286,-7.0235192681072,-1.73705217695852));
#37702=CARTESIAN_POINT('Ctrl Pts',(95.8810388503493,-5.32399595596597,-4.8684966503734));
#37703=CARTESIAN_POINT('Ctrl Pts',(96.0133799199777,-1.36040161224302,-7.52237734459912));
#37704=CARTESIAN_POINT('Ctrl Pts',(96.1788062570125,5.06648923056177,-6.44319593316877));
#37705=CARTESIAN_POINT('Ctrl Pts',(96.3773178614548,8.15971540431764,0.774448845621636));
#37706=CARTESIAN_POINT('Ctrl Pts',(96.5758294658966,3.7769504003016,7.27429530384934));
#37707=CARTESIAN_POINT('Ctrl Pts',(96.7743410703392,-4.0739257657314,7.11246903767678));
#37708=CARTESIAN_POINT('Ctrl Pts',(96.9397674073737,-7.48376886138719,1.55886403847908));
#37709=CARTESIAN_POINT('Ctrl Pts',(97.0721084770024,-6.50934104460086,-3.11057418154813));
#37710=CARTESIAN_POINT('Ctrl Pts',(97.1713642792229,-4.24340436628601,-5.8600932210277));
#37711=CARTESIAN_POINT('Ctrl Pts',(97.2706200814444,-0.924113983348465,
-7.1549427614495));
#37712=CARTESIAN_POINT('Ctrl Pts',(97.4029611510721,3.81623694597436,-6.62368394726916));
#37713=CARTESIAN_POINT('Ctrl Pts',(97.5683874881075,8.02855725455025,-1.65116787971719));
#37714=CARTESIAN_POINT('Ctrl Pts',(97.7668990925495,5.73254616351181,5.85821141451459));
#37715=CARTESIAN_POINT('Ctrl Pts',(97.9654106969915,-1.81034563845534,7.99395866659747));
#37716=CARTESIAN_POINT('Ctrl Pts',(98.1639223014339,-7.70241652089553,2.80301029167512));
#37717=CARTESIAN_POINT('Ctrl Pts',(98.3293486384687,-6.72229217472482,-3.63973094867799));
#37718=CARTESIAN_POINT('Ctrl Pts',(98.461689708097,-2.96413432287727,-6.57731710424392));
#37719=CARTESIAN_POINT('Ctrl Pts',(98.5609455103179,0.541270578014203,-7.21485962000136));
#37720=CARTESIAN_POINT('Ctrl Pts',(98.6602013125391,3.91231416913188,-6.06143468296485));
#37721=CARTESIAN_POINT('Ctrl Pts',(98.792542382167,7.19010691694292,-2.59599999692997));
#37722=CARTESIAN_POINT('Ctrl Pts',(98.9579687192023,7.19798058054701,3.9208624712771));
#37723=CARTESIAN_POINT('Ctrl Pts',(99.1564803236443,0.597354780781096,8.17458829298583));
#37724=CARTESIAN_POINT('Ctrl Pts',(99.3549919280863,-6.54244471348264,4.93732150715004));
#37725=CARTESIAN_POINT('Ctrl Pts',(99.5535035325286,-7.69232960220158,-2.83057454374467));
#37726=CARTESIAN_POINT('Ctrl Pts',(99.7189298695635,-2.78524297030128,-7.1189377759269));
#37727=CARTESIAN_POINT('Ctrl Pts',(99.8512709391918,1.98131256247304,-6.9369729063638));
#37728=CARTESIAN_POINT('Ctrl Pts',(99.9505267414127,5.07025238557831,-5.16136744685812));
#37729=CARTESIAN_POINT('Ctrl Pts',(100.049782543634,6.90058740162031,-2.10453940006798));
#37730=CARTESIAN_POINT('Ctrl Pts',(100.182123613262,7.16741135167138,2.65801955919494));
#37731=CARTESIAN_POINT('Ctrl Pts',(100.347549950297,2.96711889648337,7.64069973305668));
#37732=CARTESIAN_POINT('Ctrl Pts',(100.546061554739,-4.8200235964893,6.62933624303592));
#37733=CARTESIAN_POINT('Ctrl Pts',(100.744573159181,-8.18393018661653,-0.451678197979063));
#37734=CARTESIAN_POINT('Ctrl Pts',(100.943084763623,-4.04843001256235,-7.12701209413773));
#37735=CARTESIAN_POINT('Ctrl Pts',(101.108511100658,2.46753914216655,-7.23519896360887));
#37736=CARTESIAN_POINT('Ctrl Pts',(101.240852170286,5.9907986834069,-4.01964223640978));
#37737=CARTESIAN_POINT('Ctrl Pts',(101.340107972508,7.20407585797007,-0.669674702794391));
#37738=CARTESIAN_POINT('Ctrl Pts',(101.439363774729,6.6290624671403,2.84652830314237));
#37739=CARTESIAN_POINT('Ctrl Pts',(101.571704844357,3.75887150586802,6.65640582172574));
#37740=CARTESIAN_POINT('Ctrl Pts',(101.737131181392,-2.66539284677105,7.75111397987301));
#37741=CARTESIAN_POINT('Ctrl Pts',(101.935642785834,-7.96045029267649,1.95242352776489));
#37742=CARTESIAN_POINT('Ctrl Pts',(102.134154390276,-5.95937367401093,-5.62730769617671));
#37743=CARTESIAN_POINT('Ctrl Pts',(102.332665994718,1.50792484587792,-8.05668974305115));
#37744=CARTESIAN_POINT('Ctrl Pts',(102.498092331753,6.55466982463192,-3.93359338915324));
#37745=CARTESIAN_POINT('Ctrl Pts',(102.630433401381,7.17026564361548,0.796544520931952));
#37746=CARTESIAN_POINT('Ctrl Pts',(102.729689203602,5.93473494597949,4.13836855486806));
#37747=CARTESIAN_POINT('Ctrl Pts',(102.828945005823,3.22600619751222,6.45291225629539));
#37748=CARTESIAN_POINT('Ctrl Pts',(102.961286075451,-1.42533782016256,7.51034390421344));
#37749=CARTESIAN_POINT('Ctrl Pts',(103.126712412487,-7.03878819739605,4.19994615070119));
#37750=CARTESIAN_POINT('Ctrl Pts',(103.325224016929,-7.34040563156762,-3.64680293654208));
#37751=CARTESIAN_POINT('Ctrl Pts',(103.523735621371,-0.919642996050166,
-8.14462910474322));
#37752=CARTESIAN_POINT('Ctrl Pts',(103.722247225813,6.35194459972139,-5.18043306670365));
#37753=CARTESIAN_POINT('Ctrl Pts',(103.887673562848,7.54541183235724,1.22621928756231));
#37754=CARTESIAN_POINT('Ctrl Pts',(104.020014632476,4.96253997204499,5.23644818554906));
#37755=CARTESIAN_POINT('Ctrl Pts',(104.119270434697,1.86185906335093,6.9914700887944));
#37756=CARTESIAN_POINT('Ctrl Pts',(104.218526236918,-1.70099701708682,7.0109772302331));
#37757=CARTESIAN_POINT('Ctrl Pts',(104.350867306546,-5.93622568196176,4.81643832229469));
#37758=CARTESIAN_POINT('Ctrl Pts',(104.516293643581,-8.08710011258896,-1.33525230717154));
#37759=CARTESIAN_POINT('Ctrl Pts',(104.714805248023,-3.25279517795495,-7.52330047479355));
#37760=CARTESIAN_POINT('Ctrl Pts',(104.913316852466,4.5545217929969,-6.81447413355386));
#37761=CARTESIAN_POINT('Ctrl Pts',(105.111828456908,8.19534191959957,0.143030668481208));
#37762=CARTESIAN_POINT('Ctrl Pts',(105.277254793943,4.97174428693698,5.80677296415496));
#37763=CARTESIAN_POINT('Ctrl Pts',(105.409595863571,0.410538694972291,7.20268356057518));
#37764=CARTESIAN_POINT('Ctrl Pts',(105.508851665792,-3.09054842984606,6.54184100431835));
#37765=CARTESIAN_POINT('Ctrl Pts',(105.608107468013,-5.82445893643908,4.25709648884606));
#37766=CARTESIAN_POINT('Ctrl Pts',(105.740448537641,-7.64287435179083,-0.152725229310253));
#37767=CARTESIAN_POINT('Ctrl Pts',(105.905874874676,-5.31511202979502,-6.23968528226296));
#37768=CARTESIAN_POINT('Ctrl Pts',(106.104386479118,2.37141720322459,-7.84583357489262));
#37769=CARTESIAN_POINT('Ctrl Pts',(106.30289808356,7.8771564015956,-2.26520071409541));
#37770=CARTESIAN_POINT('Ctrl Pts',(106.501409688003,6.16730649189762,5.39892812568543));
#37771=CARTESIAN_POINT('Ctrl Pts',(106.666836025037,0.0494529375975138,
7.64423913575313));
#37772=CARTESIAN_POINT('Ctrl Pts',(106.799177094666,-4.33539853602892,5.76641372581939));
#37773=CARTESIAN_POINT('Ctrl Pts',(106.898432896887,-6.58299886234465,3.00188031505507));
#37774=CARTESIAN_POINT('Ctrl Pts',(106.997688699108,-7.19647889300465,-0.507806484833575));
#37775=CARTESIAN_POINT('Ctrl Pts',(107.130029768736,-5.73907435111488,-5.04975498101209));
#37776=CARTESIAN_POINT('Ctrl Pts',(107.295456105771,-0.0322920042968116,
-8.19650053508292));
#37777=CARTESIAN_POINT('Ctrl Pts',(107.493967710213,6.87538010918837,-4.46208277408401));
#37778=CARTESIAN_POINT('Ctrl Pts',(107.692479314655,7.47867733972214,3.35422008809143));
#37779=CARTESIAN_POINT('Ctrl Pts',(107.890990919097,1.22585064624322,8.10424595418784));
#37780=CARTESIAN_POINT('Ctrl Pts',(108.056417256132,-4.89616459018992,5.8708858044287));
#37781=CARTESIAN_POINT('Ctrl Pts',(108.18875832576,-7.03336727340939,1.60573780850504));
#37782=CARTESIAN_POINT('Ctrl Pts',(108.288014127981,-6.96557098724266,-1.95531034861243));
#37783=CARTESIAN_POINT('Ctrl Pts',(108.387269930203,-5.16912081155891,-5.03437754836346));
#37784=CARTESIAN_POINT('Ctrl Pts',(108.51961099983,-1.12374364642211,-7.55794914914912));
#37785=CARTESIAN_POINT('Ctrl Pts',(108.685037336866,5.26494275239868,-6.28824056464582));
#37786=CARTESIAN_POINT('Ctrl Pts',(108.883548941308,8.13270769338756,1.04131295379453));
#37787=CARTESIAN_POINT('Ctrl Pts',(109.048975278343,4.31059234212791,6.31114658088431));
#37788=CARTESIAN_POINT('Ctrl Pts',(109.181316347971,-0.379872332578537,
7.2055380683537));
#37789=CARTESIAN_POINT('Ctrl Pts',(109.280572150192,-3.77681976785492,6.16629695720056));
#37790=CARTESIAN_POINT('Ctrl Pts',(109.379827952413,-6.26964300376297,3.59558754355007));
#37791=CARTESIAN_POINT('Ctrl Pts',(109.445998487227,-6.90538169251611,1.30827352835722));
#37792=CARTESIAN_POINT('Ctrl Pts',(109.479083754634,-6.93125428135741,0.155573414067464));
#37793=CARTESIAN_POINT('Ctrl Pts',(108.233548336394,-6.93028901950621,-0.00380765172104063));
#37794=CARTESIAN_POINT('Ctrl Pts',(108.251703600256,-6.93170393511236,-0.636222120076916));
#37795=CARTESIAN_POINT('Ctrl Pts',(108.269858864119,-6.84796028214185,-1.26769555840962));
#37796=CARTESIAN_POINT('Ctrl Pts',(108.288014127981,-6.67746200565648,-1.87498018905138));
#37797=CARTESIAN_POINT('Ctrl Pts',(108.321099395389,-6.36675426201473,-2.98166608186278));
#37798=CARTESIAN_POINT('Ctrl Pts',(108.354184662796,-5.76793753678676,-4.00802181511322));
#37799=CARTESIAN_POINT('Ctrl Pts',(108.387269930203,-4.96285702853069,-4.83664613183659));
#37800=CARTESIAN_POINT('Ctrl Pts',(108.420355197609,-4.15777652027462,-5.66527044855996));
#37801=CARTESIAN_POINT('Ctrl Pts',(108.453440465016,-3.14643222899067,-6.29616334875622));
#37802=CARTESIAN_POINT('Ctrl Pts',(108.486525732423,-2.04629027487981,-6.63211137658697));
#37803=CARTESIAN_POINT('Ctrl Pts',(108.552696267238,0.153993633341921,-7.30400743224846));
#37804=CARTESIAN_POINT('Ctrl Pts',(108.618866802052,2.70946819287044,-6.79612399844709));
#37805=CARTESIAN_POINT('Ctrl Pts',(108.685037336866,4.46516629613274,-5.32059002847302));
#37806=CARTESIAN_POINT('Ctrl Pts',(108.75120787168,6.22086439939495,-3.84505605849902));
#37807=CARTESIAN_POINT('Ctrl Pts',(108.817378406494,7.17678604639124,-1.40187155235226));
#37808=CARTESIAN_POINT('Ctrl Pts',(108.883548941308,6.89032379963751,0.873687426138972));
#37809=CARTESIAN_POINT('Ctrl Pts',(108.944699294205,6.6255946791913,2.97660581669859));
#37810=CARTESIAN_POINT('Ctrl Pts',(109.005849647103,5.29984338919197,4.93636845490143));
#37811=CARTESIAN_POINT('Ctrl Pts',(109.067,3.46405146923455,6.01146880811242));
#37812=CARTESIAN_POINT('',(31.067,5.11685509991379,3.5431531688378));
#37813=CARTESIAN_POINT('Ctrl Pts',(31.067,5.11685509991369,3.54315316883794));
#37814=CARTESIAN_POINT('Ctrl Pts',(31.067,5.2144007801441,3.41955272739614));
#37815=CARTESIAN_POINT('Ctrl Pts',(31.067,5.30690073322865,3.29228367909392));
#37816=CARTESIAN_POINT('Ctrl Pts',(31.067,5.39405337529976,3.16152164966802));
#37817=CARTESIAN_POINT('Ctrl Pts',(31.067,5.48890910442734,3.01920206705255));
#37818=CARTESIAN_POINT('Ctrl Pts',(31.067,5.57743177629917,2.87274515576473));
#37819=CARTESIAN_POINT('Ctrl Pts',(31.067,5.65961398733303,2.72265475190711));
#37820=CARTESIAN_POINT('Ctrl Pts',(31.067,5.71255046712117,2.62597619422109));
#37821=CARTESIAN_POINT('Ctrl Pts',(31.067,5.76285543012115,2.52778927668005));
#37822=CARTESIAN_POINT('Ctrl Pts',(31.067,5.81051785955815,2.42822180627828));
#37823=CARTESIAN_POINT('Ctrl Pts',(31.067,5.83809201900622,2.37061900807582));
#37824=CARTESIAN_POINT('Ctrl Pts',(31.067,5.86478159584491,2.31255405227071));
#37825=CARTESIAN_POINT('Ctrl Pts',(31.067,5.89058332834668,2.25405104435855));
#37826=CARTESIAN_POINT('Ctrl Pts',(31.067,5.9043177737656,2.22290947783945));
#37827=CARTESIAN_POINT('Ctrl Pts',(31.067,5.91780063355126,2.19164378162859));
#37828=CARTESIAN_POINT('Ctrl Pts',(31.067,5.93103131770442,2.160257546248));
#37829=CARTESIAN_POINT('Ctrl Pts',(31.067,5.94079597664893,2.13709352233995));
#37830=CARTESIAN_POINT('Ctrl Pts',(31.067,5.9504217117342,2.11386746706017));
#37831=CARTESIAN_POINT('Ctrl Pts',(31.067,5.95990532759805,2.0905886622763));
#37832=CARTESIAN_POINT('Ctrl Pts',(31.067,6.0261120429078,1.92807541593616));
#37833=CARTESIAN_POINT('Ctrl Pts',(31.067,6.08544315296794,1.76288224841305));
#37834=CARTESIAN_POINT('Ctrl Pts',(31.067,6.13789139515789,1.5955367961925));
#37835=CARTESIAN_POINT('Ctrl Pts',(31.067,6.19084866070303,1.42656721435372));
#37836=CARTESIAN_POINT('Ctrl Pts',(31.067,6.23678906352892,1.25540265586484));
#37837=CARTESIAN_POINT('Ctrl Pts',(31.067,6.27565901721259,1.08255884663743));
#37838=CARTESIAN_POINT('Ctrl Pts',(31.067,6.30838202285779,0.937048795580633));
#37839=CARTESIAN_POINT('Ctrl Pts',(31.067,6.33609328241928,0.790347903538514));
#37840=CARTESIAN_POINT('Ctrl Pts',(31.067,6.35873389224681,0.642754751803561));
#37841=CARTESIAN_POINT('Ctrl Pts',(31.067,6.36263630840976,0.61731507039662));
#37842=CARTESIAN_POINT('Ctrl Pts',(31.067,6.36638801856405,0.591848868190301));
#37843=CARTESIAN_POINT('Ctrl Pts',(31.067,6.36998864411347,0.566357661020381));
#37844=CARTESIAN_POINT('Ctrl Pts',(31.067,6.37338728944288,0.542296405274669));
#37845=CARTESIAN_POINT('Ctrl Pts',(31.067,6.37665015407961,0.518221047747062));
#37846=CARTESIAN_POINT('Ctrl Pts',(31.067,6.3797766793027,0.494137097499145));
#37847=CARTESIAN_POINT('Ctrl Pts',(31.067,6.39255495331688,0.395704718531514));
#37848=CARTESIAN_POINT('Ctrl Pts',(31.067,6.40305930999864,0.297106734753472));
#37849=CARTESIAN_POINT('Ctrl Pts',(31.067,6.41128905366097,0.198434233054838));
#37850=CARTESIAN_POINT('Ctrl Pts',(31.067,6.4260970453098,0.020890236415967));
#37851=CARTESIAN_POINT('Ctrl Pts',(31.067,6.433543840758,-0.15689427514383));
#37852=CARTESIAN_POINT('Ctrl Pts',(31.067,6.43375826100571,-0.334500592678881));
#37853=CARTESIAN_POINT('Ctrl Pts',(31.067,6.43397455628222,-0.513660014283607));
#37854=CARTESIAN_POINT('Ctrl Pts',(31.067,6.42683148569265,-0.692638769818387));
#37855=CARTESIAN_POINT('Ctrl Pts',(31.067,6.41240941578984,-0.871018380375883));
#37856=CARTESIAN_POINT('Ctrl Pts',(31.067,6.39782718168609,-1.0513789845066));
#37857=CARTESIAN_POINT('Ctrl Pts',(31.067,6.3758034632196,-1.23112777607217));
#37858=CARTESIAN_POINT('Ctrl Pts',(31.067,6.3463674681003,-1.40983329057961));
#37859=CARTESIAN_POINT('Ctrl Pts',(31.067,6.32429047176082,-1.54386242646019));
#37860=CARTESIAN_POINT('Ctrl Pts',(31.067,6.29804296076356,-1.67730481305471));
#37861=CARTESIAN_POINT('Ctrl Pts',(31.067,6.26761729626672,-1.80997509468729));
#37862=CARTESIAN_POINT('Ctrl Pts',(31.067,6.25927860899389,-1.8463357135013));
#37863=CARTESIAN_POINT('Ctrl Pts',(31.067,6.2506259889135,-1.88263831055097));
#37864=CARTESIAN_POINT('Ctrl Pts',(31.067,6.24165905425322,-1.91887900190174));
#37865=CARTESIAN_POINT('Ctrl Pts',(31.067,6.23650670208748,-1.93970270717483));
#37866=CARTESIAN_POINT('Ctrl Pts',(31.067,6.23125127551909,-1.96050299780219));
#37867=CARTESIAN_POINT('Ctrl Pts',(31.067,6.22589545585126,-1.98126916880994));
#37868=CARTESIAN_POINT('Ctrl Pts',(31.067,6.18033062290449,-2.1579381329641));
#37869=CARTESIAN_POINT('Ctrl Pts',(31.067,6.12745232170895,-2.33234672874841));
#37870=CARTESIAN_POINT('Ctrl Pts',(31.067,6.0673660129305,-2.50406902324849));
#37871=CARTESIAN_POINT('Ctrl Pts',(31.067,6.01225975549519,-2.66155869369896));
#37872=CARTESIAN_POINT('Ctrl Pts',(31.067,5.95109019025875,-2.81678940633195));
#37873=CARTESIAN_POINT('Ctrl Pts',(31.067,5.88390014609054,-2.96943153794234));
#37874=CARTESIAN_POINT('Ctrl Pts',(31.067,5.8114028299027,-3.1341307134815));
#37875=CARTESIAN_POINT('Ctrl Pts',(31.067,5.73189706641349,-3.29581698197365));
#37876=CARTESIAN_POINT('Ctrl Pts',(31.067,5.64574085447704,-3.45414022141883));
#37877=CARTESIAN_POINT('Ctrl Pts',(31.067,5.55896582325022,-3.61360062175447));
#37878=CARTESIAN_POINT('Ctrl Pts',(31.067,5.46544409047891,-3.7696501491991));
#37879=CARTESIAN_POINT('Ctrl Pts',(31.067,5.36549302718914,-3.92190981252245));
#37880=CARTESIAN_POINT('Ctrl Pts',(31.067,5.31398434674346,-4.00037515430829));
#37881=CARTESIAN_POINT('Ctrl Pts',(31.067,5.2607674524701,-4.07783360169406));
#37882=CARTESIAN_POINT('Ctrl Pts',(31.067,5.20588132288495,-4.15423023945157));
#37883=CARTESIAN_POINT('Ctrl Pts',(31.067,5.18904408415586,-4.177666186525));
#37884=CARTESIAN_POINT('Ctrl Pts',(31.067,5.17204974051512,-4.20100219435326));
#37885=CARTESIAN_POINT('Ctrl Pts',(31.067,5.15489936485222,-4.22423663144381));
#37886=CARTESIAN_POINT('Ctrl Pts',(31.067,5.14306101915661,-4.24027460657202));
#37887=CARTESIAN_POINT('Ctrl Pts',(31.067,5.13114984623005,-4.25626208650461));
#37888=CARTESIAN_POINT('Ctrl Pts',(31.067,5.11917153389746,-4.27219166789797));
#37889=CARTESIAN_POINT('Ctrl Pts',(31.067,5.00871211991934,-4.41908817358017));
#37890=CARTESIAN_POINT('Ctrl Pts',(31.067,4.89242109857996,-4.56123408705379));
#37891=CARTESIAN_POINT('Ctrl Pts',(31.067,4.77069968034181,-4.69828929887201));
#37892=CARTESIAN_POINT('Ctrl Pts',(31.067,4.64794056813919,-4.83651292762261));
#37893=CARTESIAN_POINT('Ctrl Pts',(31.067,4.51965767575762,-4.96955932709291));
#37894=CARTESIAN_POINT('Ctrl Pts',(31.067,4.3862135670772,-5.09705898614707));
#37895=CARTESIAN_POINT('Ctrl Pts',(31.067,4.25283777375098,-5.22449337304755));
#37896=CARTESIAN_POINT('Ctrl Pts',(31.067,4.11430557895959,-5.34638732154593));
#37897=CARTESIAN_POINT('Ctrl Pts',(31.067,3.97093688259113,-5.46234190382446));
#37898=CARTESIAN_POINT('Ctrl Pts',(31.067,3.92787994422503,-5.49716574911913));
#37899=CARTESIAN_POINT('Ctrl Pts',(31.067,3.88438652067304,-5.53145365890501));
#37900=CARTESIAN_POINT('Ctrl Pts',(31.067,3.84046463239738,-5.56519416757222));
#37901=CARTESIAN_POINT('Ctrl Pts',(31.067,3.72753604226176,-5.65194517541443));
#37902=CARTESIAN_POINT('Ctrl Pts',(31.067,3.61177574729217,-5.73507858328812));
#37903=CARTESIAN_POINT('Ctrl Pts',(31.067,3.49336789459867,-5.81452363421184));
#37904=CARTESIAN_POINT('Ctrl Pts',(31.067,3.44156445904527,-5.84928084399096));
#37905=CARTESIAN_POINT('Ctrl Pts',(31.067,3.38925412896203,-5.88333188073878));
#37906=CARTESIAN_POINT('Ctrl Pts',(31.067,3.33645174789616,-5.91666986399315));
#37907=CARTESIAN_POINT('Ctrl Pts',(31.067,3.30762568726353,-5.93486985246452));
#37908=CARTESIAN_POINT('Ctrl Pts',(31.067,3.27865297384291,-5.95285731744087));
#37909=CARTESIAN_POINT('Ctrl Pts',(31.067,3.24953598484261,-5.97063106297212));
#37910=CARTESIAN_POINT('Ctrl Pts',(31.067,3.22673123260147,-5.98455165974926));
#37911=CARTESIAN_POINT('Ctrl Pts',(31.067,3.20383615363947,-5.99834216605967));
#37912=CARTESIAN_POINT('Ctrl Pts',(31.067,3.18087127062506,-6.01199068150968));
#37913=CARTESIAN_POINT('Ctrl Pts',(31.067,3.02218322859531,-6.10630233953186));
#37914=CARTESIAN_POINT('Ctrl Pts',(31.067,2.85996735085955,-6.19395958629189));
#37915=CARTESIAN_POINT('Ctrl Pts',(31.067,2.69468188090138,-6.27489113780825));
#37916=CARTESIAN_POINT('Ctrl Pts',(31.067,2.52658802341311,-6.35719780814254));
#37917=CARTESIAN_POINT('Ctrl Pts',(31.067,2.35531886065546,-6.4325486765892));
#37918=CARTESIAN_POINT('Ctrl Pts',(31.067,2.18131982375181,-6.50082927234875));
#37919=CARTESIAN_POINT('Ctrl Pts',(31.067,2.0069903506746,-6.56923953766966));
#37920=CARTESIAN_POINT('Ctrl Pts',(31.067,1.82992000150959,-6.63055296436482));
#37921=CARTESIAN_POINT('Ctrl Pts',(31.067,1.65052909766165,-6.68460995303681));
#37922=CARTESIAN_POINT('Ctrl Pts',(31.067,1.472830493977,-6.73815699026314));
#37923=CARTESIAN_POINT('Ctrl Pts',(31.067,1.29285426780137,-6.78458408156556));
#37924=CARTESIAN_POINT('Ctrl Pts',(31.067,1.11099136235469,-6.82368859152074));
#37925=CARTESIAN_POINT('Ctrl Pts',(31.067,0.984463770055063,-6.85089479654938));
#37926=CARTESIAN_POINT('Ctrl Pts',(31.067,0.857022575344876,-6.87455559284932));
#37927=CARTESIAN_POINT('Ctrl Pts',(31.067,0.728796816010263,-6.89458803707468));
#37928=CARTESIAN_POINT('Ctrl Pts',(31.067,5.1168550999138,3.5431531688378));
#37929=CARTESIAN_POINT('Ctrl Pts',(31.1281503528974,4.01942676905249,5.1044661434557));
#37930=CARTESIAN_POINT('Ctrl Pts',(31.2554712406089,0.166680189710837,7.26913646933564));
#37931=CARTESIAN_POINT('Ctrl Pts',(31.4236261011954,-5.20334138794374,4.63644610479065));
#37932=CARTESIAN_POINT('Ctrl Pts',(31.5306306088845,-6.20309813924992,1.27936691419838));
#37933=CARTESIAN_POINT('Ctrl Pts',(31.5714645817597,-6.20816386984268,-0.000295703980951051));
#37934=CARTESIAN_POINT('Origin',(31.067,-1.12618006296016E-15,0.));
#37935=CARTESIAN_POINT('',(31.067,-1.68325362372072,5.98713018070687));
#37936=CARTESIAN_POINT('Ctrl Pts',(31.067,-4.95966987665984,-4.85170944379069));
#37937=CARTESIAN_POINT('Ctrl Pts',(31.067,-5.07635566737652,-4.72174660294797));
#37938=CARTESIAN_POINT('Ctrl Pts',(31.067,-5.18774208410829,-4.5873676703608));
#37939=CARTESIAN_POINT('Ctrl Pts',(31.067,-5.2934659950304,-4.44869245219079));
#37940=CARTESIAN_POINT('Ctrl Pts',(31.067,-5.40677951528188,-4.30006214703625));
#37941=CARTESIAN_POINT('Ctrl Pts',(31.067,-5.51358913810325,-4.14649635317199));
#37942=CARTESIAN_POINT('Ctrl Pts',(31.067,-5.61378552910678,-3.98851757493328));
#37943=CARTESIAN_POINT('Ctrl Pts',(31.067,-5.67722095415703,-3.88849949198516));
#37944=CARTESIAN_POINT('Ctrl Pts',(31.067,-5.73800468699189,-3.78671197565764));
#37945=CARTESIAN_POINT('Ctrl Pts',(31.067,-5.79609912672184,-3.68328336482282));
#37946=CARTESIAN_POINT('Ctrl Pts',(31.067,-5.8261073502107,-3.62985813370775));
#37947=CARTESIAN_POINT('Ctrl Pts',(31.067,-5.85539790107394,-3.57599498956757));
#37948=CARTESIAN_POINT('Ctrl Pts',(31.067,-5.88396477006812,-3.52171140149403));
#37949=CARTESIAN_POINT('Ctrl Pts',(31.067,-5.90334141911564,-3.48489133432616));
#37950=CARTESIAN_POINT('Ctrl Pts',(31.067,-5.9223851058769,-3.44787782708014));
#37951=CARTESIAN_POINT('Ctrl Pts',(31.067,-5.94109380441469,-3.41067630557261));
#37952=CARTESIAN_POINT('Ctrl Pts',(31.067,-5.95476449124947,-3.38349267495931));
#37953=CARTESIAN_POINT('Ctrl Pts',(31.067,-5.9682569544298,-3.35620718712805));
#37954=CARTESIAN_POINT('Ctrl Pts',(31.067,-5.98156221116727,-3.32883915699247));
#37955=CARTESIAN_POINT('Ctrl Pts',(31.067,-6.0632846669316,-3.16074148881201));
#37956=CARTESIAN_POINT('Ctrl Pts',(31.067,-6.13802128983771,-2.98938944330838));
#37957=CARTESIAN_POINT('Ctrl Pts',(31.067,-6.20566688241296,-2.81530388884709));
#37958=CARTESIAN_POINT('Ctrl Pts',(31.067,-6.27332997004571,-2.64117331095313));
#37959=CARTESIAN_POINT('Ctrl Pts',(31.067,-6.33389852210686,-2.46430702539236));
#37960=CARTESIAN_POINT('Ctrl Pts',(31.067,-6.3872172336922,-2.28521174662972));
#37961=CARTESIAN_POINT('Ctrl Pts',(31.067,-6.43351747954507,-2.12969119500265));
#37962=CARTESIAN_POINT('Ctrl Pts',(31.067,-6.47435018799297,-1.97248931528049));
#37963=CARTESIAN_POINT('Ctrl Pts',(31.067,-6.50958159881369,-1.81393587356536));
#37964=CARTESIAN_POINT('Ctrl Pts',(31.067,-6.5162987831482,-1.78370623841702));
#37965=CARTESIAN_POINT('Ctrl Pts',(31.067,-6.52281226624634,-1.75342747784606));
#37966=CARTESIAN_POINT('Ctrl Pts',(31.067,-6.5291209938122,-1.72310188852852));
#37967=CARTESIAN_POINT('Ctrl Pts',(31.067,-6.53378997379954,-1.70065844519546));
#37968=CARTESIAN_POINT('Ctrl Pts',(31.067,-6.53834599767253,-1.67819309129953));
#37969=CARTESIAN_POINT('Ctrl Pts',(31.067,-6.54278721332838,-1.65571492114972));
#37970=CARTESIAN_POINT('Ctrl Pts',(31.067,-6.56381992769274,-1.54926277632505));
#37971=CARTESIAN_POINT('Ctrl Pts',(31.067,-6.58228961498628,-1.44246888520439));
#37972=CARTESIAN_POINT('Ctrl Pts',(31.067,-6.59817669086173,-1.33543377907857));
#37973=CARTESIAN_POINT('Ctrl Pts',(31.067,-6.62523147934088,-1.15315906856664));
#37974=CARTESIAN_POINT('Ctrl Pts',(31.067,-6.64479957064315,-0.970184910999771));
#37975=CARTESIAN_POINT('Ctrl Pts',(31.067,-6.6569284968028,-0.786934728926997));
#37976=CARTESIAN_POINT('Ctrl Pts',(31.067,-6.66907982591669,-0.603346071263836));
#37977=CARTESIAN_POINT('Ctrl Pts',(31.067,-6.67376443191619,-0.419479680282065));
#37978=CARTESIAN_POINT('Ctrl Pts',(31.067,-6.67097793043684,-0.235762076334595));
#37979=CARTESIAN_POINT('Ctrl Pts',(31.067,-6.66818244407636,-0.0514520876912934));
#37980=CARTESIAN_POINT('Ctrl Pts',(31.067,-6.65786756519682,0.132708849422281));
#37981=CARTESIAN_POINT('Ctrl Pts',(31.067,-6.63997697058196,0.316278910548742));
#37982=CARTESIAN_POINT('Ctrl Pts',(31.067,-6.62655902462081,0.453956456393588));
#37983=CARTESIAN_POINT('Ctrl Pts',(31.067,-6.60887867008592,0.591301469579883));
#37984=CARTESIAN_POINT('Ctrl Pts',(31.067,-6.58689321254617,0.728119878393478));
#37985=CARTESIAN_POINT('Ctrl Pts',(31.067,-6.57965626197951,0.773156378516489));
#37986=CARTESIAN_POINT('Ctrl Pts',(31.067,-6.5719527115053,0.818135753944776));
#37987=CARTESIAN_POINT('Ctrl Pts',(31.067,-6.5637806567902,0.863050874087544));
#37988=CARTESIAN_POINT('Ctrl Pts',(31.067,-6.55946815526574,0.886753177956007));
#37989=CARTESIAN_POINT('Ctrl Pts',(31.067,-6.55502649277326,0.910430215125999));
#37990=CARTESIAN_POINT('Ctrl Pts',(31.067,-6.55045718629041,0.934073267148448));
#37991=CARTESIAN_POINT('Ctrl Pts',(31.067,-6.51616820861596,1.11149539586711));
#37992=CARTESIAN_POINT('Ctrl Pts',(31.067,-6.47467065207115,1.28714095330058));
#37993=CARTESIAN_POINT('Ctrl Pts',(31.067,-6.42598064130125,1.46061043020915));
#37994=CARTESIAN_POINT('Ctrl Pts',(31.067,-6.38139733331752,1.61944882421442));
#37995=CARTESIAN_POINT('Ctrl Pts',(31.067,-6.33078305800691,1.77646305987751));
#37996=CARTESIAN_POINT('Ctrl Pts',(31.067,-6.27411319884471,1.93133634328533));
#37997=CARTESIAN_POINT('Ctrl Pts',(31.067,-6.21205804932745,2.1009271081149));
#37998=CARTESIAN_POINT('Ctrl Pts',(31.067,-6.14274198333447,2.26795156050715));
#37999=CARTESIAN_POINT('Ctrl Pts',(31.067,-6.06645428682219,2.43198635086053));
#38000=CARTESIAN_POINT('Ctrl Pts',(31.067,-5.99042918402894,2.59545650880764));
#38001=CARTESIAN_POINT('Ctrl Pts',(31.067,-5.90747986319118,2.75595816053323));
#38002=CARTESIAN_POINT('Ctrl Pts',(31.067,-5.81785241493192,2.91304016625822));
#38003=CARTESIAN_POINT('Ctrl Pts',(31.067,-5.77330574632114,2.99111312481782));
#38004=CARTESIAN_POINT('Ctrl Pts',(31.067,-5.72710880713813,3.0683407746618));
#38005=CARTESIAN_POINT('Ctrl Pts',(31.067,-5.67928867316067,3.14466404153542));
#38006=CARTESIAN_POINT('Ctrl Pts',(31.067,-5.66592045077483,3.16600037667119));
#38007=CARTESIAN_POINT('Ctrl Pts',(31.067,-5.6524253652407,3.18726601863544));
#38008=CARTESIAN_POINT('Ctrl Pts',(31.067,-5.63880398215889,3.20845963827975));
#38009=CARTESIAN_POINT('Ctrl Pts',(31.067,-5.62723633649404,3.22645783133611));
#38010=CARTESIAN_POINT('Ctrl Pts',(31.067,-5.61557834605993,3.24440285810145));
#38011=CARTESIAN_POINT('Ctrl Pts',(31.067,-5.6038372074752,3.2622837478132));
#38012=CARTESIAN_POINT('Ctrl Pts',(31.067,-5.50559617042605,3.41189761498358));
#38013=CARTESIAN_POINT('Ctrl Pts',(31.067,-5.40141185916998,3.55721997451032));
#38014=CARTESIAN_POINT('Ctrl Pts',(31.067,-5.29159672322233,3.69786677176514));
#38015=CARTESIAN_POINT('Ctrl Pts',(31.067,-5.18185629256696,3.83841788949447));
#38016=CARTESIAN_POINT('Ctrl Pts',(31.067,-5.06649219437619,3.97430040459667));
#38017=CARTESIAN_POINT('Ctrl Pts',(31.067,-4.9457752208923,4.10509926031028));
#38018=CARTESIAN_POINT('Ctrl Pts',(31.067,-4.82662308589716,4.23420258740186));
#38019=CARTESIAN_POINT('Ctrl Pts',(31.067,-4.70225542548044,4.35835368787749));
#38020=CARTESIAN_POINT('Ctrl Pts',(31.067,-4.57290041499668,4.47711448579565));
#38021=CARTESIAN_POINT('Ctrl Pts',(31.067,-4.5364413095177,4.51058758004899));
#38022=CARTESIAN_POINT('Ctrl Pts',(31.067,-4.49958583096963,4.54363219780854));
#38023=CARTESIAN_POINT('Ctrl Pts',(31.067,-4.46233870438039,4.5762378790869));
#38024=CARTESIAN_POINT('Ctrl Pts',(31.067,-4.36358707308753,4.6626838552064));
#38025=CARTESIAN_POINT('Ctrl Pts',(31.067,-4.26208285674386,4.7460454941142));
#38026=CARTESIAN_POINT('Ctrl Pts',(31.067,-4.15797763636354,4.82622587042557));
#38027=CARTESIAN_POINT('Ctrl Pts',(31.067,-4.11243160244716,4.86130478506179));
#38028=CARTESIAN_POINT('Ctrl Pts',(31.067,-4.06638765091281,4.89577460051552));
#38029=CARTESIAN_POINT('Ctrl Pts',(31.067,-4.01985820004502,4.92962631219268));
#38030=CARTESIAN_POINT('Ctrl Pts',(31.067,-3.99192547401397,4.94994829257984));
#38031=CARTESIAN_POINT('Ctrl Pts',(31.067,-3.96381777685901,4.97004750497133));
#38032=CARTESIAN_POINT('Ctrl Pts',(31.067,-3.93553777385799,4.9899219041749));
#38033=CARTESIAN_POINT('Ctrl Pts',(31.067,-3.91343652477951,5.0054540470487));
#38034=CARTESIAN_POINT('Ctrl Pts',(31.067,-3.89122738800398,5.02085061138));
#38035=CARTESIAN_POINT('Ctrl Pts',(31.067,-3.86893240489384,5.03609662377786));
#38036=CARTESIAN_POINT('Ctrl Pts',(31.067,-3.72457833794962,5.13481048614953));
#38037=CARTESIAN_POINT('Ctrl Pts',(31.067,-3.5764575554336,5.22733828199603));
#38038=CARTESIAN_POINT('Ctrl Pts',(31.067,-3.4249789067786,5.31353849959259));
#38039=CARTESIAN_POINT('Ctrl Pts',(31.067,-3.27256982914678,5.40026818573783));
#38040=CARTESIAN_POINT('Ctrl Pts',(31.067,-3.11676086341988,5.48059262935479));
#38041=CARTESIAN_POINT('Ctrl Pts',(31.067,-2.95794275057018,5.55432203962601));
#38042=CARTESIAN_POINT('Ctrl Pts',(31.067,-2.79994827293749,5.62766908709402));
#38043=CARTESIAN_POINT('Ctrl Pts',(31.067,-2.63897511619471,5.69448954961524));
#38044=CARTESIAN_POINT('Ctrl Pts',(31.067,-2.47539248397361,5.75454770723132));
#38045=CARTESIAN_POINT('Ctrl Pts',(31.067,-2.31473325949493,5.81353255724385));
#38046=CARTESIAN_POINT('Ctrl Pts',(31.067,-2.1515563817662,5.86599474730277));
#38047=CARTESIAN_POINT('Ctrl Pts',(31.067,-1.98620606863935,5.91166147165176));
#38048=CARTESIAN_POINT('Ctrl Pts',(31.067,-1.88599462349867,5.93933803515691));
#38049=CARTESIAN_POINT('Ctrl Pts',(31.067,-1.78498480160803,5.96451763689186));
#38050=CARTESIAN_POINT('Ctrl Pts',(31.067,-1.68325362372016,5.98713018070703));
#38051=CARTESIAN_POINT('Origin',(31.067,0.,0.));
#38052=CARTESIAN_POINT('Origin',(28.1999754182402,0.,0.));
#38053=CARTESIAN_POINT('Ctrl Pts',(31.067,-1.68325362372015,5.98713018070703));
#38054=CARTESIAN_POINT('Ctrl Pts',(31.100085267407,-2.67894146944392,5.70719720383451));
#38055=CARTESIAN_POINT('Ctrl Pts',(31.166255802221,-4.52416925940906,4.64399692160856));
#38056=CARTESIAN_POINT('Ctrl Pts',(31.2522476083012,-5.97677244814931,2.2702138283845));
#38057=CARTESIAN_POINT('Ctrl Pts',(31.3051541469743,-6.21736961784573,0.620749375332392));
#38058=CARTESIAN_POINT('Ctrl Pts',(31.3249754182403,-6.21654608244749,0.00207115560223001));
#38059=CARTESIAN_POINT('Ctrl Pts',(30.6549162453659,-1.87643162330758,6.67424103273558));
#38060=CARTESIAN_POINT('Ctrl Pts',(30.6880015127729,-2.98638922822823,6.36218164797731));
#38061=CARTESIAN_POINT('Ctrl Pts',(30.754172047587,-5.04338392498871,5.17696356594593));
#38062=CARTESIAN_POINT('Ctrl Pts',(30.853427849808,-6.91246875169278,2.12258368035554));
#38063=CARTESIAN_POINT('Ctrl Pts',(30.952683652029,-7.07320345546478,-1.42613979719881));
#38064=CARTESIAN_POINT('Ctrl Pts',(31.0850247216572,-5.03913679692803,-5.74620551731878));
#38065=CARTESIAN_POINT('Ctrl Pts',(31.2504510586922,1.01637773032965,-8.13586156489377));
#38066=CARTESIAN_POINT('Ctrl Pts',(31.4489626631344,7.40108795243844,-3.53348110298655));
#38067=CARTESIAN_POINT('Ctrl Pts',(31.6143890001694,7.04014314253548,2.9701480866463));
#38068=CARTESIAN_POINT('Ctrl Pts',(31.7467300697975,3.58881749933384,6.25980480689558));
#38069=CARTESIAN_POINT('Ctrl Pts',(31.8459858720186,0.159432186662248,7.23304908842483));
#38070=CARTESIAN_POINT('Ctrl Pts',(31.9452416742397,-3.30635190225879,6.4120734720337));
#38071=CARTESIAN_POINT('Ctrl Pts',(32.0775827438677,-6.90505735872034,3.28023028088796));
#38072=CARTESIAN_POINT('Ctrl Pts',(32.2430090809028,-7.54381322647391,-3.20505761210972));
#38073=CARTESIAN_POINT('Ctrl Pts',(32.4415206853449,-1.38653337747383,-8.07830009000535));
#38074=CARTESIAN_POINT('Ctrl Pts',(32.640032289787,6.03340921861916,-5.54788315750085));
#38075=CARTESIAN_POINT('Ctrl Pts',(32.8385438942292,7.93033714683168,2.07205611235235));
#38076=CARTESIAN_POINT('Ctrl Pts',(33.0039702312642,3.46180249906012,6.81563813838305));
#38077=CARTESIAN_POINT('Ctrl Pts',(33.1363113008923,-1.29997896114567,7.09628287091765));
#38078=CARTESIAN_POINT('Ctrl Pts',(33.2355671031133,-4.54639362325622,5.62827366693923));
#38079=CARTESIAN_POINT('Ctrl Pts',(33.3348229053344,-6.66425465276717,2.76313547380338));
#38080=CARTESIAN_POINT('Ctrl Pts',(33.4671639749625,-7.39119473715877,-1.95117347127662));
#38081=CARTESIAN_POINT('Ctrl Pts',(33.6325903119975,-3.693357430702,-7.31732226708638));
#38082=CARTESIAN_POINT('Ctrl Pts',(33.8311019164397,4.15513537654513,-7.06509570019544));
#38083=CARTESIAN_POINT('Ctrl Pts',(34.0296135208818,8.18919366122636,-0.343265517627367));
#38084=CARTESIAN_POINT('Ctrl Pts',(34.2281251253239,4.71981863488245,6.70129840887398));
#38085=CARTESIAN_POINT('Ctrl Pts',(34.393551462359,-1.75502246952579,7.44021165588655));
#38086=CARTESIAN_POINT('Ctrl Pts',(34.525892531987,-5.57321788935264,4.58109536851286));
#38087=CARTESIAN_POINT('Ctrl Pts',(34.6251483342082,-7.10531700255993,1.36442061554992));
#38088=CARTESIAN_POINT('Ctrl Pts',(34.7244041364292,-6.87364072807772,-2.19094856972063));
#38089=CARTESIAN_POINT('Ctrl Pts',(34.8567452060573,-4.38603192732624,-6.26095659180019));
#38090=CARTESIAN_POINT('Ctrl Pts',(35.0221715430924,1.90196620680996,-7.97286720693537));
#38091=CARTESIAN_POINT('Ctrl Pts',(35.2206831475345,7.73386740697045,-2.71440995635487));
#38092=CARTESIAN_POINT('Ctrl Pts',(35.4191947519766,6.47649012537996,5.02352487399142));
#38093=CARTESIAN_POINT('Ctrl Pts',(35.6177063564187,-0.720339615174119,
8.16487585904735));
#38094=CARTESIAN_POINT('Ctrl Pts',(35.7831326934538,-6.14277290065803,4.55007632360081));
#38095=CARTESIAN_POINT('Ctrl Pts',(35.9154737630819,-7.21370596289137,-0.0981776753163467));
#38096=CARTESIAN_POINT('Ctrl Pts',(36.0147295653029,-6.30772612813385,-3.54397577118503));
#38097=CARTESIAN_POINT('Ctrl Pts',(36.113985367524,-3.83595946031657,-6.11004153773871));
#38098=CARTESIAN_POINT('Ctrl Pts',(36.246326437152,0.691068351408432,-7.61309910580096));
#38099=CARTESIAN_POINT('Ctrl Pts',(36.4117527741872,6.59881128900457,-4.86207533144359));
#38100=CARTESIAN_POINT('Ctrl Pts',(36.6102643786292,7.65916482667057,2.91854769567105));
#38101=CARTESIAN_POINT('Ctrl Pts',(36.8087759830714,1.70432940577044,8.01723067963919));
#38102=CARTESIAN_POINT('Ctrl Pts',(37.0072875875134,-5.82021344348282,5.77141251591789));
#38103=CARTESIAN_POINT('Ctrl Pts',(37.1727139245487,-7.62871246207274,-0.489489154279525));
#38104=CARTESIAN_POINT('Ctrl Pts',(37.3050549941766,-5.44648042441822,-4.73107213644686));
#38105=CARTESIAN_POINT('Ctrl Pts',(37.4043107963977,-2.53040138538347,-6.77821820272855));
#38106=CARTESIAN_POINT('Ctrl Pts',(37.5035665986188,1.01380720327794,-7.14278569806071));
#38107=CARTESIAN_POINT('Ctrl Pts',(37.6359076682468,5.44171187513046,-5.36885698535498));
#38108=CARTESIAN_POINT('Ctrl Pts',(37.8013340052819,8.17841552233659,0.545533225941051));
#38109=CARTESIAN_POINT('Ctrl Pts',(37.999845609724,3.96631642533182,7.17280004657078));
#38110=CARTESIAN_POINT('Ctrl Pts',(38.1983572141662,-3.87294681277729,7.22364239697269));
#38111=CARTESIAN_POINT('Ctrl Pts',(38.3968688186083,-8.17065160671188,0.65156678731938));
#38112=CARTESIAN_POINT('Ctrl Pts',(38.5622951556433,-5.51089172685842,-5.29782274486176));
#38113=CARTESIAN_POINT('Ctrl Pts',(38.6946362252715,-1.10636856916135,-7.12903507937862));
#38114=CARTESIAN_POINT('Ctrl Pts',(38.7938920274925,2.44227055290094,-6.81046897954778));
#38115=CARTESIAN_POINT('Ctrl Pts',(38.8931478297135,5.38465712099301,-4.80131859630022));
#38116=CARTESIAN_POINT('Ctrl Pts',(39.0254888993417,7.62172171751438,-0.588397418332726));
#38117=CARTESIAN_POINT('Ctrl Pts',(39.1909152363767,5.89458286590277,5.69543499599519));
#38118=CARTESIAN_POINT('Ctrl Pts',(39.3894268408188,-1.60019725410325,8.03866252817617));
#38119=CARTESIAN_POINT('Ctrl Pts',(39.5879384452609,-7.62066502615036,3.01764660839399));
#38120=CARTESIAN_POINT('Ctrl Pts',(39.786450049703,-6.66132050968186,-4.77607537879091));
#38121=CARTESIAN_POINT('Ctrl Pts',(39.9518763867381,-0.789757142543198,
-7.60349505930879));
#38122=CARTESIAN_POINT('Ctrl Pts',(40.0842174563662,3.75638549375725,-6.15928247413035));
#38123=CARTESIAN_POINT('Ctrl Pts',(40.1834732585872,6.26122779876381,-3.62549301846479));
#38124=CARTESIAN_POINT('Ctrl Pts',(40.2827290608083,7.21182569809585,-0.191735948959446));
#38125=CARTESIAN_POINT('Ctrl Pts',(40.4150701304364,6.20127365133498,4.47001773625));
#38126=CARTESIAN_POINT('Ctrl Pts',(40.5804964674715,0.826182852666716,8.1548457281889));
#38127=CARTESIAN_POINT('Ctrl Pts',(40.7790080719136,-6.41078686909009,5.1071066381118));
#38128=CARTESIAN_POINT('Ctrl Pts',(40.9775196763557,-7.76842450593914,-2.61386824256068));
#38129=CARTESIAN_POINT('Ctrl Pts',(41.1760312807978,-2.00521956202275,-7.94752675142916));
#38130=CARTESIAN_POINT('Ctrl Pts',(41.3414576178329,4.30445421564323,-6.31731963466804));
#38131=CARTESIAN_POINT('Ctrl Pts',(41.473798687461,6.84464445440369,-2.27991992548857));
#38132=CARTESIAN_POINT('Ctrl Pts',(41.573054489682,7.12241671079052,1.27214518542566));
#38133=CARTESIAN_POINT('Ctrl Pts',(41.6723102919031,5.63216891050179,4.5084216681025));
#38134=CARTESIAN_POINT('Ctrl Pts',(41.8046513615311,1.8513792489286,7.41682198369137));
#38135=CARTESIAN_POINT('Ctrl Pts',(41.9700776985663,-4.6325012323385,6.76195380707258));
#38136=CARTESIAN_POINT('Ctrl Pts',(42.1685893030084,-8.19295729764973,-0.237017326015257));
#38137=CARTESIAN_POINT('Ctrl Pts',(42.3671009074505,-4.24642451586804,-7.01060663031227));
#38138=CARTESIAN_POINT('Ctrl Pts',(42.5656125118925,3.59813568041071,-7.36461177401473));
#38139=CARTESIAN_POINT('Ctrl Pts',(42.7310388489278,7.36526593039372,-2.04687841253758));
#38140=CARTESIAN_POINT('Ctrl Pts',(42.8633799185557,6.69953237756773,2.67646380430612));
#38141=CARTESIAN_POINT('Ctrl Pts',(42.9626357207769,4.61901655424491,5.56882925277487));
#38142=CARTESIAN_POINT('Ctrl Pts',(43.0618915229978,1.39190762332577,7.07882657945274));
#38143=CARTESIAN_POINT('Ctrl Pts',(43.194232592626,-3.37309616097341,6.85996178924909));
#38144=CARTESIAN_POINT('Ctrl Pts',(43.359658929661,-7.90281813252849,2.17475343907767));
#38145=CARTESIAN_POINT('Ctrl Pts',(43.5581705341032,-6.10482138465689,-5.46917565592653));
#38146=CARTESIAN_POINT('Ctrl Pts',(43.7566821385453,1.28156221813536,-8.09557439438308));
#38147=CARTESIAN_POINT('Ctrl Pts',(43.9551937429874,7.50175213064336,-3.30269616025889));
#38148=CARTESIAN_POINT('Ctrl Pts',(44.1206200800225,6.94676798905697,3.19049650796619));
#38149=CARTESIAN_POINT('Ctrl Pts',(44.2529611496505,3.38959938145578,6.368501284217));
#38150=CARTESIAN_POINT('Ctrl Pts',(44.3522169518717,-0.0663807020241724,
7.23483011392448));
#38151=CARTESIAN_POINT('Ctrl Pts',(44.4514727540926,-3.50588289361426,6.30523415188539));
#38152=CARTESIAN_POINT('Ctrl Pts',(44.5838138237208,-7.00414016531606,3.06249473562607));
#38153=CARTESIAN_POINT('Ctrl Pts',(44.7492401607558,-7.43988877947175,-3.43978806115894));
#38154=CARTESIAN_POINT('Ctrl Pts',(44.947751765198,-1.13280263660267,-8.11772657093409));
#38155=CARTESIAN_POINT('Ctrl Pts',(45.1462633696401,6.20414626300639,-5.35623894548842));
#38156=CARTESIAN_POINT('Ctrl Pts',(45.3447749740821,7.86158362152895,2.31939429987847));
#38157=CARTESIAN_POINT('Ctrl Pts',(45.5102013111174,3.24665643439725,6.92069905848522));
#38158=CARTESIAN_POINT('Ctrl Pts',(45.6425423807453,-1.52156104753122,7.05209504703919));
#38159=CARTESIAN_POINT('Ctrl Pts',(45.7417981829665,-4.72042009291361,5.48313845542561));
#38160=CARTESIAN_POINT('Ctrl Pts',(45.8410539851874,-6.74751430915288,2.55308504002825));
#38161=CARTESIAN_POINT('Ctrl Pts',(45.9733950548156,-7.32646826719433,-2.18167738011961));
#38162=CARTESIAN_POINT('Ctrl Pts',(46.1388213918505,-3.46239836164604,-7.42939328221839));
#38163=CARTESIAN_POINT('Ctrl Pts',(46.3373329962928,4.37434562194319,-6.93150971100306));
#38164=CARTESIAN_POINT('Ctrl Pts',(46.5358446007348,8.19592696626587,-0.0866467401548151));
#38165=CARTESIAN_POINT('Ctrl Pts',(46.734356205177,4.50764780719777,6.8458161093376));
#38166=CARTESIAN_POINT('Ctrl Pts',(46.899782542212,-1.98715711947764,7.381602809935));
#38167=CARTESIAN_POINT('Ctrl Pts',(47.0321236118402,-5.71394470796255,4.40431929453189));
#38168=CARTESIAN_POINT('Ctrl Pts',(47.1313794140611,-7.14455993023938,1.14124343510381));
#38169=CARTESIAN_POINT('Ctrl Pts',(47.2306352162823,-6.80165841434973,-2.40512689651597));
#38170=CARTESIAN_POINT('Ctrl Pts',(47.3629762859103,-4.18781450800034,-6.39523753333001));
#38171=CARTESIAN_POINT('Ctrl Pts',(47.5284026229455,2.15070931246681,-7.90939545160498));
#38172=CARTESIAN_POINT('Ctrl Pts',(47.7269142273875,7.81507793497872,-2.47088716135563));
#38173=CARTESIAN_POINT('Ctrl Pts',(47.9254258318296,6.31599847344063,5.2238768914896));
#38174=CARTESIAN_POINT('Ctrl Pts',(48.1239374362717,-0.975675145363378,
8.13831339819997));
#38175=CARTESIAN_POINT('Ctrl Pts',(48.2893637733068,-6.28224897351141,4.35547945649454));
#38176=CARTESIAN_POINT('Ctrl Pts',(48.4217048429349,-7.20709344807375,-0.324031795618007));
#38177=CARTESIAN_POINT('Ctrl Pts',(48.5209606451559,-6.19365036830372,-3.7397684808235));
#38178=CARTESIAN_POINT('Ctrl Pts',(48.620216447377,-3.64273784243868,-6.22717059225972));
#38179=CARTESIAN_POINT('Ctrl Pts',(48.752557517005,0.929138961386053,-7.58772391772166));
#38180=CARTESIAN_POINT('Ctrl Pts',(48.9179838540402,6.74783416273851,-4.65304427969263));
#38181=CARTESIAN_POINT('Ctrl Pts',(49.1164954584823,7.56401196412085,3.15696840348137));
#38182=CARTESIAN_POINT('Ctrl Pts',(49.3150070629244,1.4524282921612,8.06667084676652));
#38183=CARTESIAN_POINT('Ctrl Pts',(49.5135186673665,-5.99809471893604,5.58631781223311));
#38184=CARTESIAN_POINT('Ctrl Pts',(49.6789450044016,-7.60964221054302,-0.728147573403291));
#38185=CARTESIAN_POINT('Ctrl Pts',(49.8112860740297,-5.29565231143276,-4.89931211194549));
#38186=CARTESIAN_POINT('Ctrl Pts',(49.9105418762507,-2.31689566560535,-6.85413507669997));
#38187=CARTESIAN_POINT('Ctrl Pts',(50.0097976784718,1.23699132885906,-7.10753438445193));
#38188=CARTESIAN_POINT('Ctrl Pts',(50.1421387480998,5.60717247991814,-5.19581276044276));
#38189=CARTESIAN_POINT('Ctrl Pts',(50.307565085135,8.15732060565719,0.801378495544836));
#38190=CARTESIAN_POINT('Ctrl Pts',(50.5060766895771,3.73974984335584,7.29349008383935));
#38191=CARTESIAN_POINT('Ctrl Pts',(50.7045882940192,-4.09726073797571,7.09881546027125));
#38192=CARTESIAN_POINT('Ctrl Pts',(50.9030998984613,-8.18704852617428,0.395377524233446));
#38193=CARTESIAN_POINT('Ctrl Pts',(51.0685262354963,-5.34228382927205,-5.46780183882237));
#38194=CARTESIAN_POINT('Ctrl Pts',(51.2008673051245,-0.882575199040403,
-7.1601853042975));
#38195=CARTESIAN_POINT('Ctrl Pts',(51.3001231073455,2.65434734717859,-6.7306473192016));
#38196=CARTESIAN_POINT('Ctrl Pts',(51.3993789095665,5.5323728451407,-4.63033943423036));
#38197=CARTESIAN_POINT('Ctrl Pts',(51.5317199791947,7.63640967023901,-0.349429262385304));
#38198=CARTESIAN_POINT('Ctrl Pts',(51.6971463162297,5.7133352772524,5.87723463597501));
#38199=CARTESIAN_POINT('Ctrl Pts',(51.8956579206719,-1.85114879322649,7.98460860902268));
#38200=CARTESIAN_POINT('Ctrl Pts',(52.0941695251139,-7.71142714287807,2.77752010146219));
#38201=CARTESIAN_POINT('Ctrl Pts',(52.2926811295562,-6.50848726183514,-4.98233685323774));
#38202=CARTESIAN_POINT('Ctrl Pts',(52.4581074665911,-0.551261008942458,
-7.6244976727094));
#38203=CARTESIAN_POINT('Ctrl Pts',(52.5904485362193,3.94742540820808,-6.03862775972094));
#38204=CARTESIAN_POINT('Ctrl Pts',(52.6897043384403,6.37169179839973,-3.42764012130142));
#38205=CARTESIAN_POINT('Ctrl Pts',(52.7889601406614,7.21429295444991,0.0342014796987391));
#38206=CARTESIAN_POINT('Ctrl Pts',(52.9213012102894,6.05825044682572,4.66202262807325));
#38207=CARTESIAN_POINT('Ctrl Pts',(53.0867275473245,0.570402920122291,8.17671862456552));
#38208=CARTESIAN_POINT('Ctrl Pts',(53.2852391517666,-6.56757528827362,4.90384352592947));
#38209=CARTESIAN_POINT('Ctrl Pts',(53.4837507562088,-7.68275930744305,-2.85585992615889));
#38210=CARTESIAN_POINT('Ctrl Pts',(53.6822623606508,-1.75535370226148,-8.00642369204619));
#38211=CARTESIAN_POINT('Ctrl Pts',(53.847688697686,4.50017437076574,-6.17942425261726));
#38212=CARTESIAN_POINT('Ctrl Pts',(53.980029767314,6.91268474619889,-2.06445687131224));
#38213=CARTESIAN_POINT('Ctrl Pts',(54.0792855695351,7.07908535181276,1.49456473820969));
#38214=CARTESIAN_POINT('Ctrl Pts',(54.1785413717561,5.48822218121968,4.68258580950818));
#38215=CARTESIAN_POINT('Ctrl Pts',(54.3108824413843,1.61820823400769,7.47116159459295));
#38216=CARTESIAN_POINT('Ctrl Pts',(54.4763087784192,-4.84198452615164,6.61356732823588));
#38217=CARTESIAN_POINT('Ctrl Pts',(54.6748203828615,-8.18151664109748,-0.49346929528404));
#38218=CARTESIAN_POINT('Ctrl Pts',(54.8733319873035,-4.02479975377234,-7.14014799818442));
#38219=CARTESIAN_POINT('Ctrl Pts',(55.0718435917456,3.82699894374387,-7.24832160166644));
#38220=CARTESIAN_POINT('Ctrl Pts',(55.2372699287808,7.42575302102872,-1.81522602774813));
#38221=CARTESIAN_POINT('Ctrl Pts',(55.3696109984087,6.61243120057668,2.88495167922774));
#38222=CARTESIAN_POINT('Ctrl Pts',(55.46886680063,4.44235932371993,5.7107457318557));
#38223=CARTESIAN_POINT('Ctrl Pts',(55.5681226028508,1.16954652307012,7.11894328564385));
#38224=CARTESIAN_POINT('Ctrl Pts',(55.7004636724791,-3.58626632753348,6.75096639668209));
#38225=CARTESIAN_POINT('Ctrl Pts',(55.8658900095141,-7.96704607330977,1.92620451208082));
#38226=CARTESIAN_POINT('Ctrl Pts',(56.0644016139562,-5.93055615333192,-5.65767003333709));
#38227=CARTESIAN_POINT('Ctrl Pts',(56.2629132183984,1.53445226909902,-8.05147084251073));
#38228=CARTESIAN_POINT('Ctrl Pts',(56.4614248228403,7.60149909607939,-3.06615368970725));
#38229=CARTESIAN_POINT('Ctrl Pts',(56.6268511598756,6.84344825826143,3.40647462894263));
#38230=CARTESIAN_POINT('Ctrl Pts',(56.7591922295035,3.18850283536113,6.47152549579565));
#38231=CARTESIAN_POINT('Ctrl Pts',(56.8584480317247,-0.292911935040842,
7.22920298326586));
#38232=CARTESIAN_POINT('Ctrl Pts',(56.9577038339457,-3.70161624816119,6.19235251945399));
#38233=CARTESIAN_POINT('Ctrl Pts',(57.0900449035739,-7.09660911153827,2.84165314195156));
#38234=CARTESIAN_POINT('Ctrl Pts',(57.2554712406088,-7.32852045398567,-3.67108633950697));
#38235=CARTESIAN_POINT('Ctrl Pts',(57.453982845051,-0.878034732768776,-8.14921968669363));
#38236=CARTESIAN_POINT('Ctrl Pts',(57.652494449493,6.36883778380394,-5.15932474046112));
#38237=CARTESIAN_POINT('Ctrl Pts',(57.8510060539352,7.78509439098304,2.56444775343258));
#38238=CARTESIAN_POINT('Ctrl Pts',(58.0164323909703,3.02833753425322,7.01897608200542));
#38239=CARTESIAN_POINT('Ctrl Pts',(58.1487734605984,-1.74165610026088,7.00098754478702));
#38240=CARTESIAN_POINT('Ctrl Pts',(58.2480292628194,-4.88981326478571,5.33262593948569));
#38241=CARTESIAN_POINT('Ctrl Pts',(58.3472850650406,-6.82415659664868,2.34052970890252));
#38242=CARTESIAN_POINT('Ctrl Pts',(58.4796261346684,-7.25455418979818,-2.41004086446941));
#38243=CARTESIAN_POINT('Ctrl Pts',(58.6450524717038,-3.22804353224311,-7.53417692323086));
#38244=CARTESIAN_POINT('Ctrl Pts',(58.8435640761456,4.5892652922565,-6.79112439668372));
#38245=CARTESIAN_POINT('Ctrl Pts',(59.042075680588,8.19462062093288,0.170056969646981));
#38246=CARTESIAN_POINT('Ctrl Pts',(59.2405872850298,4.29105545732191,6.98361869082136));
#38247=CARTESIAN_POINT('Ctrl Pts',(59.4060136220652,-2.21734258458696,7.31575323009928));
#38248=CARTESIAN_POINT('Ctrl Pts',(59.5383546916931,-5.84906661858366,4.22322297128738));
#38249=CARTESIAN_POINT('Ctrl Pts',(59.6376104939143,-7.17679467182627,0.916946788748299));
#38250=CARTESIAN_POINT('Ctrl Pts',(59.7368662961352,-6.72300425491146,-2.61694599911454));
#38251=CARTESIAN_POINT('Ctrl Pts',(59.8692073657634,-3.98548920736035,-6.52324529963));
#38252=CARTESIAN_POINT('Ctrl Pts',(60.0346337027983,2.39734275979888,-7.83816526035532));
#38253=CARTESIAN_POINT('Ctrl Pts',(60.2331453072407,7.88862254419044,-2.22494063948536));
#38254=CARTESIAN_POINT('Ctrl Pts',(60.4316569116826,6.14931137206838,5.41910473632808));
#38255=CARTESIAN_POINT('Ctrl Pts',(60.6301685161249,-1.23005362269408,8.10376795335961));
#38256=CARTESIAN_POINT('Ctrl Pts',(60.7955948531598,-6.41556270153213,4.1566102395872));
#38257=CARTESIAN_POINT('Ctrl Pts',(60.9279359227879,-7.19341139597279,-0.549568068693677));
#38258=CARTESIAN_POINT('Ctrl Pts',(61.027191725009,-6.07349917136267,-3.93189279996371));
#38259=CARTESIAN_POINT('Ctrl Pts',(61.1264475272301,-3.44594301279078,-6.33819132927032));
#38260=CARTESIAN_POINT('Ctrl Pts',(61.2587885968582,1.16629816615583,-7.55490582659723));
#38261=CARTESIAN_POINT('Ctrl Pts',(61.4242149338931,6.89023799286911,-4.43944899263683));
#38262=CARTESIAN_POINT('Ctrl Pts',(61.6227265383354,7.4614394579179,3.39229239744583));
#38263=CARTESIAN_POINT('Ctrl Pts',(61.8212381427774,1.19910247160641,8.10819830520507));
#38264=CARTESIAN_POINT('Ctrl Pts',(62.0197497472196,-6.17009238055327,5.39574341236128));
#38265=CARTESIAN_POINT('Ctrl Pts',(62.1851760842547,-7.58310755601865,-0.966091742530031));
#38266=CARTESIAN_POINT('Ctrl Pts',(62.3175171538827,-5.13962962005787,-5.06274628462288));
#38267=CARTESIAN_POINT('Ctrl Pts',(62.4167729561038,-2.10111727091473,-6.9233286350435));
#38268=CARTESIAN_POINT('Ctrl Pts',(62.5160287583248,1.45896207258534,-7.06531119233941));
#38269=CARTESIAN_POINT('Ctrl Pts',(62.648369827953,5.76713293188694,-5.01767189113402));
#38270=CARTESIAN_POINT('Ctrl Pts',(62.813796164988,8.12822406069122,1.05643768192989));
#38271=CARTESIAN_POINT('Ctrl Pts',(63.0123077694301,3.5095148891804,7.40702583609401));
#38272=CARTESIAN_POINT('Ctrl Pts',(63.2108193738722,-4.31755560360744,6.96702519757902));
#38273=CARTESIAN_POINT('Ctrl Pts',(63.4093309783143,-8.19541465682279,0.138800429881101));
#38274=CARTESIAN_POINT('Ctrl Pts',(63.5747573153495,-5.16843561179771,-5.6324174905481));
#38275=CARTESIAN_POINT('Ctrl Pts',(63.7070983849775,-0.657916098734519,
-7.18431200469918));
#38276=CARTESIAN_POINT('Ctrl Pts',(63.8063541871985,2.86382045553496,-6.64422347407206));
#38277=CARTESIAN_POINT('Ctrl Pts',(63.9056099894197,5.67466178846288,-4.45481830834851));
#38278=CARTESIAN_POINT('Ctrl Pts',(64.0379510590476,7.64360696339799,-0.110118346455386));
#38279=CARTESIAN_POINT('Ctrl Pts',(64.2033773960828,5.52648339923105,6.0532692154428));
#38280=CARTESIAN_POINT('Ctrl Pts',(64.4018890005249,-2.10028451496734,7.92272247716148));
#38281=CARTESIAN_POINT('Ctrl Pts',(64.600400604967,-7.79462501436703,2.53466908675698));
#38282=CARTESIAN_POINT('Ctrl Pts',(64.7989122094091,-6.34926974906822,-5.18371108475186));
#38283=CARTESIAN_POINT('Ctrl Pts',(64.9643385464442,-0.312224135817155,
-7.63802131118276));
#38284=CARTESIAN_POINT('Ctrl Pts',(65.0966796160723,4.13459323863624,-5.9120496720641));
#38285=CARTESIAN_POINT('Ctrl Pts',(65.1959354182933,6.47590571766751,-3.22642500465688));
#38286=CARTESIAN_POINT('Ctrl Pts',(65.2951912205144,7.20968361135704,0.260105359630372));
#38287=CARTESIAN_POINT('Ctrl Pts',(65.4275322901425,5.90928462087591,4.8494544776534));
#38288=CARTESIAN_POINT('Ctrl Pts',(65.5929586271776,0.314063471532927,8.19057086476803));
#38289=CARTESIAN_POINT('Ctrl Pts',(65.7914702316197,-6.71792148235531,4.69577016617119));
#38290=CARTESIAN_POINT('Ctrl Pts',(65.9899818360618,-7.58955798424059,-3.09505025768462));
#38291=CARTESIAN_POINT('Ctrl Pts',(66.1884934405039,-1.50376599212421,-8.05746702061639));
#38292=CARTESIAN_POINT('Ctrl Pts',(66.353919777539,4.69148024327508,-6.03546738918793));
#38293=CARTESIAN_POINT('Ctrl Pts',(66.486260847167,6.97394428949912,-1.84696876138537));
#38294=CARTESIAN_POINT('Ctrl Pts',(66.5855166493881,7.02881002188407,1.71551824848117));
#38295=CARTESIAN_POINT('Ctrl Pts',(66.6847724516092,5.33889197633087,4.85215674409092));
#38296=CARTESIAN_POINT('Ctrl Pts',(66.8171135212373,1.38344990231137,7.51817262669399));
#38297=CARTESIAN_POINT('Ctrl Pts',(66.9825398582723,-5.04671826279436,6.45869353721455));
#38298=CARTESIAN_POINT('Ctrl Pts',(67.1810514627146,-8.16205060168547,-0.749437259000661));
#38299=CARTESIAN_POINT('Ctrl Pts',(67.3795630671564,-3.79922704754698,-7.26268541304556));
#38300=CARTESIAN_POINT('Ctrl Pts',(67.5780746715988,4.05210832491136,-7.12492161511161));
#38301=CARTESIAN_POINT('Ctrl Pts',(67.7435010086337,7.47895595825633,-1.58179277372035));
#38302=CARTESIAN_POINT('Ctrl Pts',(67.8758420782618,6.5188439801296,3.09060926131331));
#38303=CARTESIAN_POINT('Ctrl Pts',(67.9750978804829,4.26134412521868,5.8470613439865));
#38304=CARTESIAN_POINT('Ctrl Pts',(68.074353682704,0.946038930223685,7.15207529371878));
#38305=CARTESIAN_POINT('Ctrl Pts',(68.206694752332,-3.7959202569988,6.6353524066251));
#38306=CARTESIAN_POINT('Ctrl Pts',(68.3721210893672,-8.02345580532069,1.67575897078913));
#38307=CARTESIAN_POINT('Ctrl Pts',(68.5706326938091,-5.75047892022695,-5.8406027897517));
#38308=CARTESIAN_POINT('Ctrl Pts',(68.7691442982514,1.78584702629977,-7.99949146132116));
#38309=CARTESIAN_POINT('Ctrl Pts',(68.9676559026935,7.69377017617253,-2.82656025581714));
#38310=CARTESIAN_POINT('Ctrl Pts',(69.1330822397285,6.73344991610245,3.61903513164787));
#38311=CARTESIAN_POINT('Ctrl Pts',(69.2654233093567,2.98423080922018,6.56830815330687));
#38312=CARTESIAN_POINT('Ctrl Pts',(69.3646791115776,-0.51905136839031,7.21625210960086));
#38313=CARTESIAN_POINT('Ctrl Pts',(69.4639349137988,-3.89391146946297,6.07382587552981));
#38314=CARTESIAN_POINT('Ctrl Pts',(69.5962759834268,-7.18170028038283,2.6170969569783));
#38315=CARTESIAN_POINT('Ctrl Pts',(69.7617023204619,-7.21081252221904,-3.89689416412441));
#38316=CARTESIAN_POINT('Ctrl Pts',(69.960213924904,-0.620995053939498,-8.17585747700275));
#38317=CARTESIAN_POINT('Ctrl Pts',(70.1587255293462,6.52470125732709,-4.9516117227233));
#38318=CARTESIAN_POINT('Ctrl Pts',(70.3572371337882,7.70593355233525,2.79598253320879));
#38319=CARTESIAN_POINT('Ctrl Pts',(70.5557487382304,1.81768565186861,7.99406615824949));
#38320=CARTESIAN_POINT('Ctrl Pts',(70.7211750752654,-4.45822679105659,6.2121217551084));
#38321=CARTESIAN_POINT('Ctrl Pts',(70.8535161448936,-6.88881467085553,2.11853700674387));
#38322=CARTESIAN_POINT('Ctrl Pts',(70.9858572145215,-7.17723399063616,-2.63013344355206));
#38323=CARTESIAN_POINT('Ctrl Pts',(71.1512835515568,-2.99445485884597,-7.63635188476723));
#38324=CARTESIAN_POINT('Ctrl Pts',(71.3497951559987,4.80978360231764,-6.63921429906795));
#38325=CARTESIAN_POINT('Ctrl Pts',(71.515221493034,7.60411813277866,-0.758311536326274));
#38326=CARTESIAN_POINT('Ctrl Pts',(71.6475625626619,6.14450154704762,3.78291426296633));
#38327=CARTESIAN_POINT('Ctrl Pts',(71.7468183648831,3.59819571462861,6.27635644400727));
#38328=CARTESIAN_POINT('Ctrl Pts',(71.8460741671041,0.161404155566158,7.21267391002245));
#38329=CARTESIAN_POINT('Ctrl Pts',(71.9784152367322,-4.49653865790636,6.18215858561921));
#38330=CARTESIAN_POINT('Ctrl Pts',(72.1438415737672,-8.15815741081568,0.791574195716444));
#38331=CARTESIAN_POINT('Ctrl Pts',(72.3423531782093,-5.07989086167079,-6.43244417407182));
#38332=CARTESIAN_POINT('Ctrl Pts',(72.5408647826515,2.64687881754866,-7.75723974463881));
#38333=CARTESIAN_POINT('Ctrl Pts',(72.7393763870936,7.95595254297234,-1.97144739296824));
#38334=CARTESIAN_POINT('Ctrl Pts',(72.9048027241286,6.29898760469208,4.33125433189542));
#38335=CARTESIAN_POINT('Ctrl Pts',(73.0371437937569,2.25081894201211,6.85426618338362));
#38336=CARTESIAN_POINT('Ctrl Pts',(73.1363995959777,-1.30238688003595,7.11694925165258));
#38337=CARTESIAN_POINT('Ctrl Pts',(73.235655398199,-4.53230734834526,5.61296614737723));
#38338=CARTESIAN_POINT('Ctrl Pts',(73.3679964678268,-7.4246188108322,1.81985648838285));
#38339=CARTESIAN_POINT('Ctrl Pts',(73.5334228048621,-6.74221461261432,-4.66118406180153));
#38340=CARTESIAN_POINT('Ctrl Pts',(73.731934409304,0.27181873891023,-8.19187645961583));
#38341=CARTESIAN_POINT('Ctrl Pts',(73.9304460137463,7.02858186584606,-4.21660550406958));
#38342=CARTESIAN_POINT('Ctrl Pts',(74.1289576181883,7.34926068645952,3.62938777901172));
#38343=CARTESIAN_POINT('Ctrl Pts',(74.2943839552235,2.01557258935635,7.3738945111119));
#38344=CARTESIAN_POINT('Ctrl Pts',(74.4267250248515,-2.70489894858274,6.68810243885279));
#38345=CARTESIAN_POINT('Ctrl Pts',(74.5259808270726,-5.5884003905664,4.59531874068335));
#38346=CARTESIAN_POINT('Ctrl Pts',(74.6252366292936,-7.08467546628861,1.36182453082842));
#38347=CARTESIAN_POINT('Ctrl Pts',(74.7575776989218,-6.84557113769722,-3.40220653545019));
#38348=CARTESIAN_POINT('Ctrl Pts',(74.9230040359568,-2.14116300119577,-7.91198508227128));
#38349=CARTESIAN_POINT('Ctrl Pts',(75.1215156403989,5.49505931408899,-6.08153349264663));
#38350=CARTESIAN_POINT('Ctrl Pts',(75.3200272448411,8.0900573333749,1.31594028931691));
#38351=CARTESIAN_POINT('Ctrl Pts',(75.5185388492831,3.27079925713886,7.51571414921572));
#38352=CARTESIAN_POINT('Ctrl Pts',(75.6839651863183,-3.21997727761606,6.93315222625922));
#38353=CARTESIAN_POINT('Ctrl Pts',(75.8163062559462,-6.38284268877731,3.36251569288139));
#38354=CARTESIAN_POINT('Ctrl Pts',(75.9155620581674,-7.23448285468373,-0.097113334340778));
#38355=CARTESIAN_POINT('Ctrl Pts',(76.0148178603884,-6.29028443025259,-3.53263561107129));
#38356=CARTESIAN_POINT('Ctrl Pts',(76.1471589300166,-3.03271383316493,-7.01708630894154));
#38357=CARTESIAN_POINT('Ctrl Pts',(76.3125852670515,3.47136133651406,-7.42520958814913));
#38358=CARTESIAN_POINT('Ctrl Pts',(76.5110968714938,8.12246542232142,-1.09830868028507));
#38359=CARTESIAN_POINT('Ctrl Pts',(76.7096084759357,5.32983568543061,6.22684334636948));
#38360=CARTESIAN_POINT('Ctrl Pts',(76.908120080378,-2.35276902473004,7.85166000746804));
#38361=CARTESIAN_POINT('Ctrl Pts',(77.073546417413,-6.93442826554184,3.21722832437996));
#38362=CARTESIAN_POINT('Ctrl Pts',(77.2058874870412,-7.0455678962576,-1.5515043000454));
#38363=CARTESIAN_POINT('Ctrl Pts',(77.3051432892621,-5.46303685210097,-4.74366962672763));
#38364=CARTESIAN_POINT('Ctrl Pts',(77.4043990914832,-2.52439886881471,-6.75829881885711));
#38365=CARTESIAN_POINT('Ctrl Pts',(77.5367401611113,2.21278020170318,-7.31713449651446));
#38366=CARTESIAN_POINT('Ctrl Pts',(77.7021664981463,7.44403436148341,-3.43080739501002));
#38367=CARTESIAN_POINT('Ctrl Pts',(77.9006781025885,6.91286514831034,4.40375089386527));
#38368=CARTESIAN_POINT('Ctrl Pts',(78.0991897070305,0.0518300311409729,
8.19622108912486));
#38369=CARTESIAN_POINT('Ctrl Pts',(78.2977013114727,-6.86490262637786,4.47852641914182));
#38370=CARTESIAN_POINT('Ctrl Pts',(78.4631276485078,-7.37309485507158,-2.01849590518484));
#38371=CARTESIAN_POINT('Ctrl Pts',(78.5954687181359,-4.38000697731177,-5.73260250257588));
#38372=CARTESIAN_POINT('Ctrl Pts',(78.694724520357,-1.11088337052448,-7.14934341824773));
#38373=CARTESIAN_POINT('Ctrl Pts',(78.793980322578,2.43399833347421,-6.79138017537552));
#38374=CARTESIAN_POINT('Ctrl Pts',(78.9263213922061,6.4129694783647,-4.16061004309389));
#38375=CARTESIAN_POINT('Ctrl Pts',(79.091747729241,7.90018797235732,2.18428866178938));
#38376=CARTESIAN_POINT('Ctrl Pts',(79.2902593336834,2.43766676976039,7.82550363960998));
#38377=CARTESIAN_POINT('Ctrl Pts',(79.4887709381253,-5.25065983451864,6.2937506938324));
#38378=CARTESIAN_POINT('Ctrl Pts',(79.6872825425675,-8.13409534553851,-1.01023752963825));
#38379=CARTESIAN_POINT('Ctrl Pts',(79.8527088796026,-4.3287534491085,-6.30069417111822));
#38380=CARTESIAN_POINT('Ctrl Pts',(79.9850499492307,0.354644279160853,-7.20565194892855));
#38381=CARTESIAN_POINT('Ctrl Pts',(80.0843057514517,3.76604508515065,-6.17770811802905));
#38382=CARTESIAN_POINT('Ctrl Pts',(80.1835615536727,6.24258859266155,-3.61625223630912));
#38383=CARTESIAN_POINT('Ctrl Pts',(80.3159026233008,7.583708516415,0.961362886316208));
#38384=CARTESIAN_POINT('Ctrl Pts',(80.4813289603358,4.62433780266202,6.76753920147287));
#38385=CARTESIAN_POINT('Ctrl Pts',(80.6798405647781,-3.18907150028927,7.55053305800232));
#38386=CARTESIAN_POINT('Ctrl Pts',(80.8783521692201,-8.07276791414114,1.41814833439819));
#38387=CARTESIAN_POINT('Ctrl Pts',(81.0768637736623,-5.56078777391149,-6.02177102604519));
#38388=CARTESIAN_POINT('Ctrl Pts',(81.2422901106974,0.760466419715527,-7.60648041380617));
#38389=CARTESIAN_POINT('Ctrl Pts',(81.3746311803254,4.92176359902424,-5.27479247451109));
#38390=CARTESIAN_POINT('Ctrl Pts',(81.4738869825466,6.86391530262252,-2.28775870523392));
#38391=CARTESIAN_POINT('Ctrl Pts',(81.5731427847675,7.10221557276389,1.26717265273106));
#38392=CARTESIAN_POINT('Ctrl Pts',(81.7054838543957,5.17194686549097,5.62919346635642));
#38393=CARTESIAN_POINT('Ctrl Pts',(81.8709101914307,-0.836023194187075,
8.15384278579016));
#38394=CARTESIAN_POINT('Ctrl Pts',(82.0694217958728,-7.30931056586058,3.70873368493102));
#38395=CARTESIAN_POINT('Ctrl Pts',(82.267933400315,-7.08134643210635,-4.12737921718344));
#38396=CARTESIAN_POINT('Ctrl Pts',(82.466445004757,-0.360595744877148,-8.18865420355369));
#38397=CARTESIAN_POINT('Ctrl Pts',(82.6318713417921,5.49044628522498,-5.31900865295313));
#38398=CARTESIAN_POINT('Ctrl Pts',(82.7642124114202,7.16386984035125,-0.852151092438711));
#38399=CARTESIAN_POINT('Ctrl Pts',(82.8634682136414,6.71931104372443,2.68291488359821));
#38400=CARTESIAN_POINT('Ctrl Pts',(82.9627240158622,4.60679638678563,5.55199240134011));
#38401=CARTESIAN_POINT('Ctrl Pts',(83.0950650854905,0.316986986568839,7.6378251296738));
#38402=CARTESIAN_POINT('Ctrl Pts',(83.2604914225255,-5.90145159800573,5.68831750107152));
#38403=CARTESIAN_POINT('Ctrl Pts',(83.4590030269676,-7.97667297070005,-1.88505034745662));
#38404=CARTESIAN_POINT('Ctrl Pts',(83.6575146314097,-2.74473724711928,-7.72315634557654));
#38405=CARTESIAN_POINT('Ctrl Pts',(83.8560262358518,5.00993965925736,-6.48726379664039));
#38406=CARTESIAN_POINT('Ctrl Pts',(84.021452572887,7.62677061175643,-0.518867513705835));
#38407=CARTESIAN_POINT('Ctrl Pts',(84.1537936425149,6.02180479091357,3.97304160989659));
#38408=CARTESIAN_POINT('Ctrl Pts',(84.2530494447361,3.40054253636251,6.38619476944906));
#38409=CARTESIAN_POINT('Ctrl Pts',(84.3523052469571,-0.0648471614422156,
7.2140825764259));
#38410=CARTESIAN_POINT('Ctrl Pts',(84.4846463165851,-4.68771573852409,6.03839172428596));
#38411=CARTESIAN_POINT('Ctrl Pts',(84.6500726536203,-8.17906789511689,0.53566344253681));
#38412=CARTESIAN_POINT('Ctrl Pts',(84.8485842580624,-4.87590051758694,-6.58834733727196));
#38413=CARTESIAN_POINT('Ctrl Pts',(85.0470958625044,2.88847017309471,-7.67055842511386));
#38414=CARTESIAN_POINT('Ctrl Pts',(85.2456074669467,8.01380811645443,-1.7213269385129));
#38415=CARTESIAN_POINT('Ctrl Pts',(85.4110338039818,6.16025196085469,4.52638368235799));
#38416=CARTESIAN_POINT('Ctrl Pts',(85.5433748736097,2.03507347224601,6.92139209526522));
#38417=CARTESIAN_POINT('Ctrl Pts',(85.6426306758309,-1.52462288789535,7.07267263661027));
#38418=CARTESIAN_POINT('Ctrl Pts',(85.7418864780518,-4.70585728012308,5.46828125035202));
#38419=CARTESIAN_POINT('Ctrl Pts',(85.8742275476801,-7.47796826070822,1.58645647686012));
#38420=CARTESIAN_POINT('Ctrl Pts',(86.039653884715,-6.59293912528612,-4.87003497388596));
#38421=CARTESIAN_POINT('Ctrl Pts',(86.2381654891572,0.528219555732677,-8.17934658728218));
#38422=CARTESIAN_POINT('Ctrl Pts',(86.4366770935992,7.15718074288302,-3.9944324137038));
#38423=CARTESIAN_POINT('Ctrl Pts',(86.6351886980415,7.23199928445137,3.85775495674566));
#38424=CARTESIAN_POINT('Ctrl Pts',(86.8006150350765,1.78366538655549,7.43339701952848));
#38425=CARTESIAN_POINT('Ctrl Pts',(86.9329561047045,-2.9130149582689,6.60011639493883));
#38426=CARTESIAN_POINT('Ctrl Pts',(87.0322119069257,-5.72956514765639,4.41806025238579));
#38427=CARTESIAN_POINT('Ctrl Pts',(87.1314677091467,-7.12384723501912,1.13929502147146));
#38428=CARTESIAN_POINT('Ctrl Pts',(87.2638087787747,-6.73567118817512,-3.61491177014297));
#38429=CARTESIAN_POINT('Ctrl Pts',(87.4292351158099,-1.89234348115796,-7.97515661952291));
#38430=CARTESIAN_POINT('Ctrl Pts',(87.6277467202519,5.68281172087316,-5.90646911775986));
#38431=CARTESIAN_POINT('Ctrl Pts',(87.8262583246941,8.04487991343423,1.56864070850067));
#38432=CARTESIAN_POINT('Ctrl Pts',(88.0247699291362,3.03383520051197,7.61445539304916));
#38433=CARTESIAN_POINT('Ctrl Pts',(88.1901962661713,-3.43551455250795,6.8289159623353));
#38434=CARTESIAN_POINT('Ctrl Pts',(88.3225373357993,-6.48501172170561,3.160983319029));
#38435=CARTESIAN_POINT('Ctrl Pts',(88.4217931380204,-7.22789348039601,-0.323618619671762));
#38436=CARTESIAN_POINT('Ctrl Pts',(88.5210489402415,-6.17657234984887,-3.72788768351753));
#38437=CARTESIAN_POINT('Ctrl Pts',(88.6533900098695,-2.81148142816453,-7.108616295751));
#38438=CARTESIAN_POINT('Ctrl Pts',(88.8188163469046,3.702184440345,-7.31285972286276));
#38439=CARTESIAN_POINT('Ctrl Pts',(89.0173279513468,8.15287601138966,-0.843409293789282));
#38440=CARTESIAN_POINT('Ctrl Pts',(89.2158395557888,5.13222365494829,6.39069689858097));
#38441=CARTESIAN_POINT('Ctrl Pts',(89.414351160231,-2.59749534447238,7.77413049106106));
#38442=CARTESIAN_POINT('Ctrl Pts',(89.5797774972659,-7.03177699352893,2.99849391768735));
#38443=CARTESIAN_POINT('Ctrl Pts',(89.7121185668942,-6.99352590129428,-1.77138026458615));
#38444=CARTESIAN_POINT('Ctrl Pts',(89.811374369115,-5.31180611963898,-4.91242189986933));
#38445=CARTESIAN_POINT('Ctrl Pts',(89.9106301713363,-2.31151988251846,-6.83403748940264));
#38446=CARTESIAN_POINT('Ctrl Pts',(90.0429712409643,2.44083613787073,-7.24425099021252));
#38447=CARTESIAN_POINT('Ctrl Pts',(90.2083975779994,7.54782152835416,-3.19600956392727));
#38448=CARTESIAN_POINT('Ctrl Pts',(90.4069091824415,6.77156813158818,4.61807227457544));
#38449=CARTESIAN_POINT('Ctrl Pts',(90.6054207868836,-0.204865813229847,
8.19382428982425));
#38450=CARTESIAN_POINT('Ctrl Pts',(90.8039323913256,-7.0017838900133,4.26135064435577));
#38451=CARTESIAN_POINT('Ctrl Pts',(90.969358728361,-7.30626805192062,-2.24839956738446));
#38452=CARTESIAN_POINT('Ctrl Pts',(91.1016997979887,-4.19833829625926,-5.86695390505177));
#38453=CARTESIAN_POINT('Ctrl Pts',(91.2009556002101,-0.886451816183042,
-7.18062506697956));
#38454=CARTESIAN_POINT('Ctrl Pts',(91.300211402431,2.64548140559999,-6.71182692763033));
#38455=CARTESIAN_POINT('Ctrl Pts',(91.4325524720591,6.54011662097128,-3.95774279675006));
#38456=CARTESIAN_POINT('Ctrl Pts',(91.5979788090942,7.82791073605462,2.43061730121419));
#38457=CARTESIAN_POINT('Ctrl Pts',(91.7964904135364,2.19141005279209,7.89800281555184));
#38458=CARTESIAN_POINT('Ctrl Pts',(91.9950020179783,-5.4451778386233,6.12623577735211));
#38459=CARTESIAN_POINT('Ctrl Pts',(92.1935136224206,-8.09846962411599,-1.26446696432582));
#38460=CARTESIAN_POINT('Ctrl Pts',(92.3589399594556,-4.12931971582869,-6.43316190885945));
#38461=CARTESIAN_POINT('Ctrl Pts',(92.4912810290837,0.580120396574044,-7.19101195238317));
#38462=CARTESIAN_POINT('Ctrl Pts',(92.5905368313047,3.95765727397703,-6.05674186974201));
#38463=CARTESIAN_POINT('Ctrl Pts',(92.6897926335259,6.35277235243675,-3.41898757119045));
#38464=CARTESIAN_POINT('Ctrl Pts',(92.8221337031538,7.54988327981452,1.19838054152583));
#38465=CARTESIAN_POINT('Ctrl Pts',(92.987560040189,4.41013951775851,6.9090344036273));
#38466=CARTESIAN_POINT('Ctrl Pts',(93.1860716446311,-3.42395764764996,7.44696183158223));
#38467=CARTESIAN_POINT('Ctrl Pts',(93.3845832490732,-8.11321888126058,1.16464839273495));
#38468=CARTESIAN_POINT('Ctrl Pts',(93.5830948535153,-5.36948445522538,-6.19295758436106));
#38469=CARTESIAN_POINT('Ctrl Pts',(93.7485211905504,0.998295723954193,-7.57893522261972));
#38470=CARTESIAN_POINT('Ctrl Pts',(93.8808622601784,5.08453351976072,-5.11807692988962));
#38471=CARTESIAN_POINT('Ctrl Pts',(93.9801180623996,6.93219161979444,-2.07168832631786));
#38472=CARTESIAN_POINT('Ctrl Pts',(94.0793738646205,7.05904983992973,1.48896203149283));
#38473=CARTESIAN_POINT('Ctrl Pts',(94.2117149342488,4.99312809870757,5.78839574070638));
#38474=CARTESIAN_POINT('Ctrl Pts',(94.3771412712837,-1.09095647846726,8.12366302345754));
#38475=CARTESIAN_POINT('Ctrl Pts',(94.5756528757259,-7.42186726605041,3.47801851333087));
#38476=CARTESIAN_POINT('Ctrl Pts',(94.7741644801679,-6.94862155587487,-4.34711225610455));
#38477=CARTESIAN_POINT('Ctrl Pts',(94.9726760846102,-0.103985426572741,
-8.19593033082037));
#38478=CARTESIAN_POINT('Ctrl Pts',(95.1381024216451,5.65432195232088,-5.14446272419511));
#38479=CARTESIAN_POINT('Ctrl Pts',(95.2704434912733,7.18704198136562,-0.627391530009471));
#38480=CARTESIAN_POINT('Ctrl Pts',(95.3696992934942,6.63199814606807,2.89201897737531));
#38481=CARTESIAN_POINT('Ctrl Pts',(95.4689550957155,4.43067240756226,5.69353445503804));
#38482=CARTESIAN_POINT('Ctrl Pts',(95.6012961653433,0.0776476560697105,
7.64400577594225));
#38483=CARTESIAN_POINT('Ctrl Pts',(95.7667225023786,-6.07669085085267,5.50071952200477));
#38484=CARTESIAN_POINT('Ctrl Pts',(95.9652341068207,-7.91372907993021,-2.13392093185527));
#38485=CARTESIAN_POINT('Ctrl Pts',(96.1637457112627,-2.50153500276373,-7.805321846272));
#38486=CARTESIAN_POINT('Ctrl Pts',(96.3622573157049,5.21063572505351,-6.32719229179871));
#38487=CARTESIAN_POINT('Ctrl Pts',(96.52768365274,7.63927871038486,-0.279775349507908));
#38488=CARTESIAN_POINT('Ctrl Pts',(96.6600247223681,5.89443276483208,4.1596700535876));
#38489=CARTESIAN_POINT('Ctrl Pts',(96.759280524589,3.1988865391963,6.48955299572309));
#38490=CARTESIAN_POINT('Ctrl Pts',(96.8585363268103,-0.290729422875887,
7.20851364544127));
#38491=CARTESIAN_POINT('Ctrl Pts',(96.9908773964381,-4.87451309683684,5.88863104039446));
#38492=CARTESIAN_POINT('Ctrl Pts',(97.1563037334734,-8.19183109205004,0.279267463058967));
#38493=CARTESIAN_POINT('Ctrl Pts',(97.3548153379154,-4.66719037118441,-6.73780828853616));
#38494=CARTESIAN_POINT('Ctrl Pts',(97.5533269423575,3.12726243117806,-7.57634187325818));
#38495=CARTESIAN_POINT('Ctrl Pts',(97.7518385467997,8.06378225188477,-1.46952466831598));
#38496=CARTESIAN_POINT('Ctrl Pts',(97.9172648838347,6.01548373649835,4.71707630604539));
#38497=CARTESIAN_POINT('Ctrl Pts',(98.0496059534629,1.81732709838692,6.98172720688136));
#38498=CARTESIAN_POINT('Ctrl Pts',(98.1488617556837,-1.74536084060413,7.02145915825447));
#38499=CARTESIAN_POINT('Ctrl Pts',(98.2481175579051,-4.87479233060809,5.31823206594859));
#38500=CARTESIAN_POINT('Ctrl Pts',(98.3804586275328,-7.52398163919293,1.35150055649951));
#38501=CARTESIAN_POINT('Ctrl Pts',(98.5458849645683,-6.43719700480271,-5.07410895408839));
#38502=CARTESIAN_POINT('Ctrl Pts',(98.7443965690101,0.784102473898442,-8.1587934037068));
#38503=CARTESIAN_POINT('Ctrl Pts',(98.9429081734525,7.27875891268348,-3.76834117152016));
#38504=CARTESIAN_POINT('Ctrl Pts',(99.1414197778943,7.10764399270585,4.08233803469939));
#38505=CARTESIAN_POINT('Ctrl Pts',(99.3068461149296,1.55000852346872,7.4856079938977));
#38506=CARTESIAN_POINT('Ctrl Pts',(99.4391871845575,-3.11827353367708,6.50565621155993));
#38507=CARTESIAN_POINT('Ctrl Pts',(99.5384429867787,-5.86510970487799,4.23646802474608));
#38508=CARTESIAN_POINT('Ctrl Pts',(99.6376987889998,-7.15603111934792,0.915647963337127));
#38509=CARTESIAN_POINT('Ctrl Pts',(99.7700398586277,-6.61916412903343,-3.82407108904214));
#38510=CARTESIAN_POINT('Ctrl Pts',(99.935466195663,-1.64166773351012,-8.03050521507537));
#38511=CARTESIAN_POINT('Ctrl Pts',(100.133977800105,5.86498977835619,-5.72561100614777));
#38512=CARTESIAN_POINT('Ctrl Pts',(100.332489404547,7.9918111603258,1.81980242653843));
#38513=CARTESIAN_POINT('Ctrl Pts',(100.531001008989,2.7938952127985,7.70572751247425));
#38514=CARTESIAN_POINT('Ctrl Pts',(100.696427346024,-3.64768188364758,6.71798112060759));
#38515=CARTESIAN_POINT('Ctrl Pts',(100.828768415652,-6.58081951726305,2.95635029302163));
#38516=CARTESIAN_POINT('Ctrl Pts',(100.928024217873,-7.21421416567094,-0.549806463023575));
#38517=CARTESIAN_POINT('Ctrl Pts',(101.027280020094,-6.05680158445754,-3.91948301952586));
#38518=CARTESIAN_POINT('Ctrl Pts',(101.159621089723,-2.58749120224389,-7.19317334279116));
#38519=CARTESIAN_POINT('Ctrl Pts',(101.325047426758,3.92937602039146,-7.19333657261869));
#38520=CARTESIAN_POINT('Ctrl Pts',(101.5235590312,8.17528933193856,-0.587682595483952));
#38521=CARTESIAN_POINT('Ctrl Pts',(101.722070635642,4.92957735549824,6.54828172806438));
#38522=CARTESIAN_POINT('Ctrl Pts',(101.920582240084,-2.83967374520597,7.68897522283621));
#38523=CARTESIAN_POINT('Ctrl Pts',(102.086008577119,-7.12222815448253,2.77681824695588));
#38524=CARTESIAN_POINT('Ctrl Pts',(102.218349646747,-6.93462386032044,-1.98951865779466));
#38525=CARTESIAN_POINT('Ctrl Pts',(102.317605448968,-5.15536496329487,-5.07635551061814));
#38526=CARTESIAN_POINT('Ctrl Pts',(102.416861251189,-2.09637349448938,-6.90307255832048));
#38527=CARTESIAN_POINT('Ctrl Pts',(102.549202320817,2.66649782420712,-7.16426149820347));
#38528=CARTESIAN_POINT('Ctrl Pts',(102.714628657852,7.64420493298944,-2.9580767229826));
#38529=CARTESIAN_POINT('Ctrl Pts',(102.913140262295,6.62362879029324,4.82786372449762));
#38530=CARTESIAN_POINT('Ctrl Pts',(103.111651866737,-0.461360701899278,
8.18339005527401));
#38531=CARTESIAN_POINT('Ctrl Pts',(103.310163471179,-7.13179700726309,4.03999485194223));
#38532=CARTESIAN_POINT('Ctrl Pts',(103.475589808214,-7.23227442967135,-2.47609774342373));
#38533=CARTESIAN_POINT('Ctrl Pts',(103.607930877842,-4.01255140726822,-5.99555033154707));
#38534=CARTESIAN_POINT('Ctrl Pts',(103.707186680063,-0.661150729031283,
-7.20486314150311));
#38535=CARTESIAN_POINT('Ctrl Pts',(103.806442482284,2.85436948853256,-6.6256899563683));
#38536=CARTESIAN_POINT('Ctrl Pts',(103.938783551912,6.66084847297623,-3.75099334572874));
#38537=CARTESIAN_POINT('Ctrl Pts',(104.104209888947,7.74795499416537,2.67456171423117));
#38538=CARTESIAN_POINT('Ctrl Pts',(104.302721493389,1.9430037514535,7.96275473222629));
#38539=CARTESIAN_POINT('Ctrl Pts',(104.501233097831,-5.63435459263867,5.95271155055995));
#38540=CARTESIAN_POINT('Ctrl Pts',(104.699744702274,-8.0549000022414,-1.51745606366842));
#38541=CARTESIAN_POINT('Ctrl Pts',(104.865171039309,-3.9258354757219,-6.55931927333122));
#38542=CARTESIAN_POINT('Ctrl Pts',(104.997512108937,0.805027465655755,-7.16931818748407));
#38543=CARTESIAN_POINT('Ctrl Pts',(105.096767911158,4.14538734270979,-5.92983449194886));
#38544=CARTESIAN_POINT('Ctrl Pts',(105.196023713379,6.45672458925401,-3.21836915162517));
#38545=CARTESIAN_POINT('Ctrl Pts',(105.328364783007,7.50865226061103,1.43422264037047));
#38546=CARTESIAN_POINT('Ctrl Pts',(105.493791120042,4.19161526203335,7.0437525372525));
#38547=CARTESIAN_POINT('Ctrl Pts',(105.692302724484,-3.65548518083639,7.33608561355083));
#38548=CARTESIAN_POINT('Ctrl Pts',(105.890814328926,-8.14571149277621,0.910006333379135));
#38549=CARTESIAN_POINT('Ctrl Pts',(106.089325933368,-5.17291411014704,-6.35806998076943));
#38550=CARTESIAN_POINT('Ctrl Pts',(106.254752270403,1.23514574214642,-7.54395470249355));
#38551=CARTESIAN_POINT('Ctrl Pts',(106.387093340031,5.24231601294789,-4.95634245627861));
#38552=CARTESIAN_POINT('Ctrl Pts',(106.486349142253,6.99366792025834,-1.8535826036882));
#38553=CARTESIAN_POINT('Ctrl Pts',(106.585604944474,7.00896003570272,1.70928496788058));
#38554=CARTESIAN_POINT('Ctrl Pts',(106.717946014102,4.80941096796698,5.94193284353501));
#38555=CARTESIAN_POINT('Ctrl Pts',(106.883372351137,-1.34481853620912,8.08548866178312));
#38556=CARTESIAN_POINT('Ctrl Pts',(107.081883955579,-7.52714557143349,3.24393493693221));
#38557=CARTESIAN_POINT('Ctrl Pts',(107.280395560021,-6.80907733581119,-4.56266073535736));
#38558=CARTESIAN_POINT('Ctrl Pts',(107.478907164463,0.152720294781448,-8.19500999416272));
#38559=CARTESIAN_POINT('Ctrl Pts',(107.644333501498,5.81266281373758,-4.96514640636761));
#38560=CARTESIAN_POINT('Ctrl Pts',(107.776674571126,7.2031480419312,-0.401630923051306));
#38561=CARTESIAN_POINT('Ctrl Pts',(107.875930373347,6.53821527098569,3.09744391522371));
#38562=CARTESIAN_POINT('Ctrl Pts',(107.975186175568,4.25013664469689,5.83104671267199));
#38563=CARTESIAN_POINT('Ctrl Pts',(108.107527245197,-0.161622961106447,
7.63932412864128));
#38564=CARTESIAN_POINT('Ctrl Pts',(108.272953582232,-6.24629954731418,5.3146339055588));
#38565=CARTESIAN_POINT('Ctrl Pts',(108.471465186674,-7.84228358717403,-2.39245798963491));
#38566=CARTESIAN_POINT('Ctrl Pts',(108.636891523709,-3.18936293666094,-6.9454835370673));
#38567=CARTESIAN_POINT('Ctrl Pts',(108.769232593337,1.58468972940029,-7.03937783508502));
#38568=CARTESIAN_POINT('Ctrl Pts',(108.868488395558,4.75883494996184,-5.44436182139488));
#38569=CARTESIAN_POINT('Ctrl Pts',(108.967744197779,6.7844801612218,-2.49148592609996));
#38570=CARTESIAN_POINT('Ctrl Pts',(109.033914732593,7.02701963797669,-0.129888228207554));
#38571=CARTESIAN_POINT('Ctrl Pts',(109.067,6.85892174064777,1.01078264511681));
#38572=CARTESIAN_POINT('Ctrl Pts',(30.7922774969106,-1.81203895677844,6.4452040820594));
#38573=CARTESIAN_POINT('Ctrl Pts',(30.8253627643176,-2.88390664196679,6.14385349992971));
#38574=CARTESIAN_POINT('Ctrl Pts',(30.8915332991317,-4.8703123697955,4.99930801783347));
#38575=CARTESIAN_POINT('Ctrl Pts',(30.9907891013527,-6.67525664671072,2.04974392354754));
#38576=CARTESIAN_POINT('Ctrl Pts',(31.0900449035737,-6.83047548939251,-1.37719959429219));
#38577=CARTESIAN_POINT('Ctrl Pts',(31.2223859732019,-4.8662109885332,-5.54901554722458));
#38578=CARTESIAN_POINT('Ctrl Pts',(31.3878123102369,0.981499149386936,-7.85666683476529));
#38579=CARTESIAN_POINT('Ctrl Pts',(31.5863239146791,7.14710812042464,-3.4122242090372));
#38580=CARTESIAN_POINT('Ctrl Pts',(31.7517502517141,6.79854969246659,2.86822284039177));
#38581=CARTESIAN_POINT('Ctrl Pts',(31.8840913213422,3.46566165096873,6.04498987921042));
#38582=CARTESIAN_POINT('Ctrl Pts',(31.9833471235633,0.153961023470463,6.98483577110846));
#38583=CARTESIAN_POINT('Ctrl Pts',(32.0826029257843,-3.19288929971824,6.19203320852766));
#38584=CARTESIAN_POINT('Ctrl Pts',(32.2149439954124,-6.66809958720304,3.16766408236977));
#38585=CARTESIAN_POINT('Ctrl Pts',(32.3803703324475,-7.28493555493229,-3.09507108051456));
#38586=CARTESIAN_POINT('Ctrl Pts',(32.5788819368896,-1.33895233039623,-7.80108067131974));
#38587=CARTESIAN_POINT('Ctrl Pts',(32.7773935413317,5.82636340729205,-5.35749892731368));
#38588=CARTESIAN_POINT('Ctrl Pts',(32.9759051457738,7.65819530642828,2.00095028754364));
#38589=CARTESIAN_POINT('Ctrl Pts',(33.1413314828089,3.34300536777016,6.58174892634051));
#38590=CARTESIAN_POINT('Ctrl Pts',(33.273672552437,-1.25536816334185,6.85276289884607));
#38591=CARTESIAN_POINT('Ctrl Pts',(33.372928354658,-4.39037706243106,5.43513071151949));
#38592=CARTESIAN_POINT('Ctrl Pts',(33.4721841568791,-6.43556040023512,2.66831418699039));
#38593=CARTESIAN_POINT('Ctrl Pts',(33.6045252265073,-7.13755440619835,-1.88421592210945));
#38594=CARTESIAN_POINT('Ctrl Pts',(33.7699515635422,-3.56661413217037,-7.06621698471055));
#38595=CARTESIAN_POINT('Ctrl Pts',(33.9684631679844,4.01254545034611,-6.82264596434217));
#38596=CARTESIAN_POINT('Ctrl Pts',(34.1669747724265,7.90816875735116,-0.331485828065288));
#38597=CARTESIAN_POINT('Ctrl Pts',(34.3654863768686,4.55785072533662,6.47133294229691));
#38598=CARTESIAN_POINT('Ctrl Pts',(34.5309127139037,-1.69479614673967,7.18488923320334));
#38599=CARTESIAN_POINT('Ctrl Pts',(34.6632537835318,-5.38196425847962,4.42388796338411));
#38600=CARTESIAN_POINT('Ctrl Pts',(34.7625095857528,-6.86148701022481,1.31759840225387));
#38601=CARTESIAN_POINT('Ctrl Pts',(34.8617653879739,-6.63776106705247,-2.11576276551648));
#38602=CARTESIAN_POINT('Ctrl Pts',(34.9941064576019,-4.2355184272481,-6.0461021388265));
#38603=CARTESIAN_POINT('Ctrl Pts',(35.1595327946371,1.83669728137531,-7.6992658814414));
#38604=CARTESIAN_POINT('Ctrl Pts',(35.3580443990791,7.46846773094147,-2.62126076137705));
#38605=CARTESIAN_POINT('Ctrl Pts',(35.5565560035213,6.2542393043315,4.85113481298777));
#38606=CARTESIAN_POINT('Ctrl Pts',(35.7550676079634,-0.695620042101597,
7.88468545833603));
#38607=CARTESIAN_POINT('Ctrl Pts',(35.9204939449985,-5.93197410466557,4.39393338519193));
#38608=CARTESIAN_POINT('Ctrl Pts',(36.0528350146266,-6.96615643498071,-0.0948085558509277));
#38609=CARTESIAN_POINT('Ctrl Pts',(36.1520908168476,-6.09126670585619,-3.42235873639071));
#38610=CARTESIAN_POINT('Ctrl Pts',(36.2513466190687,-3.70432255158069,-5.90036596931892));
#38611=CARTESIAN_POINT('Ctrl Pts',(36.3836876886967,0.667353267230231,-7.35184378166206));
#38612=CARTESIAN_POINT('Ctrl Pts',(36.5491140257318,6.37236282717805,-4.69522566233383));
#38613=CARTESIAN_POINT('Ctrl Pts',(36.7476256301739,7.39632868574868,2.81839319700334));
#38614=CARTESIAN_POINT('Ctrl Pts',(36.9461372346161,1.64584269422835,7.74210695265263));
#38615=CARTESIAN_POINT('Ctrl Pts',(37.1446488390582,-5.62048377641761,5.57335752850344));
#38616=CARTESIAN_POINT('Ctrl Pts',(37.3100751760933,-7.36692134135521,-0.472691573440474));
#38617=CARTESIAN_POINT('Ctrl Pts',(37.4424162457214,-5.25957598656419,-4.56871804551017));
#38618=CARTESIAN_POINT('Ctrl Pts',(37.5416720479423,-2.44356673040902,-6.54561311391665));
#38619=CARTESIAN_POINT('Ctrl Pts',(37.6409278501635,0.979016833964809,-6.89766990922517));
#38620=CARTESIAN_POINT('Ctrl Pts',(37.7732689197915,5.25497107745377,-5.18461631641446));
#38621=CARTESIAN_POINT('Ctrl Pts',(37.9386952568267,7.8977604870432,0.526812405708338));
#38622=CARTESIAN_POINT('Ctrl Pts',(38.1372068612687,3.8302061148084,6.92665426873328));
#38623=CARTESIAN_POINT('Ctrl Pts',(38.3357184657109,-3.74004062557482,6.9757518848886));
#38624=CARTESIAN_POINT('Ctrl Pts',(38.534230070153,-7.89026300224576,0.629207260686155));
#38625=CARTESIAN_POINT('Ctrl Pts',(38.6996564071881,-5.3217769150866,-5.11601972624796));
#38626=CARTESIAN_POINT('Ctrl Pts',(38.8319974768161,-1.06840181276754,-6.88439116438718));
#38627=CARTESIAN_POINT('Ctrl Pts',(38.9312532790372,2.35846024436991,-6.57675715522205));
#38628=CARTESIAN_POINT('Ctrl Pts',(39.0305090812582,5.19987424584941,-4.63655388895342));
#38629=CARTESIAN_POINT('Ctrl Pts',(39.1628501508863,7.36017049505773,-0.568205646741278));
#38630=CARTESIAN_POINT('Ctrl Pts',(39.3282764879214,5.69230109656122,5.49998729522135));
#38631=CARTESIAN_POINT('Ctrl Pts',(39.5267880923636,-1.54528399913325,7.76280333400891));
#38632=CARTESIAN_POINT('Ctrl Pts',(39.7252996968056,-7.35915006569954,2.91409137656859));
#38633=CARTESIAN_POINT('Ctrl Pts',(39.9238113012478,-6.43272694682871,-4.6121769316725));
#38634=CARTESIAN_POINT('Ctrl Pts',(40.0892376382828,-0.762655399166796,
-7.34256931294684));
#38635=CARTESIAN_POINT('Ctrl Pts',(40.2215787079109,3.62747928931603,-5.94791712647381));
#38636=CARTESIAN_POINT('Ctrl Pts',(40.320834510132,6.04636403890181,-3.50107859267866));
#38637=CARTESIAN_POINT('Ctrl Pts',(40.420090312353,6.96434069439297,-0.185156231974706));
#38638=CARTESIAN_POINT('Ctrl Pts',(40.5524313819811,5.98846731119182,4.31662213265117));
#38639=CARTESIAN_POINT('Ctrl Pts',(40.7178577190162,0.797831104453527,7.87499952700156));
#38640=CARTESIAN_POINT('Ctrl Pts',(40.9163693234583,-6.19079075736279,4.93184833901336));
#38641=CARTESIAN_POINT('Ctrl Pts',(41.1148809279004,-7.50183894936851,-2.52416929270096));
#38642=CARTESIAN_POINT('Ctrl Pts',(41.3133925323426,-1.93640733728171,-7.67479502303675));
#38643=CARTESIAN_POINT('Ctrl Pts',(41.4788188693776,4.15674018148683,-6.10053099630842));
#38644=CARTESIAN_POINT('Ctrl Pts',(41.6111599390057,6.60975984556038,-2.20168093097857));
#38645=CARTESIAN_POINT('Ctrl Pts',(41.7104157412267,6.87799991540007,1.22848954688046));
#38646=CARTESIAN_POINT('Ctrl Pts',(41.8096715434478,5.43889228374724,4.35370817391472));
#38647=CARTESIAN_POINT('Ctrl Pts',(41.9420126130758,1.78784629355005,7.16230221394951));
#38648=CARTESIAN_POINT('Ctrl Pts',(42.107438950111,-4.47352975512394,6.52990685626748));
#38649=CARTESIAN_POINT('Ctrl Pts',(42.3059505545531,-7.91180323874318,-0.228883708223626));
#38650=CARTESIAN_POINT('Ctrl Pts',(42.5044621589952,-4.1007018610194,-6.77002677155041));
#38651=CARTESIAN_POINT('Ctrl Pts',(42.7029737634372,3.47466006418408,-7.11188367873607));
#38652=CARTESIAN_POINT('Ctrl Pts',(42.8684001004724,7.11251538672242,-1.97663659961656));
#38653=CARTESIAN_POINT('Ctrl Pts',(43.0007411701004,6.46962751509898,2.58461679049164));
#38654=CARTESIAN_POINT('Ctrl Pts',(43.0999969723216,4.46050782471037,5.37772622478455));
#38655=CARTESIAN_POINT('Ctrl Pts',(43.1992527745425,1.34414215065186,6.83590564714421));
#38656=CARTESIAN_POINT('Ctrl Pts',(43.3315938441707,-3.25734312549581,6.62455154226247));
#38657=CARTESIAN_POINT('Ctrl Pts',(43.4970201812057,-7.63162064985655,2.10012339594401));
#38658=CARTESIAN_POINT('Ctrl Pts',(43.6955317856479,-5.89532495390081,-5.28149239594187));
#38659=CARTESIAN_POINT('Ctrl Pts',(43.89404339009,1.23758341948163,-7.81776218110407));
#38660=CARTESIAN_POINT('Ctrl Pts',(44.092554994532,7.2443178509545,-3.18935901018531));
#38661=CARTESIAN_POINT('Ctrl Pts',(44.2579813315672,6.70837885245484,3.08100966328303));
#38662=CARTESIAN_POINT('Ctrl Pts',(44.3903224011952,3.27328001232696,6.14995626803296));
#38663=CARTESIAN_POINT('Ctrl Pts',(44.4895782034164,-0.0641027450996106,
6.98655567795094));
#38664=CARTESIAN_POINT('Ctrl Pts',(44.5888340056373,-3.38557307509794,6.08886024564441));
#38665=CARTESIAN_POINT('Ctrl Pts',(44.7211750752655,-6.76378221334741,2.95740047063501));
#38666=CARTESIAN_POINT('Ctrl Pts',(44.8866014123005,-7.18457743679441,-3.32174638950854));
#38667=CARTESIAN_POINT('Ctrl Pts',(45.0851130167426,-1.09392875411456,-7.83915417129927));
#38668=CARTESIAN_POINT('Ctrl Pts',(45.2836246211847,5.99124134473033,-5.17243128419034));
#38669=CARTESIAN_POINT('Ctrl Pts',(45.4821362256269,7.59180116516734,2.23980068088031));
#38670=CARTESIAN_POINT('Ctrl Pts',(45.647562562662,3.13524237458443,6.68320451773826));
#38671=CARTESIAN_POINT('Ctrl Pts',(45.7799036322901,-1.46934631616532,6.81009144879777));
#38672=CARTESIAN_POINT('Ctrl Pts',(45.8791594345111,-4.55843154340064,5.29497604028271));
#38673=CARTESIAN_POINT('Ctrl Pts',(45.9784152367321,-6.51596287215306,2.46547196020152));
#38674=CARTESIAN_POINT('Ctrl Pts',(46.1107563063602,-7.075049125615,-2.10680973119107));
#38675=CARTESIAN_POINT('Ctrl Pts',(46.2761826433953,-3.34358078240567,-7.17444210883576));
#38676=CARTESIAN_POINT('Ctrl Pts',(46.4746942478375,4.22423315559067,-6.69364418591888));
#38677=CARTESIAN_POINT('Ctrl Pts',(46.6732058522795,7.91467099856683,-0.0836733226452872));
#38678=CARTESIAN_POINT('Ctrl Pts',(46.8717174567217,4.35296086924962,6.61089129333479));
#38679=CARTESIAN_POINT('Ctrl Pts',(47.0371437937567,-1.91896473551536,7.12829164086005));
#38680=CARTESIAN_POINT('Ctrl Pts',(47.1694848633849,-5.51786181766442,4.25317823503533));
#38681=CARTESIAN_POINT('Ctrl Pts',(47.2687406656058,-6.89938325586998,1.10207989350079));
#38682=CARTESIAN_POINT('Ctrl Pts',(47.367996467827,-6.56824893825758,-2.32259123026316));
#38683=CARTESIAN_POINT('Ctrl Pts',(47.5003375374549,-4.04410314663289,-6.17577502121804));
#38684=CARTESIAN_POINT('Ctrl Pts',(47.6657638744901,2.07690438089424,-7.63797225801001));
#38685=CARTESIAN_POINT('Ctrl Pts',(47.8642754789321,7.54689139350594,-2.38609482944481));
#38686=CARTESIAN_POINT('Ctrl Pts',(48.0627870833744,6.09925517278121,5.04461143972248));
#38687=CARTESIAN_POINT('Ctrl Pts',(48.2612986878164,-0.942193336862589,
7.85903452960222));
#38688=CARTESIAN_POINT('Ctrl Pts',(48.4267250248516,-6.06666383937774,4.20601441192175));
#38689=CARTESIAN_POINT('Ctrl Pts',(48.5590660944796,-6.9597708388828,-0.312912141109297));
#38690=CARTESIAN_POINT('Ctrl Pts',(48.6583218967007,-5.9811056329619,-3.61143251499863));
#38691=CARTESIAN_POINT('Ctrl Pts',(48.7575776989217,-3.51773163372495,-6.01347555835291));
#38692=CARTESIAN_POINT('Ctrl Pts',(48.8899187685498,0.897254114340819,-7.32733938258665));
#38693=CARTESIAN_POINT('Ctrl Pts',(49.0553451055848,6.51627174946588,-4.49336783589115));
#38694=CARTESIAN_POINT('Ctrl Pts',(49.253856710027,7.30444114151449,3.04863212779555));
#38695=CARTESIAN_POINT('Ctrl Pts',(49.452368314469,1.40258595870646,7.78985050363078));
#38696=CARTESIAN_POINT('Ctrl Pts',(49.6508799189113,-5.79226077953301,5.39461463715364));
#38697=CARTESIAN_POINT('Ctrl Pts',(49.8163062559462,-7.3485055151358,-0.703160058113078));
#38698=CARTESIAN_POINT('Ctrl Pts',(49.9486473255744,-5.11392377461454,-4.73118460485842));
#38699=CARTESIAN_POINT('Ctrl Pts',(50.0479031277955,-2.23738779112476,-6.61892478240717));
#38700=CARTESIAN_POINT('Ctrl Pts',(50.1471589300164,1.19454204951979,-6.86362829921216));
#38701=CARTESIAN_POINT('Ctrl Pts',(50.2794999996447,5.41475364451525,-5.01751037293554));
#38702=CARTESIAN_POINT('Ctrl Pts',(50.4449263366795,7.8773894752044,0.773877947383871));
#38703=CARTESIAN_POINT('Ctrl Pts',(50.6434379411219,3.61141451710502,7.04320263985923));
#38704=CARTESIAN_POINT('Ctrl Pts',(50.8419495455637,-3.95665686991791,6.85520857846125));
#38705=CARTESIAN_POINT('Ctrl Pts',(51.0404611500061,-7.90609723594123,0.381809530199271));
#38706=CARTESIAN_POINT('Ctrl Pts',(51.205887487041,-5.15895505946872,-5.28016572350612));
#38707=CARTESIAN_POINT('Ctrl Pts',(51.3382285566692,-0.852288259845684,
-6.91447242094047));
#38708=CARTESIAN_POINT('Ctrl Pts',(51.4374843588902,2.56325929395234,-6.49967469916801));
#38709=CARTESIAN_POINT('Ctrl Pts',(51.5367401611113,5.34252087541995,-4.47144214247698));
#38710=CARTESIAN_POINT('Ctrl Pts',(51.6690812307394,7.37435440786423,-0.337438054345343));
#38711=CARTESIAN_POINT('Ctrl Pts',(51.8345075677744,5.51727330051624,5.67554819809671));
#38712=CARTESIAN_POINT('Ctrl Pts',(52.0330191722166,-1.78762374629298,7.71060435907371));
#38713=CARTESIAN_POINT('Ctrl Pts',(52.2315307766586,-7.44679753937642,2.682205183802));
#38714=CARTESIAN_POINT('Ctrl Pts',(52.4300423811009,-6.28513840933588,-4.81136022315926));
#38715=CARTESIAN_POINT('Ctrl Pts',(52.5954687181358,-0.532343630937353,
-7.36285118903727));
#38716=CARTESIAN_POINT('Ctrl Pts',(52.727809787764,3.81196337228751,-5.83140286604824));
#38717=CARTESIAN_POINT('Ctrl Pts',(52.8270655899849,6.15303729476447,-3.31001532508164));
#38718=CARTESIAN_POINT('Ctrl Pts',(52.9263213922061,6.96672328301192,0.0330278027845019));
#38719=CARTESIAN_POINT('Ctrl Pts',(53.0586624618341,5.85035217015766,4.50203807829726));
#38720=CARTESIAN_POINT('Ctrl Pts',(53.2240887988693,0.550828657694646,7.89612182095554));
#38721=CARTESIAN_POINT('Ctrl Pts',(53.4226004033113,-6.34219873834294,4.7355605163315));
#38722=CARTESIAN_POINT('Ctrl Pts',(53.6211120077535,-7.41911348525517,-2.75785665569876));
#38723=CARTESIAN_POINT('Ctrl Pts',(53.8196236121955,-1.69511601270984,-7.73167082362948));
#38724=CARTESIAN_POINT('Ctrl Pts',(53.9850499492307,4.34574389539973,-5.9673677085381));
#38725=CARTESIAN_POINT('Ctrl Pts',(54.1173910188587,6.67546522902976,-1.99361182626703));
#38726=CARTESIAN_POINT('Ctrl Pts',(54.2166468210798,6.83615553932873,1.44327642714178));
#38727=CARTESIAN_POINT('Ctrl Pts',(54.3159026233008,5.29988531012766,4.52189560221267));
#38728=CARTESIAN_POINT('Ctrl Pts',(54.448243692929,1.56267690427941,7.21477707667661));
#38729=CARTESIAN_POINT('Ctrl Pts',(54.6136700299639,-4.6758243042398,6.38661248999724));
#38730=CARTESIAN_POINT('Ctrl Pts',(54.8121816344062,-7.90075518609565,-0.476535129722538));
#38731=CARTESIAN_POINT('Ctrl Pts',(55.0106932388481,-3.8866824969691,-6.89512272611814));
#38732=CARTESIAN_POINT('Ctrl Pts',(55.2092048432904,3.69566952905561,-6.99958418432969));
#38733=CARTESIAN_POINT('Ctrl Pts',(55.3746311803254,7.17092676886464,-1.75293372632495));
#38734=CARTESIAN_POINT('Ctrl Pts',(55.5069722499535,6.3855153503238,2.78595008006179));
#38735=CARTESIAN_POINT('Ctrl Pts',(55.6062280521746,4.28991286151973,5.51477261939286));
#38736=CARTESIAN_POINT('Ctrl Pts',(55.7054838543956,1.12941171702959,6.87464568623383));
#38737=CARTESIAN_POINT('Ctrl Pts',(55.8378249240237,-3.46319802659206,6.51929649593543));
#38738=CARTESIAN_POINT('Ctrl Pts',(56.0032512610588,-7.69364450906023,1.86010381154267));
#38739=CARTESIAN_POINT('Ctrl Pts',(56.2017628655009,-5.72703990474126,-5.46351829593155));
#38740=CARTESIAN_POINT('Ctrl Pts',(56.400274469943,1.48179515543616,-7.77517211113707));
#38741=CARTESIAN_POINT('Ctrl Pts',(56.5987860743851,7.34064184429667,-2.96093386202206));
#38742=CARTESIAN_POINT('Ctrl Pts',(56.7642124114202,6.60860469874742,3.28957615947717));
#38743=CARTESIAN_POINT('Ctrl Pts',(56.8965534810483,3.07908440665131,6.24944504372459));
#38744=CARTESIAN_POINT('Ctrl Pts',(56.9958092832693,-0.282860206898158,
6.98112165102364));
#38745=CARTESIAN_POINT('Ctrl Pts',(57.0950650854904,-3.57458953547651,5.97985232181189));
#38746=CARTESIAN_POINT('Ctrl Pts',(57.2274061551185,-6.85307794401281,2.74413739936472));
#38747=CARTESIAN_POINT('Ctrl Pts',(57.3928324921536,-7.07703088842817,-3.54510730807145));
#38748=CARTESIAN_POINT('Ctrl Pts',(57.5913440965957,-0.847903606728639,
-7.86956655186127));
#38749=CARTESIAN_POINT('Ctrl Pts',(57.7898557010378,6.15028122011372,-4.98227449605031));
#38750=CARTESIAN_POINT('Ctrl Pts',(57.9883673054799,7.51793678140744,2.47644474444095));
#38751=CARTESIAN_POINT('Ctrl Pts',(58.153793642515,2.92441542669665,6.77810901250529));
#38752=CARTESIAN_POINT('Ctrl Pts',(58.2861347121431,-1.68188846520317,6.76073777989012));
#38753=CARTESIAN_POINT('Ctrl Pts',(58.3853905143641,-4.72201172539709,5.14962859517563));
#38754=CARTESIAN_POINT('Ctrl Pts',(58.4846463165852,-6.58997506047582,2.26021079550644));
#38755=CARTESIAN_POINT('Ctrl Pts',(58.6169873862132,-7.0056028915162,-2.32733656777153));
#38756=CARTESIAN_POINT('Ctrl Pts',(58.7824137232484,-3.11726820308623,-7.27562993640659));
#38757=CARTESIAN_POINT('Ctrl Pts',(58.9809253276904,4.4317775235007,-6.55807641177433));
#38758=CARTESIAN_POINT('Ctrl Pts',(59.1794369321326,7.91340948250359,0.164221200519121));
#38759=CARTESIAN_POINT('Ctrl Pts',(59.3779485365746,4.14380122237507,6.74396496513376));
#38760=CARTESIAN_POINT('Ctrl Pts',(59.5433748736098,-2.1412510287548,7.06470179166561));
#38761=CARTESIAN_POINT('Ctrl Pts',(59.6757159432378,-5.64834680998629,4.07829651348879));
#38762=CARTESIAN_POINT('Ctrl Pts',(59.7749717454589,-6.93051181221684,0.885480335050289));
#38763=CARTESIAN_POINT('Ctrl Pts',(59.87422754768,-6.49229391850386,-2.52714143125686));
#38764=CARTESIAN_POINT('Ctrl Pts',(60.006568617308,-3.84872095303324,-6.2993900021343));
#38765=CARTESIAN_POINT('Ctrl Pts',(60.1719949543432,2.31507421829155,-7.56918644144204));
#38766=CARTESIAN_POINT('Ctrl Pts',(60.3705065587852,7.61791220518773,-2.14858834459484));
#38767=CARTESIAN_POINT('Ctrl Pts',(60.5690181632275,5.93828819827106,5.23313973774365));
#38768=CARTESIAN_POINT('Ctrl Pts',(60.7675297676693,-1.18784242152082,7.82567456537414));
#38769=CARTESIAN_POINT('Ctrl Pts',(60.9329561047047,-6.19540269969449,4.01396970117181));
#38770=CARTESIAN_POINT('Ctrl Pts',(61.0652971743325,-6.94655830765724,-0.53070878656308));
#38771=CARTESIAN_POINT('Ctrl Pts',(61.1645529765538,-5.86507761102045,-3.79696378962774));
#38772=CARTESIAN_POINT('Ctrl Pts',(61.2638087787747,-3.32769012441271,-6.12068644628227));
#38773=CARTESIAN_POINT('Ctrl Pts',(61.3961498484029,1.12627483252932,-7.29564749524797));
#38774=CARTESIAN_POINT('Ctrl Pts',(61.5615761854378,6.65378877091549,-4.28710240296953));
#38775=CARTESIAN_POINT('Ctrl Pts',(61.7600877898801,7.20538857022683,3.27588061328884));
#38776=CARTESIAN_POINT('Ctrl Pts',(61.9585993943221,1.15795340727137,7.82995288281261));
#38777=CARTESIAN_POINT('Ctrl Pts',(62.1571109987642,-5.95835607416243,5.21058009390514));
#38778=CARTESIAN_POINT('Ctrl Pts',(62.3225373357994,-7.32288143850781,-0.932938803387027));
#38779=CARTESIAN_POINT('Ctrl Pts',(62.4548784054274,-4.96325524430359,-4.8890102799759));
#38780=CARTESIAN_POINT('Ctrl Pts',(62.5541342076486,-2.02901416729863,-6.68574385629147));
#38781=CARTESIAN_POINT('Ctrl Pts',(62.6533900098694,1.40889552230351,-6.82285406153834));
#38782=CARTESIAN_POINT('Ctrl Pts',(62.7857310794977,5.56922480504733,-4.84548268433111));
#38783=CARTESIAN_POINT('Ctrl Pts',(62.9511574165326,7.84929142338568,1.02018438150764));
#38784=CARTESIAN_POINT('Ctrl Pts',(63.1496690209748,3.38908043309366,7.152842236377));
#38785=CARTESIAN_POINT('Ctrl Pts',(63.348180625417,-4.16939197496766,6.72794090339327));
#38786=CARTESIAN_POINT('Ctrl Pts',(63.546692229859,-7.91417626981825,0.134037277478446));
#38787=CARTESIAN_POINT('Ctrl Pts',(63.7121185668942,-4.99107271368159,-5.43913233338277));
#38788=CARTESIAN_POINT('Ctrl Pts',(63.8444596365222,-0.635338685615254,
-6.93777117613269));
#38789=CARTESIAN_POINT('Ctrl Pts',(63.9437154387432,2.76554400714119,-6.41621662255914));
#38790=CARTESIAN_POINT('Ctrl Pts',(64.0429712409643,5.47992695258048,-4.30194429673351));
#38791=CARTESIAN_POINT('Ctrl Pts',(64.1753123105923,7.38130471472616,-0.106339464308261));
#38792=CARTESIAN_POINT('Ctrl Pts',(64.3407386476275,5.3368335349973,5.84554187746859));
#38793=CARTESIAN_POINT('Ctrl Pts',(64.5392502520696,-2.02820998866499,7.6508419459786));
#38794=CARTESIAN_POINT('Ctrl Pts',(64.7377618565118,-7.52714034664233,2.44768797897928));
#38795=CARTESIAN_POINT('Ctrl Pts',(64.9362734609538,-6.13138469289272,-5.00582398504777));
#38796=CARTESIAN_POINT('Ctrl Pts',(65.1016997979889,-0.301509679500262,
-7.37591074284501));
#38797=CARTESIAN_POINT('Ctrl Pts',(65.234040867617,3.99270824781552,-5.70916850213125));
#38798=CARTESIAN_POINT('Ctrl Pts',(65.333296669838,6.25367495147746,-3.11570521778876));
#38799=CARTESIAN_POINT('Ctrl Pts',(65.4325524720591,6.96227211668874,0.251179440093837));
#38800=CARTESIAN_POINT('Ctrl Pts',(65.5648935416872,5.70649833797061,4.68303791274987));
#38801=CARTESIAN_POINT('Ctrl Pts',(65.7303198787222,0.303285895553221,7.90949870001355));
#38802=CARTESIAN_POINT('Ctrl Pts',(65.9288314831644,-6.48738556918477,4.53462751719283));
#38803=CARTESIAN_POINT('Ctrl Pts',(66.1273430876064,-7.32911051026348,-2.98883879937283));
#38804=CARTESIAN_POINT('Ctrl Pts',(66.3258546920486,-1.45216192573285,-7.78096252107479));
#38805=CARTESIAN_POINT('Ctrl Pts',(66.4912810290837,4.53048480966573,-5.8283509485403));
#38806=CARTESIAN_POINT('Ctrl Pts',(66.6236220987118,6.73462255592388,-1.78358715873934));
#38807=CARTESIAN_POINT('Ctrl Pts',(66.7228779009328,6.78760548545835,1.65664757441715));
#38808=CARTESIAN_POINT('Ctrl Pts',(66.822133703154,5.15567960323104,4.68564744671614));
#38809=CARTESIAN_POINT('Ctrl Pts',(66.9544747727818,1.33597466947468,7.260174852171));
#38810=CARTESIAN_POINT('Ctrl Pts',(67.1199011098171,-4.87353228461882,6.23705343373919));
#38811=CARTESIAN_POINT('Ctrl Pts',(67.3184127142591,-7.88195715407007,-0.723719155071791));
#38812=CARTESIAN_POINT('Ctrl Pts',(67.5169243187013,-3.66885066862576,-7.01345507920435));
#38813=CARTESIAN_POINT('Ctrl Pts',(67.7154359231434,3.91305393206027,-6.88041886003763));
#38814=CARTESIAN_POINT('Ctrl Pts',(67.8808622601784,7.22230396464096,-1.52751109708982));
#38815=CARTESIAN_POINT('Ctrl Pts',(68.0132033298065,6.29513972075098,2.98455020269193));
#38816=CARTESIAN_POINT('Ctrl Pts',(68.1124591320276,4.11510948079485,5.64641034950249));
#38817=CARTESIAN_POINT('Ctrl Pts',(68.2117149342486,0.913574134491054,6.90664071797512));
#38818=CARTESIAN_POINT('Ctrl Pts',(68.3440560038768,-3.66565735573255,6.40764997957445));
#38819=CARTESIAN_POINT('Ctrl Pts',(68.5094823409118,-7.74811845347451,1.61825269811276));
#38820=CARTESIAN_POINT('Ctrl Pts',(68.7079939453539,-5.55314230167276,-5.64017343059075));
#38821=CARTESIAN_POINT('Ctrl Pts',(68.906505549796,1.72456291095644,-7.72497648317235));
#38822=CARTESIAN_POINT('Ctrl Pts',(69.1050171542383,7.42974649891666,-2.72956244906754));
#38823=CARTESIAN_POINT('Ctrl Pts',(69.2704434912731,6.50238112060189,3.494842318281));
#38824=CARTESIAN_POINT('Ctrl Pts',(69.4027845609014,2.88182229246086,6.34290645397399));
#38825=CARTESIAN_POINT('Ctrl Pts',(69.5020403631223,-0.501239314243825,
6.96861520670999));
#38826=CARTESIAN_POINT('Ctrl Pts',(69.6012961653434,-3.76028584749399,5.8653931038265));
#38827=CARTESIAN_POINT('Ctrl Pts',(69.7336372349715,-6.93524907719399,2.52728720876738));
#38828=CARTESIAN_POINT('Ctrl Pts',(69.8990635720067,-6.96336228722064,-3.76316618635394));
#38829=CARTESIAN_POINT('Ctrl Pts',(70.0975751764487,-0.599684643835917,
-7.89529022500933));
#38830=CARTESIAN_POINT('Ctrl Pts',(70.2960867808908,6.30079599638089,-4.78168947323583));
#38831=CARTESIAN_POINT('Ctrl Pts',(70.4945983853329,7.4414924699285,2.70003404851807));
#38832=CARTESIAN_POINT('Ctrl Pts',(70.6931099897751,1.75530894462229,7.71973735780468));
#38833=CARTESIAN_POINT('Ctrl Pts',(70.8585363268101,-4.30523581206144,5.99894314542976));
#38834=CARTESIAN_POINT('Ctrl Pts',(70.9908773964383,-6.65241429240827,2.04583611782808));
#38835=CARTESIAN_POINT('Ctrl Pts',(71.1232184660662,-6.93093605511931,-2.53987632804942));
#38836=CARTESIAN_POINT('Ctrl Pts',(71.2886448031015,-2.89169548793886,-7.37429860539061));
#38837=CARTESIAN_POINT('Ctrl Pts',(71.4871564075434,4.6447284051371,-6.411379345178));
#38838=CARTESIAN_POINT('Ctrl Pts',(71.6525827445787,7.34317100468254,-0.732288897783634));
#38839=CARTESIAN_POINT('Ctrl Pts',(71.7849238142065,5.93364342986877,3.65309768259248));
#38840=CARTESIAN_POINT('Ctrl Pts',(71.8841796164278,3.47471803823491,6.06097352117865));
#38841=CARTESIAN_POINT('Ctrl Pts',(71.9834354186487,0.155865321197622,6.96515979860947));
#38842=CARTESIAN_POINT('Ctrl Pts',(72.1157764882769,-4.34223294767585,5.97000820865479));
#38843=CARTESIAN_POINT('Ctrl Pts',(72.2812028253119,-7.87819756409372,0.764410097337301));
#38844=CARTESIAN_POINT('Ctrl Pts',(72.4797144297541,-4.90556651422554,-6.21170485827554));
#38845=CARTESIAN_POINT('Ctrl Pts',(72.6782260341962,2.55604705852035,-7.49103801052975));
#38846=CARTESIAN_POINT('Ctrl Pts',(72.8767376386383,7.68293167045214,-1.90379411267946));
#38847=CARTESIAN_POINT('Ctrl Pts',(73.0421639756733,6.08282805842319,4.18262061011101));
#38848=CARTESIAN_POINT('Ctrl Pts',(73.1745050453015,2.17357859296375,6.61905138996127));
#38849=CARTESIAN_POINT('Ctrl Pts',(73.2737608475224,-1.25769345075426,6.87272008061714));
#38850=CARTESIAN_POINT('Ctrl Pts',(73.3730166497437,-4.37677417992924,5.42034849327425));
#38851=CARTESIAN_POINT('Ctrl Pts',(73.5053577193714,-7.16983148085324,1.75740528550872));
#38852=CARTESIAN_POINT('Ctrl Pts',(73.670784056407,-6.51084504293545,-4.50122828872999));
#38853=CARTESIAN_POINT('Ctrl Pts',(73.8692956608486,0.262490856564827,-7.9107594913457));
#38854=CARTESIAN_POINT('Ctrl Pts',(74.0678072652911,6.78738515894909,-4.07190613494002));
#38855=CARTESIAN_POINT('Ctrl Pts',(74.266318869733,7.097059387601,3.50483969846582));
#38856=CARTESIAN_POINT('Ctrl Pts',(74.4317452067681,1.94640508439703,7.12084786428718));
#38857=CARTESIAN_POINT('Ctrl Pts',(74.5640862763962,-2.61207613861328,6.45858981248953));
#38858=CARTESIAN_POINT('Ctrl Pts',(74.6633420786172,-5.39662574857546,4.43762323844));
#38859=CARTESIAN_POINT('Ctrl Pts',(74.7625978808384,-6.84155382034101,1.31509140621307));
#38860=CARTESIAN_POINT('Ctrl Pts',(74.8949389504664,-6.61065472827709,-3.28545453224419));
#38861=CARTESIAN_POINT('Ctrl Pts',(75.0603652875015,-2.06768566612684,-7.64047302147642));
#38862=CARTESIAN_POINT('Ctrl Pts',(75.2588768919436,5.30648781615955,-5.87283622208682));
#38863=CARTESIAN_POINT('Ctrl Pts',(75.4573884963857,7.81243444661612,1.27078175373805));
#38864=CARTESIAN_POINT('Ctrl Pts',(75.6559001008279,3.15855669885345,7.25780074116703));
#38865=CARTESIAN_POINT('Ctrl Pts',(75.8213264378629,-3.10947875451868,6.69523033571205));
#38866=CARTESIAN_POINT('Ctrl Pts',(75.953667507491,-6.16380552501382,3.2471257426054));
#38867=CARTESIAN_POINT('Ctrl Pts',(76.0529233097121,-6.98622033545058,-0.0937807393895811));
#38868=CARTESIAN_POINT('Ctrl Pts',(76.1521791119331,-6.07442354693653,-3.41140773149026));
#38869=CARTESIAN_POINT('Ctrl Pts',(76.2845201815612,-2.92864154611183,-6.7762840899402));
#38870=CARTESIAN_POINT('Ctrl Pts',(76.4499465185962,3.35223617886508,-7.1704019847288));
#38871=CARTESIAN_POINT('Ctrl Pts',(76.6484581230384,7.84373040163857,-1.06061851150057));
#38872=CARTESIAN_POINT('Ctrl Pts',(76.8469697274805,5.14693409302365,6.01315954241379));
#38873=CARTESIAN_POINT('Ctrl Pts',(77.0454813319226,-2.27203010019493,7.58221809534107));
#38874=CARTESIAN_POINT('Ctrl Pts',(77.2109076689577,-6.69646258572395,3.10682413588426));
#38875=CARTESIAN_POINT('Ctrl Pts',(77.3432487385858,-6.80378828733636,-1.49826201944722));
#38876=CARTESIAN_POINT('Ctrl Pts',(77.4425045408069,-5.27556425470762,-4.58088323333947));
#38877=CARTESIAN_POINT('Ctrl Pts',(77.5417603430279,-2.43777019952231,-6.52637729465111));
#38878=CARTESIAN_POINT('Ctrl Pts',(77.674101412656,2.13684521112816,-7.06603565777769));
#38879=CARTESIAN_POINT('Ctrl Pts',(77.839527749691,7.18858075671824,-3.31307390887204));
#38880=CARTESIAN_POINT('Ctrl Pts',(78.0380393541333,6.67563944036266,4.25262933992035));
#38881=CARTESIAN_POINT('Ctrl Pts',(78.2365509585752,0.0500514030952952,
7.91495502814294));
#38882=CARTESIAN_POINT('Ctrl Pts',(78.4350625630174,-6.62932282688847,4.32483882687015));
#38883=CARTESIAN_POINT('Ctrl Pts',(78.6004889000525,-7.12007564968641,-1.94922808210056));
#38884=CARTESIAN_POINT('Ctrl Pts',(78.7328299696805,-4.2297002327542,-5.53587934106734));
#38885=CARTESIAN_POINT('Ctrl Pts',(78.8320857719017,-1.07276168170734,-6.90400259105531));
#38886=CARTESIAN_POINT('Ctrl Pts',(78.9313415741226,2.35047189900519,-6.55832341302287));
#38887=CARTESIAN_POINT('Ctrl Pts',(79.0636826437508,6.19289846700909,-4.01783224520675));
#38888=CARTESIAN_POINT('Ctrl Pts',(79.2291089807858,7.62908074771822,2.10933140267323));
#38889=CARTESIAN_POINT('Ctrl Pts',(79.427620585228,2.35401444720104,7.55695932388457));
#38890=CARTESIAN_POINT('Ctrl Pts',(79.62613218967,-5.07047528444934,6.07777086029618));
#38891=CARTESIAN_POINT('Ctrl Pts',(79.8246437941122,-7.85496122597134,-0.975569659222166));
#38892=CARTESIAN_POINT('Ctrl Pts',(79.9900701311471,-4.18020554900285,-6.08447606137072));
#38893=CARTESIAN_POINT('Ctrl Pts',(80.1224112007755,0.342474109717358,-6.95837880702041));
#38894=CARTESIAN_POINT('Ctrl Pts',(80.2216670029962,3.63680739682284,-5.96571046577456));
#38895=CARTESIAN_POINT('Ctrl Pts',(80.3209228052176,6.02836446611632,-3.4921549223199));
#38896=CARTESIAN_POINT('Ctrl Pts',(80.4532638748454,7.32346177601447,0.92837222522132));
#38897=CARTESIAN_POINT('Ctrl Pts',(80.6186902118807,4.46564646622055,6.53530057918074));
#38898=CARTESIAN_POINT('Ctrl Pts',(80.8172018163227,-3.07963355695854,7.29142478500135));
#38899=CARTESIAN_POINT('Ctrl Pts',(81.0157134207649,-7.79573834066554,1.36948237095418));
#38900=CARTESIAN_POINT('Ctrl Pts',(81.2142250252069,-5.36996070176256,-5.81512459737828));
#38901=CARTESIAN_POINT('Ctrl Pts',(81.3796513622421,0.734369833000959,-7.3454522203664));
#38902=CARTESIAN_POINT('Ctrl Pts',(81.5119924318701,4.75286563427561,-5.09377977540636));
#38903=CARTESIAN_POINT('Ctrl Pts',(81.6112482340912,6.62836938468186,-2.20925071081801));
#38904=CARTESIAN_POINT('Ctrl Pts',(81.7105040363122,6.85849201081093,1.22368765437101));
#38905=CARTESIAN_POINT('Ctrl Pts',(81.8428451059403,4.994463473249,5.43601894659032));
#38906=CARTESIAN_POINT('Ctrl Pts',(82.0082714429754,-0.807333759365405,
7.87403100212955));
#38907=CARTESIAN_POINT('Ctrl Pts',(82.2067830474175,-7.05848021745994,3.58146272634573));
#38908=CARTESIAN_POINT('Ctrl Pts',(82.4052946518597,-6.8383390271391,-3.98574178671712));
#38909=CARTESIAN_POINT('Ctrl Pts',(82.6038062563016,-0.348221341641362,
-7.90764781200667));
#38910=CARTESIAN_POINT('Ctrl Pts',(82.769232593337,5.3020330905482,-5.13647860698734));
#38911=CARTESIAN_POINT('Ctrl Pts',(82.9015736629648,6.91803051641495,-0.822908203731382));
#38912=CARTESIAN_POINT('Ctrl Pts',(83.0008294651861,6.48872744559679,2.59084649097491));
#38913=CARTESIAN_POINT('Ctrl Pts',(83.100085267407,4.44870701128368,5.36146715606584));
#38914=CARTESIAN_POINT('Ctrl Pts',(83.2324263370351,0.306109085628454,7.37572129360934));
#38915=CARTESIAN_POINT('Ctrl Pts',(83.3978526740702,-5.69893411744994,5.49311404819464));
#38916=CARTESIAN_POINT('Ctrl Pts',(83.5963642785123,-7.70294104450956,-1.82036191601753));
#38917=CARTESIAN_POINT('Ctrl Pts',(83.7948758829544,-2.65054732403995,-7.45812423626086));
#38918=CARTESIAN_POINT('Ctrl Pts',(83.9933874873965,4.83801579600438,-6.26464326032379));
#38919=CARTESIAN_POINT('Ctrl Pts',(84.1588138244316,7.36504612864948,-0.501061768818908));
#38920=CARTESIAN_POINT('Ctrl Pts',(84.2911548940597,5.81515720355302,3.83670051421568));
#38921=CARTESIAN_POINT('Ctrl Pts',(84.3904106962808,3.2838476358709,6.16704257382927));
#38922=CARTESIAN_POINT('Ctrl Pts',(84.4896664985018,-0.0626218303453555,
6.96652012443667));
#38923=CARTESIAN_POINT('Ctrl Pts',(84.6220075681298,-4.5268494897441,5.83117493053597));
#38924=CARTESIAN_POINT('Ctrl Pts',(84.7874339051651,-7.89839047263792,0.51728131925656));
#38925=CARTESIAN_POINT('Ctrl Pts',(84.985945509607,-4.70857641573474,-6.36225796220678));
#38926=CARTESIAN_POINT('Ctrl Pts',(85.1844571140492,2.78934783134507,-7.40733129515937));
#38927=CARTESIAN_POINT('Ctrl Pts',(85.3829687184914,7.73880184004112,-1.66225693022602));
#38928=CARTESIAN_POINT('Ctrl Pts',(85.5483950555264,5.94885334375496,4.3710537937438));
#38929=CARTESIAN_POINT('Ctrl Pts',(85.6807361251546,1.96523676419218,6.68387377188444));
#38930=CARTESIAN_POINT('Ctrl Pts',(85.7799919273754,-1.47230308472022,6.82996288641172));
#38931=CARTESIAN_POINT('Ctrl Pts',(85.8792477295967,-4.54436847615697,5.28062868328456));
#38932=CARTESIAN_POINT('Ctrl Pts',(86.0115887992246,-7.22135016146877,1.53201475801043));
#38933=CARTESIAN_POINT('Ctrl Pts',(86.1770151362597,-6.36669217588134,-4.70291215727867));
#38934=CARTESIAN_POINT('Ctrl Pts',(86.375526740702,0.510092880993074,-7.8986596010486));
#38935=CARTESIAN_POINT('Ctrl Pts',(86.5740383451439,6.91157096571897,-3.85735725935614));
#38936=CARTESIAN_POINT('Ctrl Pts',(86.7725499495862,6.98382199278953,3.72537010168621));
#38937=CARTESIAN_POINT('Ctrl Pts',(86.9379762866211,1.72245613756997,7.17830845167958));
#38938=CARTESIAN_POINT('Ctrl Pts',(87.0703173562493,-2.81305032408128,6.37362314637467));
#38939=CARTESIAN_POINT('Ctrl Pts',(87.1695731584703,-5.53294621770099,4.26644765057143));
#38940=CARTESIAN_POINT('Ctrl Pts',(87.2688289606914,-6.87938134896713,1.10019834270945));
#38941=CARTESIAN_POINT('Ctrl Pts',(87.4011700303194,-6.50452616627225,-3.49086045633253));
#38942=CARTESIAN_POINT('Ctrl Pts',(87.5665963673546,-1.82740477450515,-7.70147672927888));
#38943=CARTESIAN_POINT('Ctrl Pts',(87.7651079717965,5.48779720739767,-5.7037794532184));
#38944=CARTESIAN_POINT('Ctrl Pts',(87.9636195762388,7.76880736003202,1.51481036542182));
#38945=CARTESIAN_POINT('Ctrl Pts',(88.1621311806809,2.92972443199612,7.35315352580599));
#38946=CARTESIAN_POINT('Ctrl Pts',(88.327557517716,-3.31761953294659,6.59457110113453));
#38947=CARTESIAN_POINT('Ctrl Pts',(88.4598985873441,-6.26246846883917,3.05250926527866));
#38948=CARTESIAN_POINT('Ctrl Pts',(88.5591543895651,-6.97985708577932,-0.312513143937597));
#38949=CARTESIAN_POINT('Ctrl Pts',(88.6584101917861,-5.96461367324412,-3.59995942571118));
#38950=CARTESIAN_POINT('Ctrl Pts',(88.7907512614142,-2.71500107481349,-6.86467308304396));
#38951=CARTESIAN_POINT('Ctrl Pts',(88.9561775984493,3.5751382292627,-7.06190757962553));
#38952=CARTESIAN_POINT('Ctrl Pts',(89.1546892028915,7.87309740409461,-0.814466393484584));
#38953=CARTESIAN_POINT('Ctrl Pts',(89.3532008073335,4.95610342639328,6.17139020540508));
#38954=CARTESIAN_POINT('Ctrl Pts',(89.5517124117758,-2.50835825604882,7.5073491247457));
#38955=CARTESIAN_POINT('Ctrl Pts',(89.7171387488106,-6.79047064086134,2.89559594020068));
#38956=CARTESIAN_POINT('Ctrl Pts',(89.849479818439,-6.75353219428684,-1.71059259864776));
#38957=CARTESIAN_POINT('Ctrl Pts',(89.9487356206597,-5.1295232397943,-4.74384451004123));
#38958=CARTESIAN_POINT('Ctrl Pts',(90.0479914228811,-2.23219648638674,-6.59951687504316));
#38959=CARTESIAN_POINT('Ctrl Pts',(90.1803324925088,2.35707505352007,-6.99565326223221));
#38960=CARTESIAN_POINT('Ctrl Pts',(90.3457588295442,7.28880630570573,-3.08633353016368));
#38961=CARTESIAN_POINT('Ctrl Pts',(90.5442704339861,6.53919125029974,4.4595959494645));
#38962=CARTESIAN_POINT('Ctrl Pts',(90.7427820384283,-0.19783552455262,7.91264047873421));
#38963=CARTESIAN_POINT('Ctrl Pts',(90.9412936428704,-6.76150679729253,4.11511577621764));
#38964=CARTESIAN_POINT('Ctrl Pts',(91.1067199799056,-7.05554211211308,-2.17124224293496));
#38965=CARTESIAN_POINT('Ctrl Pts',(91.2390610495335,-4.05426579474709,-5.66562026642814));
#38966=CARTESIAN_POINT('Ctrl Pts',(91.3383168517547,-0.856031844848053,
-6.93421076140923));
#38967=CARTESIAN_POINT('Ctrl Pts',(91.4375726539757,2.55469760093386,-6.48150015857438));
#38968=CARTESIAN_POINT('Ctrl Pts',(91.5699137236037,6.31568235787109,-3.8219267036121));
#38969=CARTESIAN_POINT('Ctrl Pts',(91.735340060639,7.55928381707499,2.34720689212017));
#38970=CARTESIAN_POINT('Ctrl Pts',(91.933851665081,2.11620841207976,7.62697057796343));
#38971=CARTESIAN_POINT('Ctrl Pts',(92.1323632695231,-5.25831810102433,5.91600447843957));
#38972=CARTESIAN_POINT('Ctrl Pts',(92.3308748739652,-7.82055805653044,-1.22107481586712));
#38973=CARTESIAN_POINT('Ctrl Pts',(92.4963012110002,-3.98761569413683,-6.21239796287884));
#38974=CARTESIAN_POINT('Ctrl Pts',(92.6286422806284,0.560212663843672,-6.94424120470236));
#38975=CARTESIAN_POINT('Ctrl Pts',(92.7278980828494,3.82184411568555,-5.8488953622404));
#38976=CARTESIAN_POINT('Ctrl Pts',(92.8271538850705,6.13476709898446,-3.30165970067103));
#38977=CARTESIAN_POINT('Ctrl Pts',(92.9594949546986,7.29079730496156,1.15725625134272));
#38978=CARTESIAN_POINT('Ctrl Pts',(93.1249212917336,4.25879872825919,6.67194015363493));
#38979=CARTESIAN_POINT('Ctrl Pts',(93.3234328961758,-3.30645922123453,7.19140776613244));
#38980=CARTESIAN_POINT('Ctrl Pts',(93.5219445006179,-7.83480117000039,1.12468167364702));
#38981=CARTESIAN_POINT('Ctrl Pts',(93.7204561050599,-5.18522225368139,-5.98043662297633));
#38982=CARTESIAN_POINT('Ctrl Pts',(93.8858824420952,0.96403765515393,-7.31885228521195));
#38983=CARTESIAN_POINT('Ctrl Pts',(94.0182235117231,4.91004985228958,-4.94244216818445));
#38984=CARTESIAN_POINT('Ctrl Pts',(94.1174793139444,6.69430269395043,-2.00059512265878));
#38985=CARTESIAN_POINT('Ctrl Pts',(94.2167351161651,6.81680757716476,1.43786598601073));
#38986=CARTESIAN_POINT('Ctrl Pts',(94.3490761857935,4.82178115027497,5.58975794754651));
#38987=CARTESIAN_POINT('Ctrl Pts',(94.5145025228283,-1.05351861191065,7.84488690523109));
#38988=CARTESIAN_POINT('Ctrl Pts',(94.7130141272707,-7.16717435960562,3.35866490431669));
#38989=CARTESIAN_POINT('Ctrl Pts',(94.9115257317125,-6.71016881124756,-4.19793434501272));
#38990=CARTESIAN_POINT('Ctrl Pts',(95.1100373361551,-0.100417005100013,
-7.91467424766143));
#38991=CARTESIAN_POINT('Ctrl Pts',(95.2754636731895,5.46028510951729,-4.96792249296327));
#38992=CARTESIAN_POINT('Ctrl Pts',(95.4078047428182,6.9404074694083,-0.605861614891436));
#38993=CARTESIAN_POINT('Ctrl Pts',(95.5070605450388,6.40441082567987,2.7927748528931));
#38994=CARTESIAN_POINT('Ctrl Pts',(95.6063163472603,4.27862700004775,5.49815197428002));
#38995=CARTESIAN_POINT('Ctrl Pts',(95.7386574168879,0.0749830561122438,
7.38168984139835));
#38996=CARTESIAN_POINT('Ctrl Pts',(95.9040837539233,-5.86815976306963,5.31195378524688));
#38997=CARTESIAN_POINT('Ctrl Pts',(96.1025953583653,-7.64215717114619,-2.06069211964716));
#38998=CARTESIAN_POINT('Ctrl Pts',(96.3011069628075,-2.41569094255804,-7.53747010014103));
#38999=CARTESIAN_POINT('Ctrl Pts',(96.4996185672496,5.03182466448517,-6.11006485787073));
#39000=CARTESIAN_POINT('Ctrl Pts',(96.6650449042846,7.3771249924399,-0.270174423708261));
#39001=CARTESIAN_POINT('Ctrl Pts',(96.7973859739128,5.69215614644194,4.01692451290047));
#39002=CARTESIAN_POINT('Ctrl Pts',(96.8966417761337,3.08911177755644,6.26685390198305));
#39003=CARTESIAN_POINT('Ctrl Pts',(96.995897578355,-0.280752591029069,6.96114229997113));
#39004=CARTESIAN_POINT('Ctrl Pts',(97.1282386479826,-4.70723660648295,5.68655351719244));
#39005=CARTESIAN_POINT('Ctrl Pts',(97.2936649850182,-7.91071568063838,0.269683966171925));
#39006=CARTESIAN_POINT('Ctrl Pts',(97.4921765894599,-4.50702848227491,-6.50658992871379));
#39007=CARTESIAN_POINT('Ctrl Pts',(97.6906881939024,3.01994556208542,-7.31634793066305));
#39008=CARTESIAN_POINT('Ctrl Pts',(97.8891997983443,7.78706103537034,-1.41909564615117));
#39009=CARTESIAN_POINT('Ctrl Pts',(98.0546261353794,5.80905306594097,4.55520250377396));
#39010=CARTESIAN_POINT('Ctrl Pts',(98.1869672050076,1.75496269546036,6.742138390404));
#39011=CARTESIAN_POINT('Ctrl Pts',(98.2862230072284,-1.68546607162555,6.78050687813509));
#39012=CARTESIAN_POINT('Ctrl Pts',(98.3854788094498,-4.70750625791352,5.13572866977243));
#39013=CARTESIAN_POINT('Ctrl Pts',(98.5178198790775,-7.26578451938068,1.30512171510342));
#39014=CARTESIAN_POINT('Ctrl Pts',(98.6832462161129,-6.21629458823582,-4.89998302178471));
#39015=CARTESIAN_POINT('Ctrl Pts',(98.8817578205548,0.757194779261698,-7.87881173190068));
#39016=CARTESIAN_POINT('Ctrl Pts',(99.0802694249971,7.0289769917291,-3.63902468942159));
#39017=CARTESIAN_POINT('Ctrl Pts',(99.2787810294391,6.86373414608865,3.94224626238962));
#39018=CARTESIAN_POINT('Ctrl Pts',(99.4442073664742,1.49681757276813,7.22872772534415));
#39019=CARTESIAN_POINT('Ctrl Pts',(99.5765484361023,-3.01126513256809,6.28240451094936));
#39020=CARTESIAN_POINT('Ctrl Pts',(99.6758042383233,-5.66383935284861,4.09108704235948));
#39021=CARTESIAN_POINT('Ctrl Pts',(99.7750600405444,-6.91046079330171,0.884226080851057));
#39022=CARTESIAN_POINT('Ctrl Pts',(99.9074011101725,-6.39201722787976,-3.69284214823692));
#39023=CARTESIAN_POINT('Ctrl Pts',(100.072827447207,-1.58533135460785,-7.75492595178093));
#39024=CARTESIAN_POINT('Ctrl Pts',(100.27133905165,5.66372354179168,-5.52912776870199));
#39025=CARTESIAN_POINT('Ctrl Pts',(100.469850656092,7.71755974363839,1.75735307888005));
#39026=CARTESIAN_POINT('Ctrl Pts',(100.668362260534,2.69801835775111,7.44129350064531));
#39027=CARTESIAN_POINT('Ctrl Pts',(100.833788597569,-3.52250601247792,6.487443160858));
#39028=CARTESIAN_POINT('Ctrl Pts',(100.966129667197,-6.35498847103736,2.85489853949308));
#39029=CARTESIAN_POINT('Ctrl Pts',(101.065385469418,-6.96664719799234,-0.530939000021162));
#39030=CARTESIAN_POINT('Ctrl Pts',(101.164641271639,-5.84895302775269,-3.78497987008646));
#39031=CARTESIAN_POINT('Ctrl Pts',(101.296982341267,-2.49869742150455,-6.9463284236403));
#39032=CARTESIAN_POINT('Ctrl Pts',(101.462408678302,3.79453337725676,-6.94648605198287));
#39033=CARTESIAN_POINT('Ctrl Pts',(101.660920282744,7.89474157672574,-0.567515354149183));
#39034=CARTESIAN_POINT('Ctrl Pts',(101.859431887187,4.76041124955647,6.32356726662831));
#39035=CARTESIAN_POINT('Ctrl Pts',(102.057943491629,-2.74222592869338,7.42511609185407));
#39036=CARTESIAN_POINT('Ctrl Pts',(102.223369828664,-6.87781782969463,2.68152741452352));
#39037=CARTESIAN_POINT('Ctrl Pts',(102.355710898292,-6.69665146836396,-1.92124523397596));
#39038=CARTESIAN_POINT('Ctrl Pts',(102.454966700513,-4.97845060478972,-4.90215248423675));
#39039=CARTESIAN_POINT('Ctrl Pts',(102.554222502734,-2.02443318093161,-6.66618289831267));
#39040=CARTESIAN_POINT('Ctrl Pts',(102.686563572362,2.57499280848366,-6.91840873391956));
#39041=CARTESIAN_POINT('Ctrl Pts',(102.851989909397,7.38188216406195,-2.85656572432764));
#39042=CARTESIAN_POINT('Ctrl Pts',(103.050501513839,6.39632867735181,4.66218807983374));
#39043=CARTESIAN_POINT('Ctrl Pts',(103.249013118281,-0.445528392606267,
7.90256431115402));
#39044=CARTESIAN_POINT('Ctrl Pts',(103.447524722723,-6.88705831242505,3.90135615173695));
#39045=CARTESIAN_POINT('Ctrl Pts',(103.612951059759,-6.98408769597376,-2.39112660229325));
#39046=CARTESIAN_POINT('Ctrl Pts',(103.745292129387,-3.87485447150524,-5.78980370675049));
#39047=CARTESIAN_POINT('Ctrl Pts',(103.844547931608,-0.638462314547805,
-6.95761706874731));
#39048=CARTESIAN_POINT('Ctrl Pts',(103.943803733829,2.75641736475526,-6.39831911131053));
#39049=CARTESIAN_POINT('Ctrl Pts',(104.076144803457,6.4322711087958,-3.62227218122517));
#39050=CARTESIAN_POINT('Ctrl Pts',(104.241571140492,7.48207188069434,2.58277997359283));
#39051=CARTESIAN_POINT('Ctrl Pts',(104.440082744934,1.87632655891563,7.68950043201341));
#39052=CARTESIAN_POINT('Ctrl Pts',(104.638594349376,-5.44100296080544,5.74843500509099));
#39053=CARTESIAN_POINT('Ctrl Pts',(104.837105953818,-7.77848359392374,-1.46538220120157));
#39054=CARTESIAN_POINT('Ctrl Pts',(105.002532290853,-3.79111433187881,-6.33422604138052));
#39055=CARTESIAN_POINT('Ctrl Pts',(105.134873360482,0.777401697416134,-6.92329189505096));
#39056=CARTESIAN_POINT('Ctrl Pts',(105.234129162702,4.00313193543719,-5.72634300828974));
#39057=CARTESIAN_POINT('Ctrl Pts',(105.333384964924,6.23515205328682,-3.10792581387005));
#39058=CARTESIAN_POINT('Ctrl Pts',(105.465726034551,7.25098119224185,1.38500506214225));
#39059=CARTESIAN_POINT('Ctrl Pts',(105.631152371587,4.04777347188614,6.80203522519585));
#39060=CARTESIAN_POINT('Ctrl Pts',(105.829663976029,-3.53004152739988,7.08433643778901));
#39061=CARTESIAN_POINT('Ctrl Pts',(106.028175580471,-7.86617874706874,0.878778052190405));
#39062=CARTESIAN_POINT('Ctrl Pts',(106.226687184913,-4.99539752540193,-6.13988293097007));
#39063=CARTESIAN_POINT('Ctrl Pts',(106.392113521948,1.19275979698265,-7.28507217598246));
#39064=CARTESIAN_POINT('Ctrl Pts',(106.524454591576,5.06241779407946,-4.78625786431911));
#39065=CARTESIAN_POINT('Ctrl Pts',(106.623710393797,6.75366933964939,-1.78997403676776));
#39066=CARTESIAN_POINT('Ctrl Pts',(106.722966196018,6.76843668239335,1.65062819852489));
#39067=CARTESIAN_POINT('Ctrl Pts',(106.855307265646,4.64436855831348,5.73802618614398));
#39068=CARTESIAN_POINT('Ctrl Pts',(107.020733602682,-1.29866899872058,7.80802255608828));
#39069=CARTESIAN_POINT('Ctrl Pts',(107.219245207124,-7.26883987637063,3.13261426953325));
#39070=CARTESIAN_POINT('Ctrl Pts',(107.417756811566,-6.57541326790252,-4.40608594330653));
#39071=CARTESIAN_POINT('Ctrl Pts',(107.616268416008,0.147479460587251,-7.91378549378608));
#39072=CARTESIAN_POINT('Ctrl Pts',(107.781694753043,5.61319225826337,-4.79475969318229));
#39073=CARTESIAN_POINT('Ctrl Pts',(107.914035822671,6.95596082548192,-0.387848333920882));
#39074=CARTESIAN_POINT('Ctrl Pts',(108.013291624892,6.31384625566456,2.99115031483452));
#39075=CARTESIAN_POINT('Ctrl Pts',(108.112547427113,4.10428660238,5.63094528514316));
#39076=CARTESIAN_POINT('Ctrl Pts',(108.244888496741,-0.156076618085431,
7.37716885209829));
#39077=CARTESIAN_POINT('Ctrl Pts',(108.410314833777,-6.03194807359435,5.13225398584684));
#39078=CARTESIAN_POINT('Ctrl Pts',(108.608826438218,-7.57316344147741,-2.31035707660512));
#39079=CARTESIAN_POINT('Ctrl Pts',(108.774252775254,-3.07991499223872,-6.70713847843066));
#39080=CARTESIAN_POINT('Ctrl Pts',(108.906593844881,1.53030863923424,-6.79781064773029));
#39081=CARTESIAN_POINT('Ctrl Pts',(109.005849647103,4.59552813494485,-5.25753008669525));
#39082=CARTESIAN_POINT('Ctrl Pts',(109.105105449324,6.55166018357511,-2.40598671557301));
#39083=CARTESIAN_POINT('Ctrl Pts',(109.171275984138,6.78587654135638,-0.125430911852007));
#39084=CARTESIAN_POINT('Ctrl Pts',(109.204361251545,6.62354718454475,0.976096068216178));
#39085=CARTESIAN_POINT('Ctrl Pts',(30.9296387484553,-1.74764629024929,6.21616713138321));
#39086=CARTESIAN_POINT('Ctrl Pts',(30.9627240158623,-2.78142405570536,5.92552535188211));
#39087=CARTESIAN_POINT('Ctrl Pts',(31.0288945506764,-4.69724081460228,4.82165246972101));
#39088=CARTESIAN_POINT('Ctrl Pts',(31.1281503528974,-6.43804454172866,1.97690416673953));
#39089=CARTESIAN_POINT('Ctrl Pts',(31.2274061551185,-6.58774752332024,-1.32825939138557));
#39090=CARTESIAN_POINT('Ctrl Pts',(31.3597472247465,-4.69328518013838,-5.35182557713039));
#39091=CARTESIAN_POINT('Ctrl Pts',(31.5251735617817,0.946620568444218,-7.57747210463679));
#39092=CARTESIAN_POINT('Ctrl Pts',(31.7236851662237,6.89312828841085,-3.29096731508787));
#39093=CARTESIAN_POINT('Ctrl Pts',(31.8891115032589,6.55695624239769,2.76629759413725));
#39094=CARTESIAN_POINT('Ctrl Pts',(32.0214525728869,3.34250580260362,5.83017495152525));
#39095=CARTESIAN_POINT('Ctrl Pts',(32.120708375108,0.148489860278677,6.73662245379208));
#39096=CARTESIAN_POINT('Ctrl Pts',(32.219964177329,-3.07942669717768,5.97199294502161));
#39097=CARTESIAN_POINT('Ctrl Pts',(32.3523052469571,-6.43114181568573,3.05509788385159));
#39098=CARTESIAN_POINT('Ctrl Pts',(32.5177315839922,-7.02605788339069,-2.9850845489194));
#39099=CARTESIAN_POINT('Ctrl Pts',(32.7162431884343,-1.29137128331862,-7.52386125263412));
#39100=CARTESIAN_POINT('Ctrl Pts',(32.9147547928764,5.61931759596494,-5.16711469712653));
#39101=CARTESIAN_POINT('Ctrl Pts',(33.1132663973185,7.38605346602491,1.92984446273495));
#39102=CARTESIAN_POINT('Ctrl Pts',(33.2786927343536,3.22420823648018,6.34785971429795));
#39103=CARTESIAN_POINT('Ctrl Pts',(33.4110338039817,-1.21075736553802,6.60924292677451));
#39104=CARTESIAN_POINT('Ctrl Pts',(33.5102896062028,-4.2343605016059,5.24198775609974));
#39105=CARTESIAN_POINT('Ctrl Pts',(33.6095454084238,-6.20686614770307,2.57349290017741));
#39106=CARTESIAN_POINT('Ctrl Pts',(33.7418864780519,-6.88391407523792,-1.81725837294228));
#39107=CARTESIAN_POINT('Ctrl Pts',(33.907312815087,-3.43987083363875,-6.8151117023347));
#39108=CARTESIAN_POINT('Ctrl Pts',(34.1058244195291,3.8699555241471,-6.58019622848891));
#39109=CARTESIAN_POINT('Ctrl Pts',(34.3043360239712,7.62714385347594,-0.319706138503197));
#39110=CARTESIAN_POINT('Ctrl Pts',(34.5028476284133,4.39588281579082,6.24136747571982));
#39111=CARTESIAN_POINT('Ctrl Pts',(34.6682739654485,-1.63456982395356,6.92956681052015));
#39112=CARTESIAN_POINT('Ctrl Pts',(34.8006150350764,-5.19071062760659,4.26668055825536));
#39113=CARTESIAN_POINT('Ctrl Pts',(34.8998708372976,-6.61765701788971,1.27077618895782));
#39114=CARTESIAN_POINT('Ctrl Pts',(34.9991266395185,-6.40188140602722,-2.04057696131233));
#39115=CARTESIAN_POINT('Ctrl Pts',(35.1314677091467,-4.08500492716994,-5.8312476858528));
#39116=CARTESIAN_POINT('Ctrl Pts',(35.2968940461817,1.77142835594066,-7.42566455594743));
#39117=CARTESIAN_POINT('Ctrl Pts',(35.4954056506239,7.2030680549125,-2.52811156639923));
#39118=CARTESIAN_POINT('Ctrl Pts',(35.6939172550659,6.03198848328303,4.67874475198411));
#39119=CARTESIAN_POINT('Ctrl Pts',(35.8924288595082,-0.670900469029075,
7.60449505762471));
#39120=CARTESIAN_POINT('Ctrl Pts',(36.0578551965431,-5.72117530867311,4.23779044678305));
#39121=CARTESIAN_POINT('Ctrl Pts',(36.1901962661713,-6.71860690707006,-0.0914394363855131));
#39122=CARTESIAN_POINT('Ctrl Pts',(36.2894520683923,-5.8748072835785,-3.30074170159639));
#39123=CARTESIAN_POINT('Ctrl Pts',(36.3887078706134,-3.57268564284483,-5.69069040089914));
#39124=CARTESIAN_POINT('Ctrl Pts',(36.5210489402414,0.643638183052046,-7.09058845752315));
#39125=CARTESIAN_POINT('Ctrl Pts',(36.6864752772765,6.14591436535152,-4.52837599322407));
#39126=CARTESIAN_POINT('Ctrl Pts',(36.8849868817187,7.1334925448268,2.71823869833564));
#39127=CARTESIAN_POINT('Ctrl Pts',(37.0834984861608,1.58735598268625,7.46698322566606));
#39128=CARTESIAN_POINT('Ctrl Pts',(37.2820100906028,-5.4207541093524,5.37530254108901));
#39129=CARTESIAN_POINT('Ctrl Pts',(37.447436427638,-7.10513022063766,-0.455893992601426));
#39130=CARTESIAN_POINT('Ctrl Pts',(37.579777497266,-5.07267154871018,-4.40636395457348));
#39131=CARTESIAN_POINT('Ctrl Pts',(37.6790332994871,-2.35673207543457,-6.31300802510474));
#39132=CARTESIAN_POINT('Ctrl Pts',(37.7782891017082,0.944226464651675,-6.65255412038963));
#39133=CARTESIAN_POINT('Ctrl Pts',(37.9106301713362,5.06823027977708,-5.00037564747394));
#39134=CARTESIAN_POINT('Ctrl Pts',(38.0760565083713,7.61710545174979,0.508091585475629));
#39135=CARTESIAN_POINT('Ctrl Pts',(38.2745681128134,3.694095804285,6.68050849089578));
#39136=CARTESIAN_POINT('Ctrl Pts',(38.4730797172555,-3.60713443837236,6.72786137280452));
#39137=CARTESIAN_POINT('Ctrl Pts',(38.6715913216977,-7.60987439777963,0.606847734052926));
#39138=CARTESIAN_POINT('Ctrl Pts',(38.8370176587327,-5.13266210331478,-4.93421670763416));
#39139=CARTESIAN_POINT('Ctrl Pts',(38.9693587283608,-1.03043505637373,-6.63974724939573));
#39140=CARTESIAN_POINT('Ctrl Pts',(39.0686145305819,2.27464993583887,-6.34304533089632));
#39141=CARTESIAN_POINT('Ctrl Pts',(39.1678703328029,5.01509137070583,-4.47178918160662));
#39142=CARTESIAN_POINT('Ctrl Pts',(39.300211402431,7.09861927260105,-0.548013875149835));
#39143=CARTESIAN_POINT('Ctrl Pts',(39.4656377394661,5.49001932721968,5.30453959444752));
#39144=CARTESIAN_POINT('Ctrl Pts',(39.6641493439083,-1.49037074416326,7.48694413984165));
#39145=CARTESIAN_POINT('Ctrl Pts',(39.8626609483503,-7.09763510524872,2.81053614474318));
#39146=CARTESIAN_POINT('Ctrl Pts',(40.0611725527924,-6.20413338397556,-4.44827848455409));
#39147=CARTESIAN_POINT('Ctrl Pts',(40.2265988898275,-0.735553655790395,
-7.0816435665849));
#39148=CARTESIAN_POINT('Ctrl Pts',(40.3589399594556,3.49857308487482,-5.73655177881727));
#39149=CARTESIAN_POINT('Ctrl Pts',(40.4581957616766,5.83150027903981,-3.37666416689254));
#39150=CARTESIAN_POINT('Ctrl Pts',(40.5574515638978,6.71685569069011,-0.178576514989967));
#39151=CARTESIAN_POINT('Ctrl Pts',(40.6897926335258,5.77566097104865,4.16322652905234));
#39152=CARTESIAN_POINT('Ctrl Pts',(40.8552189705609,0.769479356240343,7.59515332581423));
#39153=CARTESIAN_POINT('Ctrl Pts',(41.053730575003,-5.9707946456355,4.75659003991491));
#39154=CARTESIAN_POINT('Ctrl Pts',(41.2522421794451,-7.23525339279788,-2.43447034284124));
#39155=CARTESIAN_POINT('Ctrl Pts',(41.4507537838872,-1.86759511254066,-7.40206329464434));
#39156=CARTESIAN_POINT('Ctrl Pts',(41.6161801209223,4.00902614733043,-5.88374235794879));
#39157=CARTESIAN_POINT('Ctrl Pts',(41.7485211905504,6.37487523671707,-2.12344193646858));
#39158=CARTESIAN_POINT('Ctrl Pts',(41.8477769927715,6.63358312000962,1.18483390833526));
#39159=CARTESIAN_POINT('Ctrl Pts',(41.9470327949925,5.24561565699268,4.19899467972695));
#39160=CARTESIAN_POINT('Ctrl Pts',(42.0793738646206,1.7243133381715,6.90778244420767));
#39161=CARTESIAN_POINT('Ctrl Pts',(42.2448002016556,-4.31455827790939,6.29785990546237));
#39162=CARTESIAN_POINT('Ctrl Pts',(42.4433118060978,-7.63064917983663,-0.220750090431982));
#39163=CARTESIAN_POINT('Ctrl Pts',(42.6418234105399,-3.95497920617077,-6.52944691278856));
#39164=CARTESIAN_POINT('Ctrl Pts',(42.840335014982,3.35118444795746,-6.8591555834574));
#39165=CARTESIAN_POINT('Ctrl Pts',(43.0057613520171,6.85976484305111,-1.90639478669554));
#39166=CARTESIAN_POINT('Ctrl Pts',(43.1381024216452,6.23972265263023,2.49276977667716));
#39167=CARTESIAN_POINT('Ctrl Pts',(43.2373582238662,4.30199909517582,5.18662319679422));
#39168=CARTESIAN_POINT('Ctrl Pts',(43.3366140260872,1.29637667797795,6.59298471483567));
#39169=CARTESIAN_POINT('Ctrl Pts',(43.4689550957154,-3.14159009001819,6.38914129527586));
#39170=CARTESIAN_POINT('Ctrl Pts',(43.6343814327504,-7.36042316718463,2.02549335281035));
#39171=CARTESIAN_POINT('Ctrl Pts',(43.8328930371926,-5.68582852314473,-5.09380913595719));
#39172=CARTESIAN_POINT('Ctrl Pts',(44.0314046416347,1.19360462082791,-7.53994996782506));
#39173=CARTESIAN_POINT('Ctrl Pts',(44.2299162460768,6.98688357126563,-3.07602186011172));
#39174=CARTESIAN_POINT('Ctrl Pts',(44.3953425831118,6.46998971585273,2.97152281859987));
#39175=CARTESIAN_POINT('Ctrl Pts',(44.52768365274,3.15696064319814,5.93141125184893));
#39176=CARTESIAN_POINT('Ctrl Pts',(44.626939454961,-0.0618247881750454,
6.7382812419774));
#39177=CARTESIAN_POINT('Ctrl Pts',(44.726195257182,-3.26526325658163,5.87248633940344));
#39178=CARTESIAN_POINT('Ctrl Pts',(44.8585363268102,-6.52342426137875,2.85230620564395));
#39179=CARTESIAN_POINT('Ctrl Pts',(45.0239626638452,-6.92926609411708,-3.20370471785814));
#39180=CARTESIAN_POINT('Ctrl Pts',(45.2224742682874,-1.05505487162644,-7.56058177166444));
#39181=CARTESIAN_POINT('Ctrl Pts',(45.4209858727294,5.77833642645426,-4.98862362289226));
#39182=CARTESIAN_POINT('Ctrl Pts',(45.6194974771717,7.32201870880574,2.16020706188214));
#39183=CARTESIAN_POINT('Ctrl Pts',(45.7849238142066,3.0238283147716,6.44570997699132));
#39184=CARTESIAN_POINT('Ctrl Pts',(45.9172648838347,-1.41713158479941,6.56808785055635));
#39185=CARTESIAN_POINT('Ctrl Pts',(46.0165206860558,-4.39644299388766,5.10681362513981));
#39186=CARTESIAN_POINT('Ctrl Pts',(46.1157764882768,-6.28441143515325,2.37785888037478));
#39187=CARTESIAN_POINT('Ctrl Pts',(46.248117557905,-6.82362998403564,-2.03194208226253));
#39188=CARTESIAN_POINT('Ctrl Pts',(46.41354389494,-3.22476320316531,-6.91949093545313));
#39189=CARTESIAN_POINT('Ctrl Pts',(46.6120554993822,4.07412068923817,-6.45577866083469));
#39190=CARTESIAN_POINT('Ctrl Pts',(46.8105671038242,7.63341503086778,-0.0806999051357613));
#39191=CARTESIAN_POINT('Ctrl Pts',(47.0090787082664,4.19827393130149,6.37596647733199));
#39192=CARTESIAN_POINT('Ctrl Pts',(47.1745050453014,-1.85077235155308,6.8749804717851));
#39193=CARTESIAN_POINT('Ctrl Pts',(47.3068461149295,-5.32177892736629,4.10203717553878));
#39194=CARTESIAN_POINT('Ctrl Pts',(47.4061019171506,-6.6542065815006,1.06291635189777));
#39195=CARTESIAN_POINT('Ctrl Pts',(47.5053577193716,-6.33483946216542,-2.24005556401035));
#39196=CARTESIAN_POINT('Ctrl Pts',(47.6376987889997,-3.90039178526545,-5.95631250910608));
#39197=CARTESIAN_POINT('Ctrl Pts',(47.8031251260348,2.00309944932168,-7.36654906441504));
#39198=CARTESIAN_POINT('Ctrl Pts',(48.0016367304768,7.27870485203315,-2.301302497534));
#39199=CARTESIAN_POINT('Ctrl Pts',(48.2001483349191,5.88251187212179,4.86534598795536));
#39200=CARTESIAN_POINT('Ctrl Pts',(48.3986599393611,-0.9087115283618,7.57975566100446));
#39201=CARTESIAN_POINT('Ctrl Pts',(48.5640862763962,-5.85107870524407,4.05654936734897));
#39202=CARTESIAN_POINT('Ctrl Pts',(48.6964273460243,-6.71244822969185,-0.301792486600593));
#39203=CARTESIAN_POINT('Ctrl Pts',(48.7956831482453,-5.76856089762008,-3.48309654917376));
#39204=CARTESIAN_POINT('Ctrl Pts',(48.8949389504664,-3.39272542501121,-5.79978052444612));
#39205=CARTESIAN_POINT('Ctrl Pts',(49.0272800200945,0.865369267295591,-7.06695484745162));
#39206=CARTESIAN_POINT('Ctrl Pts',(49.1927063571296,6.28470933619326,-4.33369139208969));
#39207=CARTESIAN_POINT('Ctrl Pts',(49.3912179615717,7.04487031890815,2.94029585210974));
#39208=CARTESIAN_POINT('Ctrl Pts',(49.5897295660138,1.3527436252517,7.51303016049503));
#39209=CARTESIAN_POINT('Ctrl Pts',(49.7882411704559,-5.58642684012997,5.20291146207417));
#39210=CARTESIAN_POINT('Ctrl Pts',(49.953667507491,-7.08736881972858,-0.678172542822872));
#39211=CARTESIAN_POINT('Ctrl Pts',(50.0860085771191,-4.93219523779632,-4.56305709777133));
#39212=CARTESIAN_POINT('Ctrl Pts',(50.1852643793401,-2.15787991664417,-6.38371448811436));
#39213=CARTESIAN_POINT('Ctrl Pts',(50.2845201815612,1.15209277018053,-6.61972221397241));
#39214=CARTESIAN_POINT('Ctrl Pts',(50.4168612511892,5.22233480911237,-4.83920798542831));
#39215=CARTESIAN_POINT('Ctrl Pts',(50.5822875882244,7.59745834475163,0.746377399222896));
#39216=CARTESIAN_POINT('Ctrl Pts',(50.7807991926665,3.48307919085419,6.79291519587912));
#39217=CARTESIAN_POINT('Ctrl Pts',(50.9793107971085,-3.8160530018601,6.61160169665124));
#39218=CARTESIAN_POINT('Ctrl Pts',(51.1778224015507,-7.62514594570818,0.368241536165105));
#39219=CARTESIAN_POINT('Ctrl Pts',(51.3432487385857,-4.97562628966537,-5.09252960818989));
#39220=CARTESIAN_POINT('Ctrl Pts',(51.4755898082139,-0.822001320650966,
-6.66875953758343));
#39221=CARTESIAN_POINT('Ctrl Pts',(51.5748456104349,2.47217124072609,-6.26870207913443));
#39222=CARTESIAN_POINT('Ctrl Pts',(51.674101412656,5.15266890569921,-4.31254485072359));
#39223=CARTESIAN_POINT('Ctrl Pts',(51.806442482284,7.11229914548942,-0.325446846305394));
#39224=CARTESIAN_POINT('Ctrl Pts',(51.9718688193191,5.32121132378008,5.47386176021844));
#39225=CARTESIAN_POINT('Ctrl Pts',(52.1703804237614,-1.72409869935947,7.43660010912471));
#39226=CARTESIAN_POINT('Ctrl Pts',(52.3688920282032,-7.18216793587477,2.58689026614183));
#39227=CARTESIAN_POINT('Ctrl Pts',(52.5674036326456,-6.06178955683664,-4.6403835930808));
#39228=CARTESIAN_POINT('Ctrl Pts',(52.7328299696805,-0.513426252932243,
-7.10120470536513));
#39229=CARTESIAN_POINT('Ctrl Pts',(52.8651710393087,3.67650133636693,-5.62417797237554));
#39230=CARTESIAN_POINT('Ctrl Pts',(52.9644268415297,5.93438279112921,-3.19239052886186));
#39231=CARTESIAN_POINT('Ctrl Pts',(53.0636826437508,6.71915361157393,0.0318541258702626));
#39232=CARTESIAN_POINT('Ctrl Pts',(53.1960237133788,5.64245389348959,4.34205352852127));
#39233=CARTESIAN_POINT('Ctrl Pts',(53.361450050414,0.531254395267008,7.61552501734556));
#39234=CARTESIAN_POINT('Ctrl Pts',(53.559961654856,-6.11682218841227,4.56727750673352));
#39235=CARTESIAN_POINT('Ctrl Pts',(53.7584732592982,-7.15546766306728,-2.65985338523861));
#39236=CARTESIAN_POINT('Ctrl Pts',(53.9569848637402,-1.63487832315821,-7.45691795521279));
#39237=CARTESIAN_POINT('Ctrl Pts',(54.1224112007754,4.19131342003372,-5.7553111644589));
#39238=CARTESIAN_POINT('Ctrl Pts',(54.2547522704034,6.43824571186064,-1.92276678122184));
#39239=CARTESIAN_POINT('Ctrl Pts',(54.3540080726245,6.59322572684469,1.39198811607388));
#39240=CARTESIAN_POINT('Ctrl Pts',(54.4532638748455,5.11154843903565,4.36120539491713));
#39241=CARTESIAN_POINT('Ctrl Pts',(54.5856049444738,1.50714557455112,6.95839255876029));
#39242=CARTESIAN_POINT('Ctrl Pts',(54.7510312815086,-4.50966408232794,6.15965765175859));
#39243=CARTESIAN_POINT('Ctrl Pts',(54.9495428859509,-7.61999373109382,-0.459600964161025));
#39244=CARTESIAN_POINT('Ctrl Pts',(55.1480544903929,-3.74856524016585,-6.65009745405187));
#39245=CARTESIAN_POINT('Ctrl Pts',(55.3465660948351,3.56434011436733,-6.75084676699293));
#39246=CARTESIAN_POINT('Ctrl Pts',(55.5119924318701,6.91610051670058,-1.69064142490175));
#39247=CARTESIAN_POINT('Ctrl Pts',(55.6443335014983,6.1585995000709,2.68694848089583));
#39248=CARTESIAN_POINT('Ctrl Pts',(55.7435893037193,4.13746639931955,5.31879950693002));
#39249=CARTESIAN_POINT('Ctrl Pts',(55.8428451059403,1.08927691098905,6.63034808682382));
#39250=CARTESIAN_POINT('Ctrl Pts',(55.9751861755685,-3.34012972565061,6.28762659518877));
#39251=CARTESIAN_POINT('Ctrl Pts',(56.1406125126035,-7.42024294481071,1.79400311100452));
#39252=CARTESIAN_POINT('Ctrl Pts',(56.3391241170456,-5.52352365615058,-5.26936655852601));
#39253=CARTESIAN_POINT('Ctrl Pts',(56.5376357214877,1.42913804177327,-7.49887337976339));
#39254=CARTESIAN_POINT('Ctrl Pts',(56.7361473259298,7.07978459251398,-2.85571403433688));
#39255=CARTESIAN_POINT('Ctrl Pts',(56.9015736629649,6.37376113923339,3.17267769001173));
#39256=CARTESIAN_POINT('Ctrl Pts',(57.0339147325929,2.96966597794152,6.02736459165353));
#39257=CARTESIAN_POINT('Ctrl Pts',(57.133170534814,-0.272808478755478,6.73304031878143));
#39258=CARTESIAN_POINT('Ctrl Pts',(57.2324263370351,-3.44756282279183,5.76735212416978));
#39259=CARTESIAN_POINT('Ctrl Pts',(57.3647674066631,-6.60954677648735,2.64662165677788));
#39260=CARTESIAN_POINT('Ctrl Pts',(57.5301937436982,-6.82554132287069,-3.41912827663594));
#39261=CARTESIAN_POINT('Ctrl Pts',(57.7287053481404,-0.817772480688494,
-7.58991341702892));
#39262=CARTESIAN_POINT('Ctrl Pts',(57.9272169525824,5.93172465642349,-4.80522425163951));
#39263=CARTESIAN_POINT('Ctrl Pts',(58.1257285570247,7.25077917183186,2.38844173544932));
#39264=CARTESIAN_POINT('Ctrl Pts',(58.2911548940596,2.82049331914008,6.53724194300516));
#39265=CARTESIAN_POINT('Ctrl Pts',(58.4234959636878,-1.62212083014546,6.52048801499322));
#39266=CARTESIAN_POINT('Ctrl Pts',(58.5227517659088,-4.55421018600847,4.96663125086556));
#39267=CARTESIAN_POINT('Ctrl Pts',(58.6220075681299,-6.35579352430296,2.17989188211036));
#39268=CARTESIAN_POINT('Ctrl Pts',(58.7543486377579,-6.75665159323421,-2.24463227107365));
#39269=CARTESIAN_POINT('Ctrl Pts',(58.9197749747931,-3.00649287392933,-7.01708294958232));
#39270=CARTESIAN_POINT('Ctrl Pts',(59.1182865792351,4.27428975474489,-6.32502842686495));
#39271=CARTESIAN_POINT('Ctrl Pts',(59.3167981836773,7.6321983440743,0.158385431391267));
#39272=CARTESIAN_POINT('Ctrl Pts',(59.5153097881193,3.99654698742823,6.50431123944617));
#39273=CARTESIAN_POINT('Ctrl Pts',(59.6807361251545,-2.06515947292264,6.81365035323193));
#39274=CARTESIAN_POINT('Ctrl Pts',(59.8130771947826,-5.44762700138892,3.9333700556902));
#39275=CARTESIAN_POINT('Ctrl Pts',(59.9123329970036,-6.68422895260743,0.854013881352277));
#39276=CARTESIAN_POINT('Ctrl Pts',(60.0115887992247,-6.26158358209626,-2.43733686339917));
#39277=CARTESIAN_POINT('Ctrl Pts',(60.1439298688528,-3.71195269870614,-6.07553470463859));
#39278=CARTESIAN_POINT('Ctrl Pts',(60.3093562058878,2.23280567678422,-7.30020762252876));
#39279=CARTESIAN_POINT('Ctrl Pts',(60.50786781033,7.34720186618502,-2.07223604970431));
#39280=CARTESIAN_POINT('Ctrl Pts',(60.706379414772,5.72726502447374,5.04717473915921));
#39281=CARTESIAN_POINT('Ctrl Pts',(60.9048910192142,-1.14563122034757,7.54758117738868));
#39282=CARTESIAN_POINT('Ctrl Pts',(61.0703173562493,-5.97524269785684,3.87132916275642));
#39283=CARTESIAN_POINT('Ctrl Pts',(61.2026584258773,-6.69970521934169,-0.511849504432479));
#39284=CARTESIAN_POINT('Ctrl Pts',(61.3019142280984,-5.65665605067822,-3.66203477929179));
#39285=CARTESIAN_POINT('Ctrl Pts',(61.4011700303195,-3.20943723603463,-5.90318156329419));
#39286=CARTESIAN_POINT('Ctrl Pts',(61.5335110999475,1.08625149890279,-7.03638916389873));
#39287=CARTESIAN_POINT('Ctrl Pts',(61.6989374369826,6.4173395489619,-4.1347558133022));
#39288=CARTESIAN_POINT('Ctrl Pts',(61.8974490414248,6.94933768253574,3.15946882913184));
#39289=CARTESIAN_POINT('Ctrl Pts',(62.0959606458668,1.11680434293635,7.55170746042015));
#39290=CARTESIAN_POINT('Ctrl Pts',(62.2944722503089,-5.74661976777159,5.025416775449));
#39291=CARTESIAN_POINT('Ctrl Pts',(62.4598985873441,-7.06265532099699,-0.899785864244022));
#39292=CARTESIAN_POINT('Ctrl Pts',(62.5922396569721,-4.78688086854931,-4.71527427532892));
#39293=CARTESIAN_POINT('Ctrl Pts',(62.6914954591932,-1.95691106368252,-6.44815907753943));
#39294=CARTESIAN_POINT('Ctrl Pts',(62.7907512614142,1.35882897202167,-6.58039693073728));
#39295=CARTESIAN_POINT('Ctrl Pts',(62.9230923310424,5.37131667820771,-4.67329347752821));
#39296=CARTESIAN_POINT('Ctrl Pts',(63.0885186680773,7.57035878608015,0.983931081085398));
#39297=CARTESIAN_POINT('Ctrl Pts',(63.2870302725196,3.26864597700691,6.89865863665999));
#39298=CARTESIAN_POINT('Ctrl Pts',(63.4855418769615,-4.02122834632787,6.48885660920751));
#39299=CARTESIAN_POINT('Ctrl Pts',(63.6840534814038,-7.63293788281372,0.129274125075791));
#39300=CARTESIAN_POINT('Ctrl Pts',(63.8494798184388,-4.81370981556546,-5.24584717621744));
#39301=CARTESIAN_POINT('Ctrl Pts',(63.9818208880669,-0.612761272495992,
-6.6912303475662));
#39302=CARTESIAN_POINT('Ctrl Pts',(64.0810766902879,2.66726755874743,-6.18820977104621));
#39303=CARTESIAN_POINT('Ctrl Pts',(64.180332492509,5.28519211669809,-4.14907028511851));
#39304=CARTESIAN_POINT('Ctrl Pts',(64.3126735621372,7.11900246605432,-0.102560582161132));
#39305=CARTESIAN_POINT('Ctrl Pts',(64.4780998991721,5.14718367076357,5.63781453949438));
#39306=CARTESIAN_POINT('Ctrl Pts',(64.6766115036143,-1.95613546236265,7.37896141479572));
#39307=CARTESIAN_POINT('Ctrl Pts',(64.8751231080564,-7.25965567891763,2.36070687120159));
#39308=CARTESIAN_POINT('Ctrl Pts',(65.0736347124985,-5.91349963671721,-4.82793688534368));
#39309=CARTESIAN_POINT('Ctrl Pts',(65.2390610495336,-0.290795223183368,
-7.11380017450725));
#39310=CARTESIAN_POINT('Ctrl Pts',(65.3714021191617,3.8508232569948,-5.50628733219841));
#39311=CARTESIAN_POINT('Ctrl Pts',(65.4706579213827,6.03144418528739,-3.00498543092064));
#39312=CARTESIAN_POINT('Ctrl Pts',(65.5699137236038,6.71486062202045,0.242253520557295));
#39313=CARTESIAN_POINT('Ctrl Pts',(65.7022547932319,5.50371205506531,4.51662134784635));
#39314=CARTESIAN_POINT('Ctrl Pts',(65.8676811302669,0.292508319573518,7.62842653525906));
#39315=CARTESIAN_POINT('Ctrl Pts',(66.0661927347091,-6.25684965601425,4.37348486821448));
#39316=CARTESIAN_POINT('Ctrl Pts',(66.2647043391512,-7.06866303628636,-2.88262734106105));
#39317=CARTESIAN_POINT('Ctrl Pts',(66.4632159435933,-1.40055785934149,-7.50445802153318));
#39318=CARTESIAN_POINT('Ctrl Pts',(66.6286422806284,4.36948937605636,-5.62123450789267));
#39319=CARTESIAN_POINT('Ctrl Pts',(66.7609833502565,6.49530082234867,-1.72020555609331));
#39320=CARTESIAN_POINT('Ctrl Pts',(66.8602391524775,6.54640094903262,1.59777690035313));
#39321=CARTESIAN_POINT('Ctrl Pts',(66.9594949546986,4.97246723013121,4.51913814934136));
#39322=CARTESIAN_POINT('Ctrl Pts',(67.0918360243266,1.28849943663799,7.00217707764802));
#39323=CARTESIAN_POINT('Ctrl Pts',(67.2572623613617,-4.70034630644326,6.01541333026384));
#39324=CARTESIAN_POINT('Ctrl Pts',(67.4557739658039,-7.60186370645468,-0.698001051142927));
#39325=CARTESIAN_POINT('Ctrl Pts',(67.654285570246,-3.53847428970454,-6.76422474536313));
#39326=CARTESIAN_POINT('Ctrl Pts',(67.852797174688,3.77399953920919,-6.63591610496366));
#39327=CARTESIAN_POINT('Ctrl Pts',(68.0182235117233,6.96565197102557,-1.47322942045928));
#39328=CARTESIAN_POINT('Ctrl Pts',(68.1505645813511,6.07143546137237,2.87849114407054));
#39329=CARTESIAN_POINT('Ctrl Pts',(68.2498203835724,3.96887483637101,5.44575935501849));
#39330=CARTESIAN_POINT('Ctrl Pts',(68.3490761857933,0.881109338758424,6.66120614223146));
#39331=CARTESIAN_POINT('Ctrl Pts',(68.4814172554215,-3.53539445446629,6.17994755252381));
#39332=CARTESIAN_POINT('Ctrl Pts',(68.6468435924565,-7.47278110162834,1.56074642543637));
#39333=CARTESIAN_POINT('Ctrl Pts',(68.8453551968986,-5.35580568311857,-5.43974407142979));
#39334=CARTESIAN_POINT('Ctrl Pts',(69.0438668013406,1.6632787956131,-7.45046150502356));
#39335=CARTESIAN_POINT('Ctrl Pts',(69.242378405783,7.16572282166079,-2.63256464231793));
#39336=CARTESIAN_POINT('Ctrl Pts',(69.4078047428178,6.27131232510135,3.37064950491412));
#39337=CARTESIAN_POINT('Ctrl Pts',(69.5401458124461,2.77941377570154,6.11750475464112));
#39338=CARTESIAN_POINT('Ctrl Pts',(69.639401614667,-0.483427260097334,6.72097830381911));
#39339=CARTESIAN_POINT('Ctrl Pts',(69.7386574168881,-3.62666022552501,5.6569603321232));
#39340=CARTESIAN_POINT('Ctrl Pts',(69.8709984865162,-6.68879787400515,2.43747746055645));
#39341=CARTESIAN_POINT('Ctrl Pts',(70.0364248235513,-6.71591205222224,-3.62943820858347));
#39342=CARTESIAN_POINT('Ctrl Pts',(70.2349364279934,-0.57837423373233,-7.61472297301591));
#39343=CARTESIAN_POINT('Ctrl Pts',(70.4334480324355,6.07689073543469,-4.61176722374836));
#39344=CARTESIAN_POINT('Ctrl Pts',(70.6319596368776,7.17705138752177,2.60408556382735));
#39345=CARTESIAN_POINT('Ctrl Pts',(70.8304712413198,1.69293223737595,7.44540855735987));
#39346=CARTESIAN_POINT('Ctrl Pts',(70.9958975783548,-4.15224483306629,5.78576453575111));
#39347=CARTESIAN_POINT('Ctrl Pts',(71.128238647983,-6.41601391396102,1.9731352289123));
#39348=CARTESIAN_POINT('Ctrl Pts',(71.2605797176109,-6.68463811960246,-2.44961921254678));
#39349=CARTESIAN_POINT('Ctrl Pts',(71.4260060546462,-2.78893611703176,-7.11224532601399));
#39350=CARTESIAN_POINT('Ctrl Pts',(71.6245176590881,4.47967320795655,-6.18354439128806));
#39351=CARTESIAN_POINT('Ctrl Pts',(71.7899439961234,7.08222387658641,-0.70626625924099));
#39352=CARTESIAN_POINT('Ctrl Pts',(71.9222850657513,5.72278531268991,3.52328110221862));
#39353=CARTESIAN_POINT('Ctrl Pts',(72.0215408679725,3.35124036184121,5.84559059835005));
#39354=CARTESIAN_POINT('Ctrl Pts',(72.1207966701934,0.150326486829087,6.71764568719649));
#39355=CARTESIAN_POINT('Ctrl Pts',(72.2531377398217,-4.18792723744534,5.75785783169036));
#39356=CARTESIAN_POINT('Ctrl Pts',(72.4185640768566,-7.59823771737176,0.737245998958156));
#39357=CARTESIAN_POINT('Ctrl Pts',(72.6170756812988,-4.73124216678028,-5.99096554247927));
#39358=CARTESIAN_POINT('Ctrl Pts',(72.8155872857409,2.46521529949203,-7.22483627642068));
#39359=CARTESIAN_POINT('Ctrl Pts',(73.014098890183,7.40991079793194,-1.83614083239068));
#39360=CARTESIAN_POINT('Ctrl Pts',(73.1795252272181,5.86666851215432,4.03398688832659));
#39361=CARTESIAN_POINT('Ctrl Pts',(73.3118662968462,2.09633824391537,6.38383659653893));
#39362=CARTESIAN_POINT('Ctrl Pts',(73.4111220990671,-1.21300002147258,6.62849090958169));
#39363=CARTESIAN_POINT('Ctrl Pts',(73.5103779012884,-4.22124101151322,5.22773083917127));
#39364=CARTESIAN_POINT('Ctrl Pts',(73.6427189709162,-6.91504415087427,1.6949540826346));
#39365=CARTESIAN_POINT('Ctrl Pts',(73.8081453079515,-6.27947547325658,-4.34127251565845));
#39366=CARTESIAN_POINT('Ctrl Pts',(74.0066569123935,0.253162974219424,-7.62964252307557));
#39367=CARTESIAN_POINT('Ctrl Pts',(74.2051685168357,6.54618845205212,-3.92720676581047));
#39368=CARTESIAN_POINT('Ctrl Pts',(74.4036801212777,6.84485808874247,3.38029161791993));
#39369=CARTESIAN_POINT('Ctrl Pts',(74.5691064583128,1.87723757943772,6.86780121746246));
#39370=CARTESIAN_POINT('Ctrl Pts',(74.7014475279409,-2.51925332864382,6.22907718612626));
#39371=CARTESIAN_POINT('Ctrl Pts',(74.8007033301619,-5.20485110658452,4.27992773619665));
#39372=CARTESIAN_POINT('Ctrl Pts',(74.8999591323831,-6.5984321743934,1.26835828159773));
#39373=CARTESIAN_POINT('Ctrl Pts',(75.0323002020111,-6.37573831885696,-3.16870252903819));
#39374=CARTESIAN_POINT('Ctrl Pts',(75.1977265390462,-1.99420833105789,-7.36896096068155));
#39375=CARTESIAN_POINT('Ctrl Pts',(75.3962381434883,5.11791631823011,-5.66413895152702));
#39376=CARTESIAN_POINT('Ctrl Pts',(75.5947497479304,7.53481155985735,1.22562321815919));
#39377=CARTESIAN_POINT('Ctrl Pts',(75.7932613523725,3.04631414056803,6.99988733311835));
#39378=CARTESIAN_POINT('Ctrl Pts',(75.9586876894077,-2.9989802314213,6.45730844516487));
#39379=CARTESIAN_POINT('Ctrl Pts',(76.0910287590357,-5.94476836125033,3.13173579232941));
#39380=CARTESIAN_POINT('Ctrl Pts',(76.1902845612568,-6.73795781621743,-0.0904481444383849));
#39381=CARTESIAN_POINT('Ctrl Pts',(76.2895403634778,-5.85856266362047,-3.29017985190923));
#39382=CARTESIAN_POINT('Ctrl Pts',(76.4218814331059,-2.82456925905874,-6.53548187093887));
#39383=CARTESIAN_POINT('Ctrl Pts',(76.587307770141,3.23311102121609,-6.91559438130846));
#39384=CARTESIAN_POINT('Ctrl Pts',(76.7858193745831,7.56499538095572,-1.02292834271609));
#39385=CARTESIAN_POINT('Ctrl Pts',(76.9843309790252,4.96403250061669,5.79947573845812));
#39386=CARTESIAN_POINT('Ctrl Pts',(77.1828425834674,-2.19129117565982,7.31277618321408));
#39387=CARTESIAN_POINT('Ctrl Pts',(77.3482689205024,-6.45849690590605,2.99641994738856));
#39388=CARTESIAN_POINT('Ctrl Pts',(77.4806099901305,-6.56200867841511,-1.44501973884905));
#39389=CARTESIAN_POINT('Ctrl Pts',(77.5798657923516,-5.08809165731427,-4.41809683995133));
#39390=CARTESIAN_POINT('Ctrl Pts',(77.6791215945725,-2.35114153022991,-6.2944557704451));
#39391=CARTESIAN_POINT('Ctrl Pts',(77.8114626642008,2.06091022055313,-6.81493681904093));
#39392=CARTESIAN_POINT('Ctrl Pts',(77.9768890012357,6.93312715195307,-3.19534042273405));
#39393=CARTESIAN_POINT('Ctrl Pts',(78.1754006056779,6.43841373241497,4.10150778597543));
#39394=CARTESIAN_POINT('Ctrl Pts',(78.3739122101199,0.0482727750496181,
7.63368896716102));
#39395=CARTESIAN_POINT('Ctrl Pts',(78.5724238145622,-6.39374302739908,4.17115123459849));
#39396=CARTESIAN_POINT('Ctrl Pts',(78.7378501515971,-6.86705644430124,-1.87996025901627));
#39397=CARTESIAN_POINT('Ctrl Pts',(78.8701912212254,-4.07939348819663,-5.33915617955881));
#39398=CARTESIAN_POINT('Ctrl Pts',(78.9694470234462,-1.0346399928902,-6.6586617638629));
#39399=CARTESIAN_POINT('Ctrl Pts',(79.0687028256675,2.26694546453617,-6.32526665067021));
#39400=CARTESIAN_POINT('Ctrl Pts',(79.2010438952954,5.97282745565348,-3.87505444731962));
#39401=CARTESIAN_POINT('Ctrl Pts',(79.3664702323306,7.35797352307912,2.03437414355709));
#39402=CARTESIAN_POINT('Ctrl Pts',(79.5649818367726,2.27036212464169,7.28841500815914));
#39403=CARTESIAN_POINT('Ctrl Pts',(79.7634934412148,-4.89029073438004,5.86179102675996));
#39404=CARTESIAN_POINT('Ctrl Pts',(79.9620050456568,-7.57582710640418,-0.940901788806087));
#39405=CARTESIAN_POINT('Ctrl Pts',(80.127431382692,-4.03165764889719,-5.86825795162323));
#39406=CARTESIAN_POINT('Ctrl Pts',(80.25977245232,0.330303940273858,-6.71110566511225));
#39407=CARTESIAN_POINT('Ctrl Pts',(80.3590282545411,3.50756970849505,-5.75371281352009));
#39408=CARTESIAN_POINT('Ctrl Pts',(80.4582840567622,5.81414033957109,-3.36805760833066));
#39409=CARTESIAN_POINT('Ctrl Pts',(80.5906251263901,7.06321503561394,0.895381564126428));
#39410=CARTESIAN_POINT('Ctrl Pts',(80.7560514634254,4.30695512977908,6.30306195688861));
#39411=CARTESIAN_POINT('Ctrl Pts',(80.9545630678673,-2.9701956136278,7.03231651200037));
#39412=CARTESIAN_POINT('Ctrl Pts',(81.1530746723096,-7.51870876718994,1.32081640751017));
#39413=CARTESIAN_POINT('Ctrl Pts',(81.3515862767517,-5.17913362961361,-5.60847816871138));
#39414=CARTESIAN_POINT('Ctrl Pts',(81.5170126137868,0.70827324628638,-7.08442402692663));
#39415=CARTESIAN_POINT('Ctrl Pts',(81.6493536834148,4.58396766952698,-4.91276707630163));
#39416=CARTESIAN_POINT('Ctrl Pts',(81.7486094856359,6.39282346674118,-2.13074271640208));
#39417=CARTESIAN_POINT('Ctrl Pts',(81.8478652878569,6.61476844885798,1.18020265601094));
#39418=CARTESIAN_POINT('Ctrl Pts',(81.980206357485,4.81698008100702,5.24284442682424));
#39419=CARTESIAN_POINT('Ctrl Pts',(82.1456326945201,-0.77864432454375,7.59421921846892));
#39420=CARTESIAN_POINT('Ctrl Pts',(82.3441442989622,-6.80764986905927,3.45419176776045));
#39421=CARTESIAN_POINT('Ctrl Pts',(82.5426559034044,-6.59533162217188,-3.84410435625081));
#39422=CARTESIAN_POINT('Ctrl Pts',(82.7411675078464,-0.33584693840556,-7.62664142045963));
#39423=CARTESIAN_POINT('Ctrl Pts',(82.9065938448816,5.11361989587141,-4.95394856102158));
#39424=CARTESIAN_POINT('Ctrl Pts',(83.0389349145096,6.67219119247864,-0.793665315024038));
#39425=CARTESIAN_POINT('Ctrl Pts',(83.1381907167307,6.25814384746915,2.4987780983516));
#39426=CARTESIAN_POINT('Ctrl Pts',(83.2374465189517,4.29061763578174,5.17094191079159));
#39427=CARTESIAN_POINT('Ctrl Pts',(83.3697875885797,0.295231184688071,7.11361745754488));
#39428=CARTESIAN_POINT('Ctrl Pts',(83.5352139256149,-5.49641663689415,5.29791059531774));
#39429=CARTESIAN_POINT('Ctrl Pts',(83.7337255300571,-7.42920911831907,-1.75567348457842));
#39430=CARTESIAN_POINT('Ctrl Pts',(83.9322371344991,-2.55635740096063,-7.19309212694518));
#39431=CARTESIAN_POINT('Ctrl Pts',(84.1307487389412,4.6660919327514,-6.04202272400717));
#39432=CARTESIAN_POINT('Ctrl Pts',(84.2961750759763,7.10332164554252,-0.483256023931992));
#39433=CARTESIAN_POINT('Ctrl Pts',(84.4285161456044,5.60850961619246,3.70035941853477));
#39434=CARTESIAN_POINT('Ctrl Pts',(84.5277719478254,3.16715273537929,5.94789037820946));
#39435=CARTESIAN_POINT('Ctrl Pts',(84.6270277500466,-0.0603964992484957,
6.71895767244744));
#39436=CARTESIAN_POINT('Ctrl Pts',(84.7593688196744,-4.3659832409641,5.62395813678596));
#39437=CARTESIAN_POINT('Ctrl Pts',(84.9247951567098,-7.61771305015897,0.498899195976315));
#39438=CARTESIAN_POINT('Ctrl Pts',(85.1233067611518,-4.54125231388254,-6.1361685871416));
#39439=CARTESIAN_POINT('Ctrl Pts',(85.3218183655939,2.69022548959542,-7.14410416520489));
#39440=CARTESIAN_POINT('Ctrl Pts',(85.5203299700359,7.46379556362782,-1.60318692193913));
#39441=CARTESIAN_POINT('Ctrl Pts',(85.6857563070712,5.73745472665523,4.2157239051296));
#39442=CARTESIAN_POINT('Ctrl Pts',(85.8180973766991,1.89540005613835,6.44635544850367));
#39443=CARTESIAN_POINT('Ctrl Pts',(85.9173531789203,-1.41998328154509,6.58725313621316));
#39444=CARTESIAN_POINT('Ctrl Pts',(86.0166089811413,-4.38287967219087,5.09297611621711));
#39445=CARTESIAN_POINT('Ctrl Pts',(86.1489500507694,-6.9647320622293,1.47757303916075));
#39446=CARTESIAN_POINT('Ctrl Pts',(86.3143763878045,-6.14044522647656,-4.53578934067139));
#39447=CARTESIAN_POINT('Ctrl Pts',(86.5128879922466,0.491966206253473,-7.61797261481501));
#39448=CARTESIAN_POINT('Ctrl Pts',(86.7113995966886,6.66596118855492,-3.72028210500849));
#39449=CARTESIAN_POINT('Ctrl Pts',(86.9099112011309,6.73564470112767,3.59298524662677));
#39450=CARTESIAN_POINT('Ctrl Pts',(87.0753375381658,1.66124688858446,6.92321988383066));
#39451=CARTESIAN_POINT('Ctrl Pts',(87.207678607794,-2.71308568989366,6.14712989781052));
#39452=CARTESIAN_POINT('Ctrl Pts',(87.306934410015,-5.33632728774559,4.11483504875706));
#39453=CARTESIAN_POINT('Ctrl Pts',(87.4061902122361,-6.63491546291512,1.06110166394744));
#39454=CARTESIAN_POINT('Ctrl Pts',(87.5385312818642,-6.27338114436937,-3.36680914252208));
#39455=CARTESIAN_POINT('Ctrl Pts',(87.7039576188991,-1.76246606785234,-7.42779683903485));
#39456=CARTESIAN_POINT('Ctrl Pts',(87.9024692233414,5.29278269392219,-5.50108978867694));
#39457=CARTESIAN_POINT('Ctrl Pts',(88.1009808277834,7.49273480662979,1.46098002234296));
#39458=CARTESIAN_POINT('Ctrl Pts',(88.2994924322256,2.82561366348029,7.09185165856283));
#39459=CARTESIAN_POINT('Ctrl Pts',(88.4649187692607,-3.19972451338524,6.36022623993376));
#39460=CARTESIAN_POINT('Ctrl Pts',(88.5972598388888,-6.03992521597272,2.94403521152833));
#39461=CARTESIAN_POINT('Ctrl Pts',(88.6965156411097,-6.73182069116263,-0.301407668203426));
#39462=CARTESIAN_POINT('Ctrl Pts',(88.7957714433308,-5.75265499663935,-3.47203116790483));
#39463=CARTESIAN_POINT('Ctrl Pts',(88.928112512959,-2.61852072146245,-6.6207298703369));
#39464=CARTESIAN_POINT('Ctrl Pts',(89.0935388499939,3.44809201818041,-6.81095543638831));
#39465=CARTESIAN_POINT('Ctrl Pts',(89.2920504544363,7.59331879679955,-0.785523493179886));
#39466=CARTESIAN_POINT('Ctrl Pts',(89.4905620588782,4.77998319783827,5.9520835122292));
#39467=CARTESIAN_POINT('Ctrl Pts',(89.6890736633205,-2.41922116762525,7.24056775843034));
#39468=CARTESIAN_POINT('Ctrl Pts',(89.8545000003553,-6.54916428819377,2.792697962714));
#39469=CARTESIAN_POINT('Ctrl Pts',(89.9868410699836,-6.5135384872794,-1.64980493270938));
#39470=CARTESIAN_POINT('Ctrl Pts',(90.0860968722044,-4.94724035994962,-4.57526712021312));
#39471=CARTESIAN_POINT('Ctrl Pts',(90.1853526744257,-2.15287309025503,-6.3649962606837));
#39472=CARTESIAN_POINT('Ctrl Pts',(90.3176937440536,2.27331396916941,-6.7470555342519));
#39473=CARTESIAN_POINT('Ctrl Pts',(90.4831200810889,7.0297910830573,-2.97665749640009));
#39474=CARTESIAN_POINT('Ctrl Pts',(90.6816316855308,6.3068143690113,4.30111962435357));
#39475=CARTESIAN_POINT('Ctrl Pts',(90.8801432899731,-0.190805235875399,
7.63145666764416));
#39476=CARTESIAN_POINT('Ctrl Pts',(91.078654894415,-6.52122970457174,3.96888090807952));
#39477=CARTESIAN_POINT('Ctrl Pts',(91.2440812314504,-6.80481617230556,-2.09408491848547));
#39478=CARTESIAN_POINT('Ctrl Pts',(91.3764223010781,-3.91019329323491,-5.46428662780449));
#39479=CARTESIAN_POINT('Ctrl Pts',(91.4756781032995,-0.825611873513067,
-6.68779645583891));
#39480=CARTESIAN_POINT('Ctrl Pts',(91.5749339055203,2.46391379626772,-6.25117338951843));
#39481=CARTESIAN_POINT('Ctrl Pts',(91.7072749751485,6.09124809477092,-3.68611061047414));
#39482=CARTESIAN_POINT('Ctrl Pts',(91.8727013121836,7.29065689809534,2.26379648302618));
#39483=CARTESIAN_POINT('Ctrl Pts',(92.0712129166257,2.04100677136742,7.35593834037501));
#39484=CARTESIAN_POINT('Ctrl Pts',(92.2697245210678,-5.07145836342535,5.70577317952703));
#39485=CARTESIAN_POINT('Ctrl Pts',(92.4682361255099,-7.54264648894489,-1.17768266740843));
#39486=CARTESIAN_POINT('Ctrl Pts',(92.633662462545,-3.84591167244496,-5.99163401689822));
#39487=CARTESIAN_POINT('Ctrl Pts',(92.7660035321731,0.5403049311133,-6.69747045702155));
#39488=CARTESIAN_POINT('Ctrl Pts',(92.8652593343941,3.68603095739406,-5.64104885473879));
#39489=CARTESIAN_POINT('Ctrl Pts',(92.9645151366152,5.9167618455322,-3.18433183015161));
#39490=CARTESIAN_POINT('Ctrl Pts',(93.0968562062433,7.03171133010858,1.11613196115961));
#39491=CARTESIAN_POINT('Ctrl Pts',(93.2622825432784,4.10745793875989,6.43484590364255));
#39492=CARTESIAN_POINT('Ctrl Pts',(93.4607941477204,-3.1889607948191,6.93585370068267));
#39493=CARTESIAN_POINT('Ctrl Pts',(93.6593057521627,-7.55638345874021,1.0847149545591));
#39494=CARTESIAN_POINT('Ctrl Pts',(93.8578173566046,-5.0009600521374,-5.76791566159161));
#39495=CARTESIAN_POINT('Ctrl Pts',(94.0232436936399,0.929779586353665,-7.05876934780418));
#39496=CARTESIAN_POINT('Ctrl Pts',(94.1555847632678,4.73556618481844,-4.76680740647929));
#39497=CARTESIAN_POINT('Ctrl Pts',(94.254840565489,6.45641376810642,-1.92950191899969));
#39498=CARTESIAN_POINT('Ctrl Pts',(94.35409636771,6.57456531439976,1.38676994052863));
#39499=CARTESIAN_POINT('Ctrl Pts',(94.4864374373379,4.65043420184241,5.39112015438664));
#39500=CARTESIAN_POINT('Ctrl Pts',(94.6518637743732,-1.01608074535405,7.56611078700463));
#39501=CARTESIAN_POINT('Ctrl Pts',(94.8503753788152,-6.91248145316082,3.23931129530254));
#39502=CARTESIAN_POINT('Ctrl Pts',(95.0488869832573,-6.47171606662027,-4.04875643392091));
#39503=CARTESIAN_POINT('Ctrl Pts',(95.2473985876995,-0.0968485836272764,
-7.63341816450247));
#39504=CARTESIAN_POINT('Ctrl Pts',(95.4128249247347,5.2662482667137,-4.79138226173144));
#39505=CARTESIAN_POINT('Ctrl Pts',(95.5451659943625,6.69377295745098,-0.5843316997734));
#39506=CARTESIAN_POINT('Ctrl Pts',(95.6444217965838,6.17682350529167,2.69353072841089));
#39507=CARTESIAN_POINT('Ctrl Pts',(95.7436775988047,4.12658159253324,5.302769493522));
#39508=CARTESIAN_POINT('Ctrl Pts',(95.8760186684327,0.0723184561547882,
7.11937390685444));
#39509=CARTESIAN_POINT('Ctrl Pts',(96.0414450054678,-5.65962867528661,5.12318804848898));
#39510=CARTESIAN_POINT('Ctrl Pts',(96.2399566099102,-7.37058526236216,-1.98746330743906));
#39511=CARTESIAN_POINT('Ctrl Pts',(96.438468214352,-2.32984688235236,-7.26961835401006));
#39512=CARTESIAN_POINT('Ctrl Pts',(96.6369798187944,4.85301360391685,-5.89293742394273));
#39513=CARTESIAN_POINT('Ctrl Pts',(96.8024061558294,7.11497127449493,-0.260573497908623));
#39514=CARTESIAN_POINT('Ctrl Pts',(96.9347472254574,5.4898795280518,3.87417897221335));
#39515=CARTESIAN_POINT('Ctrl Pts',(97.0340030276785,2.97933701591658,6.04415480824299));
#39516=CARTESIAN_POINT('Ctrl Pts',(97.1332588298996,-0.270775759182261,
6.71377095450099));
#39517=CARTESIAN_POINT('Ctrl Pts',(97.2655998995276,-4.53996011612904,5.48447599399042));
#39518=CARTESIAN_POINT('Ctrl Pts',(97.4310262365626,-7.62960026922674,0.26010046928489));
#39519=CARTESIAN_POINT('Ctrl Pts',(97.6295378410049,-4.34686659336538,-6.27537156889143));
#39520=CARTESIAN_POINT('Ctrl Pts',(97.8280494454467,2.91262869299278,-7.05635398806792));
#39521=CARTESIAN_POINT('Ctrl Pts',(98.0265610498892,7.51033981885591,-1.36866662398636));
#39522=CARTESIAN_POINT('Ctrl Pts',(98.1919873869241,5.60262239538359,4.39332870150253));
#39523=CARTESIAN_POINT('Ctrl Pts',(98.3243284565523,1.6925982925338,6.50254957392664));
#39524=CARTESIAN_POINT('Ctrl Pts',(98.4235842587731,-1.62557130264698,6.53955459801569));
#39525=CARTESIAN_POINT('Ctrl Pts',(98.5228400609944,-4.54022018521893,4.95322527359627));
#39526=CARTESIAN_POINT('Ctrl Pts',(98.6551811306222,-7.00758739956846,1.25874287370734));
#39527=CARTESIAN_POINT('Ctrl Pts',(98.8206074676577,-5.9953921716689,-4.72585708948102));
#39528=CARTESIAN_POINT('Ctrl Pts',(99.0191190720994,0.730287084624933,-7.59883006009458));
#39529=CARTESIAN_POINT('Ctrl Pts',(99.217630676542,6.77919507077474,-3.50970820732301));
#39530=CARTESIAN_POINT('Ctrl Pts',(99.4161422809837,6.61982429947142,3.80215449007985));
#39531=CARTESIAN_POINT('Ctrl Pts',(99.581568618019,1.44362662206756,6.9718474567906));
#39532=CARTESIAN_POINT('Ctrl Pts',(99.7139096876469,-2.90425673145911,6.0591528103388));
#39533=CARTESIAN_POINT('Ctrl Pts',(99.8131654898681,-5.46256900081922,3.94570605997287));
#39534=CARTESIAN_POINT('Ctrl Pts',(99.9124212920891,-6.6648904672555,0.85280419836499));
#39535=CARTESIAN_POINT('Ctrl Pts',(100.044762361717,-6.16487032672607,-3.5616132074317));
#39536=CARTESIAN_POINT('Ctrl Pts',(100.210188698752,-1.52899497570559,-7.4793466884865));
#39537=CARTESIAN_POINT('Ctrl Pts',(100.408700303195,5.46245730522718,-5.33264453125622));
#39538=CARTESIAN_POINT('Ctrl Pts',(100.607211907636,7.44330832695098,1.69490373122168));
#39539=CARTESIAN_POINT('Ctrl Pts',(100.805723512079,2.60214150270374,7.17685948881637));
#39540=CARTESIAN_POINT('Ctrl Pts',(100.971149849114,-3.39733014130829,6.25690520110843));
#39541=CARTESIAN_POINT('Ctrl Pts',(101.103490918742,-6.12915742481166,2.75344678596453));
#39542=CARTESIAN_POINT('Ctrl Pts',(101.202746720963,-6.71908023031374,-0.512071537018741));
#39543=CARTESIAN_POINT('Ctrl Pts',(101.302002523184,-5.64110447104782,-3.65047672064705));
#39544=CARTESIAN_POINT('Ctrl Pts',(101.434343592812,-2.40990364076523,-6.69948350448945));
#39545=CARTESIAN_POINT('Ctrl Pts',(101.599769929847,3.65969073412208,-6.69963553134705));
#39546=CARTESIAN_POINT('Ctrl Pts',(101.798281534289,7.6141938215129,-0.547348112814414));
#39547=CARTESIAN_POINT('Ctrl Pts',(101.996793138732,4.59124514361469,6.09885280519223));
#39548=CARTESIAN_POINT('Ctrl Pts',(102.195304743173,-2.6447781121808,7.16125696087193));
#39549=CARTESIAN_POINT('Ctrl Pts',(102.360731080209,-6.63340750490673,2.58623658209116));
#39550=CARTESIAN_POINT('Ctrl Pts',(102.493072149836,-6.45867907640749,-1.85297181015727));
#39551=CARTESIAN_POINT('Ctrl Pts',(102.592327952058,-4.80153624628457,-4.72794945785535));
#39552=CARTESIAN_POINT('Ctrl Pts',(102.691583754279,-1.95249286737386,-6.42929323830486));
#39553=CARTESIAN_POINT('Ctrl Pts',(102.823924823907,2.48348779276022,-6.67255596963564));
#39554=CARTESIAN_POINT('Ctrl Pts',(102.989351160942,7.11955939513445,-2.75505472567269));
#39555=CARTESIAN_POINT('Ctrl Pts',(103.187862765384,6.16902856441037,4.49651243516987));
#39556=CARTESIAN_POINT('Ctrl Pts',(103.386374369826,-0.429696083313257,
7.62173856703403));
#39557=CARTESIAN_POINT('Ctrl Pts',(103.584885974268,-6.642319617587,3.76271745153168));
#39558=CARTESIAN_POINT('Ctrl Pts',(103.750312311303,-6.73590096227615,-2.30615546116277));
#39559=CARTESIAN_POINT('Ctrl Pts',(103.882653380931,-3.73715753574226,-5.58405708195391));
#39560=CARTESIAN_POINT('Ctrl Pts',(103.981909183152,-0.615773900064327,
-6.71037099599149));
#39561=CARTESIAN_POINT('Ctrl Pts',(104.081164985373,2.65846524097796,-6.17094826625278));
#39562=CARTESIAN_POINT('Ctrl Pts',(104.213506055002,6.20369374461536,-3.49355101672159));
#39563=CARTESIAN_POINT('Ctrl Pts',(104.378932392037,7.21618876722331,2.49099823295448));
#39564=CARTESIAN_POINT('Ctrl Pts',(104.577443996479,1.80964936637775,7.41624613180053));
#39565=CARTESIAN_POINT('Ctrl Pts',(104.775955600921,-5.24765132897221,5.54415845962204));
#39566=CARTESIAN_POINT('Ctrl Pts',(104.974467205363,-7.50206718560608,-1.41330833873472));
#39567=CARTESIAN_POINT('Ctrl Pts',(105.139893542398,-3.65639318803571,-6.10913280942983));
#39568=CARTESIAN_POINT('Ctrl Pts',(105.272234612026,0.749775929176509,-6.67726560261785));
#39569=CARTESIAN_POINT('Ctrl Pts',(105.371490414247,3.8608765281646,-5.52285152463062));
#39570=CARTESIAN_POINT('Ctrl Pts',(105.470746216468,6.01357951731961,-2.99748247611494));
#39571=CARTESIAN_POINT('Ctrl Pts',(105.603087286096,6.99331012387269,1.33578748391403));
#39572=CARTESIAN_POINT('Ctrl Pts',(105.768513623132,3.9039316817389,6.56031791313918));
#39573=CARTESIAN_POINT('Ctrl Pts',(105.967025227573,-3.40459787396335,6.83258726202722));
#39574=CARTESIAN_POINT('Ctrl Pts',(106.165536832016,-7.58664600136129,0.847549771001657));
#39575=CARTESIAN_POINT('Ctrl Pts',(106.364048436458,-4.8178809406568,-5.92169588117069));
#39576=CARTESIAN_POINT('Ctrl Pts',(106.529474773493,1.15037385181886,-7.02618964947138));
#39577=CARTESIAN_POINT('Ctrl Pts',(106.661815843121,4.88251957521103,-4.6161732723596));
#39578=CARTESIAN_POINT('Ctrl Pts',(106.761071645342,6.51367075904044,-1.72636546984731));
#39579=CARTESIAN_POINT('Ctrl Pts',(106.860327447563,6.52791332908397,1.59197142916921));
#39580=CARTESIAN_POINT('Ctrl Pts',(106.992668517191,4.47932614866,5.53411952875296));
#39581=CARTESIAN_POINT('Ctrl Pts',(107.158094854226,-1.25251946123205,7.53055645039344));
#39582=CARTESIAN_POINT('Ctrl Pts',(107.356606458668,-7.01053418130777,3.0212936021343));
#39583=CARTESIAN_POINT('Ctrl Pts',(107.555118063111,-6.34174919999383,-4.2495111512557));
#39584=CARTESIAN_POINT('Ctrl Pts',(107.753629667552,0.142238626393045,-7.63256099340945));
#39585=CARTESIAN_POINT('Ctrl Pts',(107.919056004588,5.41372170278917,-4.62437297999697));
#39586=CARTESIAN_POINT('Ctrl Pts',(108.051397074216,6.70877360903263,-0.374065744790461));
#39587=CARTESIAN_POINT('Ctrl Pts',(108.150652876437,6.08947724034344,2.88485671444533));
#39588=CARTESIAN_POINT('Ctrl Pts',(108.249908678658,3.9584365600631,5.43084385761433));
#39589=CARTESIAN_POINT('Ctrl Pts',(108.382249748286,-0.150530275064401,
7.1150135755553));
#39590=CARTESIAN_POINT('Ctrl Pts',(108.547676085321,-5.81759659987454,4.94987406613489));
#39591=CARTESIAN_POINT('Ctrl Pts',(108.746187689763,-7.30404329578078,-2.22825616357533));
#39592=CARTESIAN_POINT('Ctrl Pts',(108.911614026798,-2.97046704781651,-6.46879341979401));
#39593=CARTESIAN_POINT('Ctrl Pts',(109.043955096426,1.4759275490682,-6.55624346037556));
#39594=CARTESIAN_POINT('Ctrl Pts',(109.143210898647,4.43222131992785,-5.07069835199561));
#39595=CARTESIAN_POINT('Ctrl Pts',(109.242466700868,6.31884020592842,-2.32048750504607));
#39596=CARTESIAN_POINT('Ctrl Pts',(109.308637235682,6.54473344473606,-0.120973595496458));
#39597=CARTESIAN_POINT('Ctrl Pts',(109.341722503089,6.38817262844173,0.941409491315552));
#39598=CARTESIAN_POINT('Ctrl Pts',(31.067,-1.68325362372015,5.98713018070703));
#39599=CARTESIAN_POINT('Ctrl Pts',(31.100085267407,-2.67894146944392,5.70719720383451));
#39600=CARTESIAN_POINT('Ctrl Pts',(31.166255802221,-4.52416925940906,4.64399692160856));
#39601=CARTESIAN_POINT('Ctrl Pts',(31.2655116044422,-6.20083243674659,1.90406440993152));
#39602=CARTESIAN_POINT('Ctrl Pts',(31.3647674066631,-6.34501955724797,-1.27931918847895));
#39603=CARTESIAN_POINT('Ctrl Pts',(31.4971084762913,-4.52035937174355,-5.15463560703619));
#39604=CARTESIAN_POINT('Ctrl Pts',(31.6625348133263,0.911741987501496,-7.29827737450832));
#39605=CARTESIAN_POINT('Ctrl Pts',(31.8610464177685,6.63914845639706,-3.16971042113852));
#39606=CARTESIAN_POINT('Ctrl Pts',(32.0264727548036,6.31536279232879,2.66437234788271));
#39607=CARTESIAN_POINT('Ctrl Pts',(32.1588138244316,3.21934995423852,5.61536002384009));
#39608=CARTESIAN_POINT('Ctrl Pts',(32.2580696266527,0.14301869708689,6.4884091364757));
#39609=CARTESIAN_POINT('Ctrl Pts',(32.3573254288737,-2.96596409463713,5.75195268151558));
#39610=CARTESIAN_POINT('Ctrl Pts',(32.4896664985018,-6.19418404416841,2.9425316853334));
#39611=CARTESIAN_POINT('Ctrl Pts',(32.6550928355369,-6.76718021184908,-2.87509801732424));
#39612=CARTESIAN_POINT('Ctrl Pts',(32.853604439979,-1.24379023624101,-7.2466418339485));
#39613=CARTESIAN_POINT('Ctrl Pts',(33.0521160444211,5.41227178463782,-4.97673046693937));
#39614=CARTESIAN_POINT('Ctrl Pts',(33.2506276488633,7.11391162562153,1.85873863792625));
#39615=CARTESIAN_POINT('Ctrl Pts',(33.4160539858983,3.10541110519021,6.11397050225541));
#39616=CARTESIAN_POINT('Ctrl Pts',(33.5483950555264,-1.16614656773419,6.36572295470293));
#39617=CARTESIAN_POINT('Ctrl Pts',(33.6476508577475,-4.07834394078075,5.04884480068));
#39618=CARTESIAN_POINT('Ctrl Pts',(33.7469066599685,-5.97817189517101,2.47867161336443));
#39619=CARTESIAN_POINT('Ctrl Pts',(33.8792477295966,-6.6302737442775,-1.75030082377511));
#39620=CARTESIAN_POINT('Ctrl Pts',(34.0446740666317,-3.31312753510712,-6.56400641995886));
#39621=CARTESIAN_POINT('Ctrl Pts',(34.2431856710738,3.72736559794809,-6.33774649263565));
#39622=CARTESIAN_POINT('Ctrl Pts',(34.4416972755159,7.34611894960073,-0.307926448941118));
#39623=CARTESIAN_POINT('Ctrl Pts',(34.640208879958,4.233914906245,6.01140200914276));
#39624=CARTESIAN_POINT('Ctrl Pts',(34.8056352169931,-1.57434350116745,6.67424438783693));
#39625=CARTESIAN_POINT('Ctrl Pts',(34.9379762866212,-4.99945699673356,4.10947315312662));
#39626=CARTESIAN_POINT('Ctrl Pts',(35.0372320888423,-6.37382702555459,1.22395397566176));
#39627=CARTESIAN_POINT('Ctrl Pts',(35.1364878910633,-6.16600174500198,-1.96539115710818));
#39628=CARTESIAN_POINT('Ctrl Pts',(35.2688289606914,-3.93449142709178,-5.61639323287909));
#39629=CARTESIAN_POINT('Ctrl Pts',(35.4342552977265,1.706159430506,-7.15206323045347));
#39630=CARTESIAN_POINT('Ctrl Pts',(35.6327669021685,6.93766837888352,-2.43496237142141));
#39631=CARTESIAN_POINT('Ctrl Pts',(35.8312785066107,5.80973766223456,4.50635469098045));
#39632=CARTESIAN_POINT('Ctrl Pts',(36.0297901110528,-0.646180895956555,
7.3243046569134));
#39633=CARTESIAN_POINT('Ctrl Pts',(36.1952164480879,-5.51037651268064,4.08164750837416));
#39634=CARTESIAN_POINT('Ctrl Pts',(36.3275575177159,-6.47105737915941,-0.0880703169200902));
#39635=CARTESIAN_POINT('Ctrl Pts',(36.426813319937,-5.65834786130082,-3.17912466680208));
#39636=CARTESIAN_POINT('Ctrl Pts',(36.526069122158,-3.44104873410895,-5.48101483247933));
#39637=CARTESIAN_POINT('Ctrl Pts',(36.6584101917862,0.619923098873849,-6.82933313338426));
#39638=CARTESIAN_POINT('Ctrl Pts',(36.8238365288212,5.919465903525,-4.36152632411429));
#39639=CARTESIAN_POINT('Ctrl Pts',(37.0223481332634,6.8706564039049,2.61808419966792));
#39640=CARTESIAN_POINT('Ctrl Pts',(37.2208597377055,1.52886927114417,7.19185949867951));
#39641=CARTESIAN_POINT('Ctrl Pts',(37.4193713421476,-5.22102444228719,5.17724755367456));
#39642=CARTESIAN_POINT('Ctrl Pts',(37.5847976791827,-6.84333909992013,-0.439096411762364));
#39643=CARTESIAN_POINT('Ctrl Pts',(37.7171387488107,-4.88576711085616,-4.2440098636368));
#39644=CARTESIAN_POINT('Ctrl Pts',(37.8163945510318,-2.26989742046013,-6.08040293629282));
#39645=CARTESIAN_POINT('Ctrl Pts',(37.9156503532528,0.909436095338548,-6.40743833155411));
#39646=CARTESIAN_POINT('Ctrl Pts',(38.0479914228809,4.88148948210039,-4.81613497853341));
#39647=CARTESIAN_POINT('Ctrl Pts',(38.213417759916,7.33645041645639,0.489370765242909));
#39648=CARTESIAN_POINT('Ctrl Pts',(38.4119293643581,3.55798549376158,6.43436271305828));
#39649=CARTESIAN_POINT('Ctrl Pts',(38.6104409688003,-3.4742282511699,6.47997086072042));
#39650=CARTESIAN_POINT('Ctrl Pts',(38.8089525732423,-7.32948579331351,0.584488207419706));
#39651=CARTESIAN_POINT('Ctrl Pts',(38.9743789102775,-4.94354729154295,-4.75241368902037));
#39652=CARTESIAN_POINT('Ctrl Pts',(39.1067199799055,-0.992468299979939,
-6.39510333440429));
#39653=CARTESIAN_POINT('Ctrl Pts',(39.2059757821266,2.19083962730784,-6.10933350657059));
#39654=CARTESIAN_POINT('Ctrl Pts',(39.3052315843476,4.83030849556222,-4.30702447425982));
#39655=CARTESIAN_POINT('Ctrl Pts',(39.4375726539757,6.83706805014439,-0.527822103558383));
#39656=CARTESIAN_POINT('Ctrl Pts',(39.6029989910108,5.28773755787813,5.10909189367368));
#39657=CARTESIAN_POINT('Ctrl Pts',(39.8015105954529,-1.43545748919326,7.2110849456744));
#39658=CARTESIAN_POINT('Ctrl Pts',(40.000022199895,-6.8361201447979,2.70698091291776));
#39659=CARTESIAN_POINT('Ctrl Pts',(40.1985338043371,-5.97553982112241,-4.28438003743567));
#39660=CARTESIAN_POINT('Ctrl Pts',(40.3639601413723,-0.708451912413997,
-6.82071782022295));
#39661=CARTESIAN_POINT('Ctrl Pts',(40.4963012110003,3.3696668804336,-5.52518643116073));
#39662=CARTESIAN_POINT('Ctrl Pts',(40.5955570132214,5.6166365191778,-3.25224974110642));
#39663=CARTESIAN_POINT('Ctrl Pts',(40.6948128154424,6.46937068698724,-0.17199679800523));
#39664=CARTESIAN_POINT('Ctrl Pts',(40.8271538850705,5.56285463090548,4.00983092545351));
#39665=CARTESIAN_POINT('Ctrl Pts',(40.9925802221055,0.741127608027151,7.3153071246269));
#39666=CARTESIAN_POINT('Ctrl Pts',(41.1910918265477,-5.75079853390819,4.58133174081647));
#39667=CARTESIAN_POINT('Ctrl Pts',(41.3896034309898,-6.96866783622726,-2.34477139298153));
#39668=CARTESIAN_POINT('Ctrl Pts',(41.5881150354319,-1.7987828877996,-7.12933156625193));
#39669=CARTESIAN_POINT('Ctrl Pts',(41.753541372467,3.86131211317401,-5.66695371958917));
#39670=CARTESIAN_POINT('Ctrl Pts',(41.8858824420951,6.13999062787377,-2.04520294195858));
#39671=CARTESIAN_POINT('Ctrl Pts',(41.9851382443162,6.38916632461915,1.14117826979005));
#39672=CARTESIAN_POINT('Ctrl Pts',(42.0843940465372,5.05233903023813,4.04428118553917));
#39673=CARTESIAN_POINT('Ctrl Pts',(42.2167351161653,1.66078038279294,6.65326267446582));
#39674=CARTESIAN_POINT('Ctrl Pts',(42.3821614532004,-4.15558680069482,6.06581295465727));
#39675=CARTESIAN_POINT('Ctrl Pts',(42.5806730576425,-7.34949512093008,-0.212616472640353));
#39676=CARTESIAN_POINT('Ctrl Pts',(42.7791846620846,-3.80925655132213,-6.2888670540267));
#39677=CARTESIAN_POINT('Ctrl Pts',(42.9776962665266,3.22770883173084,-6.60642748817874));
#39678=CARTESIAN_POINT('Ctrl Pts',(43.1431226035619,6.60701429937979,-1.83615297377451));
#39679=CARTESIAN_POINT('Ctrl Pts',(43.2754636731898,6.00981779016149,2.40092276286268));
#39680=CARTESIAN_POINT('Ctrl Pts',(43.3747194754109,4.14349036564128,4.9955201688039));
#39681=CARTESIAN_POINT('Ctrl Pts',(43.473975277632,1.24861120530404,6.35006378252714));
#39682=CARTESIAN_POINT('Ctrl Pts',(43.6063163472601,-3.02583705454058,6.15373104828925));
#39683=CARTESIAN_POINT('Ctrl Pts',(43.7717426842951,-7.08922568451271,1.95086330967669));
#39684=CARTESIAN_POINT('Ctrl Pts',(43.9702542887373,-5.47633209238865,-4.90612587597253));
#39685=CARTESIAN_POINT('Ctrl Pts',(44.1687658931793,1.14962582217418,-7.26213775454605));
#39686=CARTESIAN_POINT('Ctrl Pts',(44.3672774976215,6.72944929157678,-2.96268471003815));
#39687=CARTESIAN_POINT('Ctrl Pts',(44.5327038346566,6.2316005792506,2.86203597391672));
#39688=CARTESIAN_POINT('Ctrl Pts',(44.6650449042847,3.04064127406932,5.71286623566488));
#39689=CARTESIAN_POINT('Ctrl Pts',(44.7643007065057,-0.0595468312504839,
6.49000680600387));
#39690=CARTESIAN_POINT('Ctrl Pts',(44.8635565087267,-3.14495343806531,5.65611243316245));
#39691=CARTESIAN_POINT('Ctrl Pts',(44.9958975783549,-6.28306630941009,2.7472119406529));
#39692=CARTESIAN_POINT('Ctrl Pts',(45.1613239153899,-6.67395475143974,-3.08566304620775));
#39693=CARTESIAN_POINT('Ctrl Pts',(45.3598355198321,-1.01618098913832,-7.2820093720296));
#39694=CARTESIAN_POINT('Ctrl Pts',(45.5583471242741,5.56543150817819,-4.80481596159418));
#39695=CARTESIAN_POINT('Ctrl Pts',(45.7568587287163,7.05223625244414,2.08061344288397));
#39696=CARTESIAN_POINT('Ctrl Pts',(45.9222850657513,2.91241425495877,6.20821543624437));
#39697=CARTESIAN_POINT('Ctrl Pts',(46.0546261353794,-1.3649168534335,6.32608425231493));
#39698=CARTESIAN_POINT('Ctrl Pts',(46.1538819376005,-4.23445444437469,4.9186512099969));
#39699=CARTESIAN_POINT('Ctrl Pts',(46.2531377398215,-6.05285999815342,2.29024580054805));
#39700=CARTESIAN_POINT('Ctrl Pts',(46.3854788094496,-6.5722108424563,-1.957074433334));
#39701=CARTESIAN_POINT('Ctrl Pts',(46.5509051464847,-3.10594562392494,-6.66453976207049));
#39702=CARTESIAN_POINT('Ctrl Pts',(46.7494167509268,3.92400822288565,-6.21791313575052));
#39703=CARTESIAN_POINT('Ctrl Pts',(46.947928355369,7.35215906316875,-0.077726487626221));
#39704=CARTESIAN_POINT('Ctrl Pts',(47.146439959811,4.04358699335335,6.14104166132917));
#39705=CARTESIAN_POINT('Ctrl Pts',(47.3118662968462,-1.7825799675908,6.62166930271015));
#39706=CARTESIAN_POINT('Ctrl Pts',(47.4442073664742,-5.12569603706815,3.95089611604222));
#39707=CARTESIAN_POINT('Ctrl Pts',(47.5434631686953,-6.4090299071312,1.02375281029476));
#39708=CARTESIAN_POINT('Ctrl Pts',(47.6427189709163,-6.10142998607327,-2.15751989775753));
#39709=CARTESIAN_POINT('Ctrl Pts',(47.7750600405443,-3.756680423898,-5.73684999699412));
#39710=CARTESIAN_POINT('Ctrl Pts',(47.9404863775796,1.92929451774911,-7.09512587082007));
#39711=CARTESIAN_POINT('Ctrl Pts',(48.1389979820215,7.01051831056036,-2.21651016562319));
#39712=CARTESIAN_POINT('Ctrl Pts',(48.3375095864638,5.66576857146238,4.68608053618823));
#39713=CARTESIAN_POINT('Ctrl Pts',(48.5360211909057,-0.875229719861018,
7.30047679240671));
#39714=CARTESIAN_POINT('Ctrl Pts',(48.701447527941,-5.63549357111038,3.90708432277619));
#39715=CARTESIAN_POINT('Ctrl Pts',(48.833788597569,-6.46512562050092,-0.290672832091888));
#39716=CARTESIAN_POINT('Ctrl Pts',(48.93304439979,-5.55601616227824,-3.3547605833489));
#39717=CARTESIAN_POINT('Ctrl Pts',(49.0323002020111,-3.26771921629748,-5.58608549053932));
#39718=CARTESIAN_POINT('Ctrl Pts',(49.1646412716392,0.833484420250366,-6.80657031231661));
#39719=CARTESIAN_POINT('Ctrl Pts',(49.3300676086743,6.05314692292063,-4.17401494828823));
#39720=CARTESIAN_POINT('Ctrl Pts',(49.5285792131164,6.78529949630181,2.83195957642392));
#39721=CARTESIAN_POINT('Ctrl Pts',(49.7270908175584,1.30290129179695,7.23620981735928));
#39722=CARTESIAN_POINT('Ctrl Pts',(49.9256024220008,-5.38059290072692,5.0112082869947));
#39723=CARTESIAN_POINT('Ctrl Pts',(50.0910287590355,-6.82623212432137,-0.653185027532664));
#39724=CARTESIAN_POINT('Ctrl Pts',(50.2233698286639,-4.75046670097809,-4.39492959068425));
#39725=CARTESIAN_POINT('Ctrl Pts',(50.3226256308848,-2.07837204216358,-6.14850419382157));
#39726=CARTESIAN_POINT('Ctrl Pts',(50.4218814331059,1.10964349084127,-6.37581612873264));
#39727=CARTESIAN_POINT('Ctrl Pts',(50.554222502734,5.02991597370948,-4.66090559792109));
#39728=CARTESIAN_POINT('Ctrl Pts',(50.719648839769,7.31752721429885,0.718876851061941));
#39729=CARTESIAN_POINT('Ctrl Pts',(50.9181604442113,3.35474386460336,6.54262775189899));
#39730=CARTESIAN_POINT('Ctrl Pts',(51.1166720486532,-3.6754491338023,6.36799481484125));
#39731=CARTESIAN_POINT('Ctrl Pts',(51.3151836530955,-7.34419465547514,0.35467354213092));
#39732=CARTESIAN_POINT('Ctrl Pts',(51.4806099901304,-4.79229751986203,-4.90489349287364));
#39733=CARTESIAN_POINT('Ctrl Pts',(51.6129510597586,-0.791714381456252,
-6.42304665422641));
#39734=CARTESIAN_POINT('Ctrl Pts',(51.7122068619796,2.38108318749985,-6.03772945910084));
#39735=CARTESIAN_POINT('Ctrl Pts',(51.8114626642006,4.96281693597846,-4.15364755897021));
#39736=CARTESIAN_POINT('Ctrl Pts',(51.9438037338288,6.85024388311463,-0.313455638265433));
#39737=CARTESIAN_POINT('Ctrl Pts',(52.1092300708638,5.12514934704392,5.27217532234014));
#39738=CARTESIAN_POINT('Ctrl Pts',(52.307741675306,-1.66057365242597,7.16259585917574));
#39739=CARTESIAN_POINT('Ctrl Pts',(52.506253279748,-6.91753833237311,2.49157534848164));
#39740=CARTESIAN_POINT('Ctrl Pts',(52.7047648841903,-5.83844070433739,-4.46940696300231));
#39741=CARTESIAN_POINT('Ctrl Pts',(52.8701912212252,-0.494508874927136,
-6.83955822169301));
#39742=CARTESIAN_POINT('Ctrl Pts',(53.0025322908534,3.54103930044635,-5.41695307870284));
#39743=CARTESIAN_POINT('Ctrl Pts',(53.1017880930744,5.71572828749395,-3.07476573264209));
#39744=CARTESIAN_POINT('Ctrl Pts',(53.2010438952954,6.47158394013595,0.0306804489560287));
#39745=CARTESIAN_POINT('Ctrl Pts',(53.3333849649236,5.43455561682152,4.18206897874528));
#39746=CARTESIAN_POINT('Ctrl Pts',(53.4988113019586,0.511680132839369,7.33492821373557));
#39747=CARTESIAN_POINT('Ctrl Pts',(53.6973229064008,-5.89144563848159,4.39899449713555));
#39748=CARTESIAN_POINT('Ctrl Pts',(53.8958345108428,-6.8918218408794,-2.56185011477848));
#39749=CARTESIAN_POINT('Ctrl Pts',(54.094346115285,-1.57464063360658,-7.18216508679608));
#39750=CARTESIAN_POINT('Ctrl Pts',(54.2597724523201,4.03688294466771,-5.54325462037972));
#39751=CARTESIAN_POINT('Ctrl Pts',(54.3921135219481,6.20102619469151,-1.85192173617664));
#39752=CARTESIAN_POINT('Ctrl Pts',(54.4913693241692,6.35029591436066,1.34069980500598));
#39753=CARTESIAN_POINT('Ctrl Pts',(54.5906251263902,4.92321156794364,4.2005151876216));
#39754=CARTESIAN_POINT('Ctrl Pts',(54.7229661960184,1.45161424482283,6.70200804084397));
#39755=CARTESIAN_POINT('Ctrl Pts',(54.8883925330533,-4.34350386041609,5.93270281351995));
#39756=CARTESIAN_POINT('Ctrl Pts',(55.0869041374956,-7.339232276092,-0.442666798599518));
#39757=CARTESIAN_POINT('Ctrl Pts',(55.2854157419376,-3.61044798336259,-6.4050721819856));
#39758=CARTESIAN_POINT('Ctrl Pts',(55.4839273463797,3.43301069967906,-6.50210934965618));
#39759=CARTESIAN_POINT('Ctrl Pts',(55.6493536834148,6.66127426453652,-1.62834912347856));
#39760=CARTESIAN_POINT('Ctrl Pts',(55.7816947530429,5.93168364981801,2.58794688172988));
#39761=CARTESIAN_POINT('Ctrl Pts',(55.880950555264,3.98501993711935,5.12282639446718));
#39762=CARTESIAN_POINT('Ctrl Pts',(55.980206357485,1.04914210494851,6.38605048741379));
#39763=CARTESIAN_POINT('Ctrl Pts',(56.1125474271131,-3.21706142470918,6.05595669444211));
#39764=CARTESIAN_POINT('Ctrl Pts',(56.2779737641482,-7.14684138056117,1.72790241046636));
#39765=CARTESIAN_POINT('Ctrl Pts',(56.4764853685903,-5.32000740755992,-5.07521482112047));
#39766=CARTESIAN_POINT('Ctrl Pts',(56.6749969730323,1.3764809281104,-7.2225746483897));
#39767=CARTESIAN_POINT('Ctrl Pts',(56.8735085774746,6.81892734073127,-2.7504942066517));
#39768=CARTESIAN_POINT('Ctrl Pts',(57.0389349145096,6.13891757971937,3.05577922054628));
#39769=CARTESIAN_POINT('Ctrl Pts',(57.1712759841377,2.86024754923171,5.80528413958247));
#39770=CARTESIAN_POINT('Ctrl Pts',(57.2705317863587,-0.262756750612794,
6.48495898653921));
#39771=CARTESIAN_POINT('Ctrl Pts',(57.3697875885798,-3.32053611010715,5.55485192652768));
#39772=CARTESIAN_POINT('Ctrl Pts',(57.5021286582079,-6.36601560896188,2.54910591419103));
#39773=CARTESIAN_POINT('Ctrl Pts',(57.6675549952429,-6.57405175731321,-3.29314924520042));
#39774=CARTESIAN_POINT('Ctrl Pts',(57.8660665996852,-0.787641354648353,
-7.31026028219656));
#39775=CARTESIAN_POINT('Ctrl Pts',(58.0645782041271,5.71316809273326,-4.6281740072287));
#39776=CARTESIAN_POINT('Ctrl Pts',(58.2630898085693,6.98362156225626,2.30043872645768));
#39777=CARTESIAN_POINT('Ctrl Pts',(58.4285161456044,2.71657121158352,6.29637487350503));
#39778=CARTESIAN_POINT('Ctrl Pts',(58.5608572152325,-1.56235319508776,6.28023825009631));
#39779=CARTESIAN_POINT('Ctrl Pts',(58.6601130174535,-4.38640864661985,4.78363390655549));
#39780=CARTESIAN_POINT('Ctrl Pts',(58.7593688196746,-6.1216119881301,2.09957296871427));
#39781=CARTESIAN_POINT('Ctrl Pts',(58.8917098893027,-6.50770029495222,-2.16192797437576));
#39782=CARTESIAN_POINT('Ctrl Pts',(59.0571362263377,-2.89571754477245,-6.75853596275806));
#39783=CARTESIAN_POINT('Ctrl Pts',(59.2556478307799,4.11680198598908,-6.09198044195556));
#39784=CARTESIAN_POINT('Ctrl Pts',(59.4541594352219,7.35098720564501,0.15254966226341));
#39785=CARTESIAN_POINT('Ctrl Pts',(59.6526710396641,3.84929275248138,6.26465751375856));
#39786=CARTESIAN_POINT('Ctrl Pts',(59.8180973766992,-1.98906791709047,6.56259891479826));
#39787=CARTESIAN_POINT('Ctrl Pts',(59.9504384463272,-5.24690719279156,3.7884435978916));
#39788=CARTESIAN_POINT('Ctrl Pts',(60.0496942485483,-6.43794609299798,0.822547427654274));
#39789=CARTESIAN_POINT('Ctrl Pts',(60.1489500507694,-6.03087324568868,-2.34753229554149));
#39790=CARTESIAN_POINT('Ctrl Pts',(60.2812911203974,-3.57518444437901,-5.85167940714288));
#39791=CARTESIAN_POINT('Ctrl Pts',(60.4467174574326,2.15053713527687,-7.03122880361549));
#39792=CARTESIAN_POINT('Ctrl Pts',(60.6452290618746,7.07649152718233,-1.99588375481379));
#39793=CARTESIAN_POINT('Ctrl Pts',(60.8437406663167,5.5162418506764,4.86120974057477));
#39794=CARTESIAN_POINT('Ctrl Pts',(61.0422522707589,-1.1034200191743,7.26948778940321));
#39795=CARTESIAN_POINT('Ctrl Pts',(61.207678607794,-5.75508269601921,3.72868862434105));
#39796=CARTESIAN_POINT('Ctrl Pts',(61.340019677422,-6.45285213102613,-0.492990222301885));
#39797=CARTESIAN_POINT('Ctrl Pts',(61.4392754796431,-5.448234490336,-3.52710576895582));
#39798=CARTESIAN_POINT('Ctrl Pts',(61.5385312818642,-3.09118434765655,-5.68567668030614));
#39799=CARTESIAN_POINT('Ctrl Pts',(61.6708723514922,1.04622816527626,-6.77713083254947));
#39800=CARTESIAN_POINT('Ctrl Pts',(61.8362986885273,6.18089032700829,-3.98240922363489));
#39801=CARTESIAN_POINT('Ctrl Pts',(62.0348102929695,6.69328679484465,3.04305704497484));
#39802=CARTESIAN_POINT('Ctrl Pts',(62.2333218974115,1.07565527860131,7.27346203802769));
#39803=CARTESIAN_POINT('Ctrl Pts',(62.4318335018537,-5.53488346138075,4.84025345699285));
#39804=CARTESIAN_POINT('Ctrl Pts',(62.5972598388888,-6.80242920348616,-0.866632925101025));
#39805=CARTESIAN_POINT('Ctrl Pts',(62.7296009085167,-4.61050649279502,-4.54153827068194));
#39806=CARTESIAN_POINT('Ctrl Pts',(62.828856710738,-1.88480796006642,-6.2105742987874));
#39807=CARTESIAN_POINT('Ctrl Pts',(62.9281125129588,1.30876242173983,-6.33793979993621));
#39808=CARTESIAN_POINT('Ctrl Pts',(63.0604535825871,5.17340855136809,-4.50110427072531));
#39809=CARTESIAN_POINT('Ctrl Pts',(63.225879919622,7.29142614877463,0.947677780663159));
#39810=CARTESIAN_POINT('Ctrl Pts',(63.4243915240643,3.14821152092017,6.64447503694298));
#39811=CARTESIAN_POINT('Ctrl Pts',(63.6229031285063,-3.87306471768808,6.24977231502176));
#39812=CARTESIAN_POINT('Ctrl Pts',(63.8214147329484,-7.35169949580919,0.124510972673139));
#39813=CARTESIAN_POINT('Ctrl Pts',(63.9868410699835,-4.63634691744933,-5.05256201905211));
#39814=CARTESIAN_POINT('Ctrl Pts',(64.1191821396116,-0.590183859376729,
-6.44468951899971));
#39815=CARTESIAN_POINT('Ctrl Pts',(64.2184379418327,2.56899111035366,-5.9602029195333));
#39816=CARTESIAN_POINT('Ctrl Pts',(64.3176937440537,5.09045728081569,-3.99619627350351));
#39817=CARTESIAN_POINT('Ctrl Pts',(64.4500348136817,6.85670021738249,-0.098781700014005));
#39818=CARTESIAN_POINT('Ctrl Pts',(64.615461150717,4.95753380652983,5.43008720152017));
#39819=CARTESIAN_POINT('Ctrl Pts',(64.8139727551589,-1.8840609360603,7.10708088361284));
#39820=CARTESIAN_POINT('Ctrl Pts',(65.0124843596012,-6.99217101119294,2.27372576342389));
#39821=CARTESIAN_POINT('Ctrl Pts',(65.2109959640432,-5.6956145805417,-4.65004978563959));
#39822=CARTESIAN_POINT('Ctrl Pts',(65.3764223010783,-0.280080766866481,
-6.8516896061695));
#39823=CARTESIAN_POINT('Ctrl Pts',(65.5087633707064,3.70893826617409,-5.30340616226556));
#39824=CARTESIAN_POINT('Ctrl Pts',(65.6080191729274,5.80921341909733,-2.89426564405251));
#39825=CARTESIAN_POINT('Ctrl Pts',(65.7072749751485,6.46744912735215,0.233327601020761));
#39826=CARTESIAN_POINT('Ctrl Pts',(65.8396160447766,5.30092577216001,4.35020478294281));
#39827=CARTESIAN_POINT('Ctrl Pts',(66.0050423818117,0.281730743593815,7.34735437050459));
#39828=CARTESIAN_POINT('Ctrl Pts',(66.2035539862537,-6.02631374284371,4.21234221923613));
#39829=CARTESIAN_POINT('Ctrl Pts',(66.402065590696,-6.80821556230926,-2.77641588274926));
#39830=CARTESIAN_POINT('Ctrl Pts',(66.6005771951379,-1.34895379295012,-7.22795352199158));
#39831=CARTESIAN_POINT('Ctrl Pts',(66.7660035321732,4.20849394244699,-5.41411806724503));
#39832=CARTESIAN_POINT('Ctrl Pts',(66.8983446018011,6.25597908877345,-1.65682395344729));
#39833=CARTESIAN_POINT('Ctrl Pts',(66.9976004040223,6.30519641260689,1.53890622628911));
#39834=CARTESIAN_POINT('Ctrl Pts',(67.0968562062432,4.78925485703138,4.35262885196658));
#39835=CARTESIAN_POINT('Ctrl Pts',(67.2291972758714,1.24102420380131,6.74417930312503));
#39836=CARTESIAN_POINT('Ctrl Pts',(67.3946236129065,-4.52716032826772,5.79377322678848));
#39837=CARTESIAN_POINT('Ctrl Pts',(67.5931352173485,-7.32177025883928,-0.672282947214057));
#39838=CARTESIAN_POINT('Ctrl Pts',(67.7916468217906,-3.40809791078333,-6.51499441152191));
#39839=CARTESIAN_POINT('Ctrl Pts',(67.9901584262328,3.63494514635811,-6.39141334988969));
#39840=CARTESIAN_POINT('Ctrl Pts',(68.1555847632678,6.70899997741019,-1.41894774382875));
#39841=CARTESIAN_POINT('Ctrl Pts',(68.2879258328959,5.84773120199377,2.77243208544916));
#39842=CARTESIAN_POINT('Ctrl Pts',(68.387181635117,3.82264019194717,5.24510836053448));
#39843=CARTESIAN_POINT('Ctrl Pts',(68.486437437338,0.848644543025793,6.4157715664878));
#39844=CARTESIAN_POINT('Ctrl Pts',(68.6187785069662,-3.40513155320004,5.95224512547316));
#39845=CARTESIAN_POINT('Ctrl Pts',(68.7842048440012,-7.19744374978217,1.50324015275999));
#39846=CARTESIAN_POINT('Ctrl Pts',(68.9827164484433,-5.15846906456438,-5.23931471226884));
#39847=CARTESIAN_POINT('Ctrl Pts',(69.1812280528855,1.60199468026975,-7.17594652687476));
#39848=CARTESIAN_POINT('Ctrl Pts',(69.3797396573275,6.90169914440493,-2.53556683556833));
#39849=CARTESIAN_POINT('Ctrl Pts',(69.5451659943627,6.04024352960078,3.24645669154724));
#39850=CARTESIAN_POINT('Ctrl Pts',(69.6775070639907,2.67700525894223,5.89210305530824));
#39851=CARTESIAN_POINT('Ctrl Pts',(69.7767628662118,-0.46561520595085,6.47334140092824));
#39852=CARTESIAN_POINT('Ctrl Pts',(69.8760186684328,-3.49303460355603,5.44852756041988));
#39853=CARTESIAN_POINT('Ctrl Pts',(70.008359738061,-6.44234667081631,2.34766771234552));
#39854=CARTESIAN_POINT('Ctrl Pts',(70.1737860750959,-6.46846181722385,-3.49571023081299));
#39855=CARTESIAN_POINT('Ctrl Pts',(70.3722976795382,-0.557063823628739,
-7.3341557210225));
#39856=CARTESIAN_POINT('Ctrl Pts',(70.5708092839802,5.85298547448848,-4.44184497426088));
#39857=CARTESIAN_POINT('Ctrl Pts',(70.7693208884224,6.91261030511504,2.50813707913662));
#39858=CARTESIAN_POINT('Ctrl Pts',(70.9678324928645,1.6305555301296,7.17107975691506));
#39859=CARTESIAN_POINT('Ctrl Pts',(71.1332588298994,-3.99925385407112,5.57258592607248));
#39860=CARTESIAN_POINT('Ctrl Pts',(71.2655998995277,-6.17961353551377,1.90043433999651));
#39861=CARTESIAN_POINT('Ctrl Pts',(71.3979409691555,-6.4383401840856,-2.35936209704413));
#39862=CARTESIAN_POINT('Ctrl Pts',(71.563367306191,-2.68617674612466,-6.85019204663737));
#39863=CARTESIAN_POINT('Ctrl Pts',(71.7618789106327,4.31461801077602,-5.95570943739811));
#39864=CARTESIAN_POINT('Ctrl Pts',(71.9273052476681,6.82127674849029,-0.680243620698351));
#39865=CARTESIAN_POINT('Ctrl Pts',(72.059646317296,5.51192719551105,3.39346452184477));
#39866=CARTESIAN_POINT('Ctrl Pts',(72.1589021195172,3.22776268544752,5.63020767552143));
#39867=CARTESIAN_POINT('Ctrl Pts',(72.2581579217381,0.144787652460555,6.47013157578351));
#39868=CARTESIAN_POINT('Ctrl Pts',(72.3904989913663,-4.03362152721484,5.54570745472594));
#39869=CARTESIAN_POINT('Ctrl Pts',(72.5559253284013,-7.31827787064979,0.71008190057901));
#39870=CARTESIAN_POINT('Ctrl Pts',(72.7544369328434,-4.55691781933503,-5.77022622668299));
#39871=CARTESIAN_POINT('Ctrl Pts',(72.9529485372856,2.37438354046372,-6.95863454231163));
#39872=CARTESIAN_POINT('Ctrl Pts',(73.1514601417277,7.13688992541174,-1.76848755210188));
#39873=CARTESIAN_POINT('Ctrl Pts',(73.3168864787627,5.65050896588544,3.88535316654217));
#39874=CARTESIAN_POINT('Ctrl Pts',(73.4492275483909,2.01909789486699,6.14862180311659));
#39875=CARTESIAN_POINT('Ctrl Pts',(73.5484833506118,-1.16830659219089,6.38426173854624));
#39876=CARTESIAN_POINT('Ctrl Pts',(73.647739152833,-4.06570784309721,5.0351131850683));
#39877=CARTESIAN_POINT('Ctrl Pts',(73.780080222461,-6.6602568208953,1.63250287976047));
#39878=CARTESIAN_POINT('Ctrl Pts',(73.9455065594962,-6.04810590357771,-4.18131674258692));
#39879=CARTESIAN_POINT('Ctrl Pts',(74.1440181639382,0.243835091874022,-7.34852555480543));
#39880=CARTESIAN_POINT('Ctrl Pts',(74.3425297683804,6.30499174515516,-3.78250739668092));
#39881=CARTESIAN_POINT('Ctrl Pts',(74.5410413728224,6.59265678988395,3.25574353737405));
#39882=CARTESIAN_POINT('Ctrl Pts',(74.7064677098575,1.80807007447841,6.61475457063774));
#39883=CARTESIAN_POINT('Ctrl Pts',(74.8388087794856,-2.42643051867436,5.99956455976299));
#39884=CARTESIAN_POINT('Ctrl Pts',(74.9380645817067,-5.01307646459359,4.1222322339533));
#39885=CARTESIAN_POINT('Ctrl Pts',(75.0373203839277,-6.35531052844578,1.22162515698238));
#39886=CARTESIAN_POINT('Ctrl Pts',(75.1696614535559,-6.14082190943682,-3.05195052583219));
#39887=CARTESIAN_POINT('Ctrl Pts',(75.3350877905908,-1.92073099598895,-7.09744889988669));
#39888=CARTESIAN_POINT('Ctrl Pts',(75.533599395033,4.92934482030065,-5.45544168096722));
#39889=CARTESIAN_POINT('Ctrl Pts',(75.7321109994751,7.25718867309859,1.18046468258034));
#39890=CARTESIAN_POINT('Ctrl Pts',(75.9306226039172,2.93407158228261,6.74197392506965));
#39891=CARTESIAN_POINT('Ctrl Pts',(76.0960489409524,-2.88848170832391,6.21938655461771));
#39892=CARTESIAN_POINT('Ctrl Pts',(76.2283900105804,-5.72573119748685,3.01634584205342));
#39893=CARTESIAN_POINT('Ctrl Pts',(76.3276458128015,-6.48969529698426,-0.0871155494871867));
#39894=CARTESIAN_POINT('Ctrl Pts',(76.4269016150225,-5.64270178030442,-3.1689519723282));
#39895=CARTESIAN_POINT('Ctrl Pts',(76.5592426846506,-2.72049697200563,-6.29467965193754));
#39896=CARTESIAN_POINT('Ctrl Pts',(76.7246690216857,3.1139858635671,-6.66078677788813));
#39897=CARTESIAN_POINT('Ctrl Pts',(76.9231806261278,7.28626036027289,-0.985238173931595));
#39898=CARTESIAN_POINT('Ctrl Pts',(77.1216922305699,4.78113090820971,5.58579193450243));
#39899=CARTESIAN_POINT('Ctrl Pts',(77.3202038350121,-2.11055225112471,7.0433342710871));
#39900=CARTESIAN_POINT('Ctrl Pts',(77.4856301720471,-6.22053122608817,2.88601575889286));
#39901=CARTESIAN_POINT('Ctrl Pts',(77.6179712416752,-6.32022906949386,-1.39177745825087));
#39902=CARTESIAN_POINT('Ctrl Pts',(77.7172270438963,-4.90061905992092,-4.25531044656318));
#39903=CARTESIAN_POINT('Ctrl Pts',(77.8164828461173,-2.26451286093752,-6.0625342462391));
#39904=CARTESIAN_POINT('Ctrl Pts',(77.9488239157454,1.98497522997811,-6.56383798030416));
#39905=CARTESIAN_POINT('Ctrl Pts',(78.1142502527804,6.6776735471879,-3.07760693659607));
#39906=CARTESIAN_POINT('Ctrl Pts',(78.3127618572227,6.20118802446728,3.95038623203051));
#39907=CARTESIAN_POINT('Ctrl Pts',(78.5112734616646,0.0464941470039349,
7.3524229061791));
#39908=CARTESIAN_POINT('Ctrl Pts',(78.7097850661068,-6.15816322790969,4.01746364232682));
#39909=CARTESIAN_POINT('Ctrl Pts',(78.8752114031418,-6.61403723891607,-1.81069243593199));
#39910=CARTESIAN_POINT('Ctrl Pts',(79.0075524727701,-3.92908674363906,-5.14243301805027));
#39911=CARTESIAN_POINT('Ctrl Pts',(79.106808274991,-0.996518304073061,-6.41332093667049));
#39912=CARTESIAN_POINT('Ctrl Pts',(79.2060640772121,2.18341903006714,-6.09220988831756));
#39913=CARTESIAN_POINT('Ctrl Pts',(79.33840514684,5.75275644429788,-3.73227664943248));
#39914=CARTESIAN_POINT('Ctrl Pts',(79.5038314838753,7.08686629844,1.95941688444093));
#39915=CARTESIAN_POINT('Ctrl Pts',(79.7023430883174,2.18670980208234,7.01987069243372));
#39916=CARTESIAN_POINT('Ctrl Pts',(79.9008546927594,-4.71010618431074,5.64581119322374));
#39917=CARTESIAN_POINT('Ctrl Pts',(80.0993662972016,-7.29669298683701,-0.906233918390003));
#39918=CARTESIAN_POINT('Ctrl Pts',(80.2647926342366,-3.88310974879154,-5.65203984187573));
#39919=CARTESIAN_POINT('Ctrl Pts',(80.3971337038648,0.318133770830362,-6.46383252320411));
#39920=CARTESIAN_POINT('Ctrl Pts',(80.4963895060858,3.37833202016725,-5.5417151612656));
#39921=CARTESIAN_POINT('Ctrl Pts',(80.5956453083068,5.59991621302585,-3.24396029434143));
#39922=CARTESIAN_POINT('Ctrl Pts',(80.7279863779349,6.80296829521341,0.862390903031537));
#39923=CARTESIAN_POINT('Ctrl Pts',(80.89341271497,4.14826379333761,6.07082333459648));
#39924=CARTESIAN_POINT('Ctrl Pts',(81.0919243194122,-2.86075767029707,6.77320823899939));
#39925=CARTESIAN_POINT('Ctrl Pts',(81.2904359238541,-7.24167919371434,1.27215044406616));
#39926=CARTESIAN_POINT('Ctrl Pts',(81.4889475282965,-4.98830655746467,-5.40183174004447));
#39927=CARTESIAN_POINT('Ctrl Pts',(81.6543738653314,0.682176659571807,-6.82339583348686));
#39928=CARTESIAN_POINT('Ctrl Pts',(81.7867149349596,4.41506970477836,-4.73175437719689));
#39929=CARTESIAN_POINT('Ctrl Pts',(81.8859707371805,6.1572775488005,-2.05223472198617));
#39930=CARTESIAN_POINT('Ctrl Pts',(81.9852265394016,6.37104488690502,1.13671765765088));
#39931=CARTESIAN_POINT('Ctrl Pts',(82.1175676090297,4.63949668876505,5.04966990705815));
#39932=CARTESIAN_POINT('Ctrl Pts',(82.2829939460648,-0.749954889722087,
7.3144074348083));
#39933=CARTESIAN_POINT('Ctrl Pts',(82.4815055505069,-6.55681952065862,3.32692080917517));
#39934=CARTESIAN_POINT('Ctrl Pts',(82.680017154949,-6.35232421720465,-3.7024669257845));
#39935=CARTESIAN_POINT('Ctrl Pts',(82.8785287593912,-0.323472535169768,
-7.34563502891261));
#39936=CARTESIAN_POINT('Ctrl Pts',(83.0439550964262,4.92520670119462,-4.77141851505581));
#39937=CARTESIAN_POINT('Ctrl Pts',(83.1762961660544,6.42635186854234,-0.7644224263167));
#39938=CARTESIAN_POINT('Ctrl Pts',(83.2755519682753,6.02756024934152,2.40670970572829));
#39939=CARTESIAN_POINT('Ctrl Pts',(83.3748077704965,4.13252826027979,4.98041666551734));
#39940=CARTESIAN_POINT('Ctrl Pts',(83.5071488401245,0.284353283747686,6.85151362148041));
#39941=CARTESIAN_POINT('Ctrl Pts',(83.6725751771596,-5.29389915633836,5.10270714244087));
#39942=CARTESIAN_POINT('Ctrl Pts',(83.8710867816018,-7.15547719212857,-1.69098505313933));
#39943=CARTESIAN_POINT('Ctrl Pts',(84.0695983860438,-2.46216747788131,-6.92806001762949));
#39944=CARTESIAN_POINT('Ctrl Pts',(84.2681099904858,4.49416806949842,-5.81940218769057));
#39945=CARTESIAN_POINT('Ctrl Pts',(84.4335363275211,6.84159716243557,-0.465450279045067));
#39946=CARTESIAN_POINT('Ctrl Pts',(84.565877397149,5.4018620288319,3.56401832285386));
#39947=CARTESIAN_POINT('Ctrl Pts',(84.6651331993702,3.05045783488768,5.72873818258966));
#39948=CARTESIAN_POINT('Ctrl Pts',(84.7643890015912,-0.0581711681516334,
6.47139522045821));
#39949=CARTESIAN_POINT('Ctrl Pts',(84.8967300712192,-4.20511699218411,5.41674134303595));
#39950=CARTESIAN_POINT('Ctrl Pts',(85.0621564082545,-7.33703562768,0.480517072696063));
#39951=CARTESIAN_POINT('Ctrl Pts',(85.2606680126964,-4.37392821203035,-5.91007921207641));
#39952=CARTESIAN_POINT('Ctrl Pts',(85.4591796171386,2.59110314784578,-6.88087703525041));
#39953=CARTESIAN_POINT('Ctrl Pts',(85.6576912215807,7.18878928721451,-1.54411691365224));
#39954=CARTESIAN_POINT('Ctrl Pts',(85.8231175586158,5.52605610955549,4.0603940165154));
#39955=CARTESIAN_POINT('Ctrl Pts',(85.9554586282439,1.82556334808452,6.2088371251229));
#39956=CARTESIAN_POINT('Ctrl Pts',(86.0547144304649,-1.36766347836997,6.34454338601461));
#39957=CARTESIAN_POINT('Ctrl Pts',(86.1539702326861,-4.22139086822476,4.90532354914965));
#39958=CARTESIAN_POINT('Ctrl Pts',(86.286311302314,-6.70811396298986,1.42313132031107));
#39959=CARTESIAN_POINT('Ctrl Pts',(86.4517376393492,-5.91419827707177,-4.36866652406411));
#39960=CARTESIAN_POINT('Ctrl Pts',(86.6502492437913,0.473839531513867,-7.33728562858142));
#39961=CARTESIAN_POINT('Ctrl Pts',(86.8487608482334,6.42035141139087,-3.58320695066083));
#39962=CARTESIAN_POINT('Ctrl Pts',(87.0472724526755,6.48746740946582,3.46060039156732));
#39963=CARTESIAN_POINT('Ctrl Pts',(87.2126987897107,1.60003763959895,6.66813131598175));
#39964=CARTESIAN_POINT('Ctrl Pts',(87.3450398593386,-2.61312105570604,5.92063664924637));
#39965=CARTESIAN_POINT('Ctrl Pts',(87.4442956615597,-5.13970835779019,3.9632224469427));
#39966=CARTESIAN_POINT('Ctrl Pts',(87.5435514637809,-6.39044957686313,1.02200498518542));
#39967=CARTESIAN_POINT('Ctrl Pts',(87.6758925334087,-6.0422361224665,-3.24275782871163));
#39968=CARTESIAN_POINT('Ctrl Pts',(87.8413188704441,-1.69752736119953,-7.15411694879083));
#39969=CARTESIAN_POINT('Ctrl Pts',(88.0398304748858,5.0977681804467,-5.29840012413548));
#39970=CARTESIAN_POINT('Ctrl Pts',(88.2383420793283,7.21666225322758,1.40714967926411));
#39971=CARTESIAN_POINT('Ctrl Pts',(88.4368536837702,2.72150289496444,6.83054979131966));
#39972=CARTESIAN_POINT('Ctrl Pts',(88.6022800208054,-3.0818294938239,6.125881378733));
#39973=CARTESIAN_POINT('Ctrl Pts',(88.7346210904335,-5.81738196310627,2.835561157778));
#39974=CARTESIAN_POINT('Ctrl Pts',(88.8338768926545,-6.48378429654595,-0.290302192469259));
#39975=CARTESIAN_POINT('Ctrl Pts',(88.9331326948756,-5.54069632003458,-3.34410291009848));
#39976=CARTESIAN_POINT('Ctrl Pts',(89.0654737645036,-2.52204036811142,-6.37678665762986));
#39977=CARTESIAN_POINT('Ctrl Pts',(89.2309001015388,3.32104580709813,-6.56000329315107));
#39978=CARTESIAN_POINT('Ctrl Pts',(89.4294117059809,7.31354018950449,-0.7565805928752));
#39979=CARTESIAN_POINT('Ctrl Pts',(89.6279233104229,4.60386296928326,5.73277681905332));
#39980=CARTESIAN_POINT('Ctrl Pts',(89.8264349148652,-2.33008407920169,6.97378639211496));
#39981=CARTESIAN_POINT('Ctrl Pts',(89.9918612518999,-6.30785793552618,2.68979998522734));
#39982=CARTESIAN_POINT('Ctrl Pts',(90.1242023215284,-6.27354478027196,-1.589017266771));
#39983=CARTESIAN_POINT('Ctrl Pts',(90.2234581237491,-4.76495748010495,-4.406689730385));
#39984=CARTESIAN_POINT('Ctrl Pts',(90.3227139259705,-2.07354969412331,-6.13047564632424));
#39985=CARTESIAN_POINT('Ctrl Pts',(90.4550549955982,2.18955288481874,-6.49845780627156));
#39986=CARTESIAN_POINT('Ctrl Pts',(90.6204813326336,6.77077586040887,-2.86698146263652));
#39987=CARTESIAN_POINT('Ctrl Pts',(90.8189929370755,6.07443748772285,4.14264329924265));
#39988=CARTESIAN_POINT('Ctrl Pts',(91.0175045415178,-0.183774947198175,
7.35027285655411));
#39989=CARTESIAN_POINT('Ctrl Pts',(91.2160161459598,-6.28095261185096,3.82264603994139));
#39990=CARTESIAN_POINT('Ctrl Pts',(91.3814424829949,-6.55409023249801,-2.01692759403598));
#39991=CARTESIAN_POINT('Ctrl Pts',(91.513783552623,-3.76612079172275,-5.26295298918085));
#39992=CARTESIAN_POINT('Ctrl Pts',(91.613039354844,-0.795191902178077,-6.44138215026858));
#39993=CARTESIAN_POINT('Ctrl Pts',(91.7122951570653,2.37312999160159,-6.02084662046249));
#39994=CARTESIAN_POINT('Ctrl Pts',(91.844636226693,5.86681383167074,-3.55029451733617));
#39995=CARTESIAN_POINT('Ctrl Pts',(92.0100625637283,7.0220299791157,2.18038607393216));
#39996=CARTESIAN_POINT('Ctrl Pts',(92.2085741681705,1.9658051306551,7.08490610278661));
#39997=CARTESIAN_POINT('Ctrl Pts',(92.4070857726124,-4.88459862582638,5.49554188061449));
#39998=CARTESIAN_POINT('Ctrl Pts',(92.6055973770546,-7.26473492135933,-1.13429051894974));
#39999=CARTESIAN_POINT('Ctrl Pts',(92.7710237140898,-3.7042076507531,-5.7708700709176));
#40000=CARTESIAN_POINT('Ctrl Pts',(92.9033647837178,0.520397198382932,-6.45069970934075));
#40001=CARTESIAN_POINT('Ctrl Pts',(93.0026205859388,3.55021779910258,-5.43320234723718));
#40002=CARTESIAN_POINT('Ctrl Pts',(93.10187638816,5.69875659207993,-3.06700395963218));
#40003=CARTESIAN_POINT('Ctrl Pts',(93.2342174577878,6.77262535525563,1.0750076709765));
#40004=CARTESIAN_POINT('Ctrl Pts',(93.3996437948232,3.95611714926058,6.19775165365016));
#40005=CARTESIAN_POINT('Ctrl Pts',(93.5981553992651,-3.07146236840367,6.6802996352329));
#40006=CARTESIAN_POINT('Ctrl Pts',(93.7966670037075,-7.27796574748004,1.04474823547117));
#40007=CARTESIAN_POINT('Ctrl Pts',(93.9951786081492,-4.8166978505934,-5.55539470020689));
#40008=CARTESIAN_POINT('Ctrl Pts',(94.1606049451846,0.895521517553394,-6.7986864103964));
#40009=CARTESIAN_POINT('Ctrl Pts',(94.2929460148125,4.56108251734731,-4.59117264477413));
#40010=CARTESIAN_POINT('Ctrl Pts',(94.3922018170336,6.21852484226242,-1.85840871534061));
#40011=CARTESIAN_POINT('Ctrl Pts',(94.4914576192548,6.33232305163478,1.33567389504654));
#40012=CARTESIAN_POINT('Ctrl Pts',(94.6237986888826,4.47908725340983,5.19248236122677));
#40013=CARTESIAN_POINT('Ctrl Pts',(94.7892250259181,-0.978642878797454,
7.28733466877817));
#40014=CARTESIAN_POINT('Ctrl Pts',(94.9877366303597,-6.657788546716,3.11995768628837));
#40015=CARTESIAN_POINT('Ctrl Pts',(95.1862482348023,-6.23326332199298,-3.89957852282909));
#40016=CARTESIAN_POINT('Ctrl Pts',(95.384759839244,-0.0932801621545284,
-7.35216208134352));
#40017=CARTESIAN_POINT('Ctrl Pts',(95.5501861762794,5.07221142391009,-4.61484203049959));
#40018=CARTESIAN_POINT('Ctrl Pts',(95.6825272459072,6.44713844549368,-0.562801784655363));
#40019=CARTESIAN_POINT('Ctrl Pts',(95.7817830481286,5.94923618490345,2.59428660392868));
#40020=CARTESIAN_POINT('Ctrl Pts',(95.8810388503493,3.97453618501874,5.10738701276399));
#40021=CARTESIAN_POINT('Ctrl Pts',(96.0133799199776,0.069653856197323,6.85705797231051));
#40022=CARTESIAN_POINT('Ctrl Pts',(96.1788062570125,-5.45109758750357,4.93442231173111));
#40023=CARTESIAN_POINT('Ctrl Pts',(96.3773178614549,-7.09901335357813,-1.91423449523096));
#40024=CARTESIAN_POINT('Ctrl Pts',(96.5758294658966,-2.24400282214668,-7.00176660787908));
#40025=CARTESIAN_POINT('Ctrl Pts',(96.7743410703392,4.67420254334854,-5.67580999001474));
#40026=CARTESIAN_POINT('Ctrl Pts',(96.9397674073738,6.85281755654995,-0.250972572108975));
#40027=CARTESIAN_POINT('Ctrl Pts',(97.0721084770024,5.28760290966167,3.73143343152621));
#40028=CARTESIAN_POINT('Ctrl Pts',(97.171364279223,2.86956225427671,5.82145571450295));
#40029=CARTESIAN_POINT('Ctrl Pts',(97.2706200814443,-0.260798927335446,
6.46639960903085));
#40030=CARTESIAN_POINT('Ctrl Pts',(97.4029611510722,-4.37268362577514,5.28239847078841));
#40031=CARTESIAN_POINT('Ctrl Pts',(97.5683874881074,-7.34848485781509,0.250516972397847));
#40032=CARTESIAN_POINT('Ctrl Pts',(97.7668990925496,-4.18670470445587,-6.04415320906906));
#40033=CARTESIAN_POINT('Ctrl Pts',(97.9654106969916,2.80531182390014,-6.79636004547279));
#40034=CARTESIAN_POINT('Ctrl Pts',(98.1639223014338,7.23361860234148,-1.31823760182156));
#40035=CARTESIAN_POINT('Ctrl Pts',(98.3293486384688,5.39619172482621,4.2314548992311));
#40036=CARTESIAN_POINT('Ctrl Pts',(98.4616897080969,1.63023388960724,6.26296075744928));
#40037=CARTESIAN_POINT('Ctrl Pts',(98.5609455103179,-1.56567653366841,6.29860231789631));
#40038=CARTESIAN_POINT('Ctrl Pts',(98.6602013125392,-4.37293411252434,4.77072187742011));
#40039=CARTESIAN_POINT('Ctrl Pts',(98.7925423821669,-6.74939027975622,1.21236403231126));
#40040=CARTESIAN_POINT('Ctrl Pts',(98.9579687192024,-5.77448975510201,-4.55173115717733));
#40041=CARTESIAN_POINT('Ctrl Pts',(99.1564803236441,0.70337938998819,-7.31884838828847));
#40042=CARTESIAN_POINT('Ctrl Pts',(99.3549919280866,6.52941314982036,-3.38039172522444));
#40043=CARTESIAN_POINT('Ctrl Pts',(99.5535035325282,6.37591445285421,3.66206271777009));
#40044=CARTESIAN_POINT('Ctrl Pts',(99.7189298695639,1.39043567136697,6.71496718823704));
#40045=CARTESIAN_POINT('Ctrl Pts',(99.8512709391915,-2.79724833035012,5.83590110972824));
#40046=CARTESIAN_POINT('Ctrl Pts',(99.9505267414128,-5.26129864878984,3.80032507758626));
#40047=CARTESIAN_POINT('Ctrl Pts',(100.049782543634,-6.41932014120929,0.821382315878928));
#40048=CARTESIAN_POINT('Ctrl Pts',(100.182123613262,-5.9377234255724,-3.43038426662649));
#40049=CARTESIAN_POINT('Ctrl Pts',(100.347549950297,-1.47265859680333,-7.20376742519206));
#40050=CARTESIAN_POINT('Ctrl Pts',(100.546061554739,5.26119106866268,-5.13616129381046));
#40051=CARTESIAN_POINT('Ctrl Pts',(100.744573159181,7.16905691026357,1.63245438356331));
#40052=CARTESIAN_POINT('Ctrl Pts',(100.943084763623,2.50626464765636,6.91242547698743));
#40053=CARTESIAN_POINT('Ctrl Pts',(101.108511100658,-3.27215427013865,6.02636724135885));
#40054=CARTESIAN_POINT('Ctrl Pts',(101.240852170287,-5.90332637858596,2.65199503243598));
#40055=CARTESIAN_POINT('Ctrl Pts',(101.340107972507,-6.47151326263513,-0.493204074016322));
#40056=CARTESIAN_POINT('Ctrl Pts',(101.439363774729,-5.43325591434297,-3.51597357120765));
#40057=CARTESIAN_POINT('Ctrl Pts',(101.571704844356,-2.3211098600259,-6.45263858533859));
#40058=CARTESIAN_POINT('Ctrl Pts',(101.737131181392,3.52484809098738,-6.45278501071125));
#40059=CARTESIAN_POINT('Ctrl Pts',(101.935642785834,7.33364606630008,-0.527180871479639));
#40060=CARTESIAN_POINT('Ctrl Pts',(102.134154390276,4.42207903767292,5.87413834375616));
#40061=CARTESIAN_POINT('Ctrl Pts',(102.332665994718,-2.54733029566822,6.89739782988979));
#40062=CARTESIAN_POINT('Ctrl Pts',(102.498092331753,-6.38899718011882,2.4909457496588));
#40063=CARTESIAN_POINT('Ctrl Pts',(102.630433401381,-6.22070668445104,-1.78469838633858));
#40064=CARTESIAN_POINT('Ctrl Pts',(102.729689203602,-4.62462188777941,-4.55374643147395));
#40065=CARTESIAN_POINT('Ctrl Pts',(102.828945005823,-1.88055255381611,-6.19240357829704));
#40066=CARTESIAN_POINT('Ctrl Pts',(102.961286075451,2.39198277703677,-6.42670320535172));
#40067=CARTESIAN_POINT('Ctrl Pts',(103.126712412487,6.85723662620696,-2.65354372701774));
#40068=CARTESIAN_POINT('Ctrl Pts',(103.325224016929,5.94172845146893,4.33083679050598));
#40069=CARTESIAN_POINT('Ctrl Pts',(103.523735621371,-0.413863774020237,
7.34091282291405));
#40070=CARTESIAN_POINT('Ctrl Pts',(103.722247225813,-6.39758092274897,3.6240787513264));
#40071=CARTESIAN_POINT('Ctrl Pts',(103.887673562848,-6.48771422857854,-2.22118432003229));
#40072=CARTESIAN_POINT('Ctrl Pts',(104.020014632476,-3.59946059997928,-5.37831045715732));
#40073=CARTESIAN_POINT('Ctrl Pts',(104.119270434697,-0.593085485580851,
-6.46312492323568));
#40074=CARTESIAN_POINT('Ctrl Pts',(104.218526236918,2.56051311720067,-5.94357742119504));
#40075=CARTESIAN_POINT('Ctrl Pts',(104.350867306546,5.97511638043491,-3.364829852218));
#40076=CARTESIAN_POINT('Ctrl Pts',(104.516293643581,6.95030565375228,2.39921649231612));
#40077=CARTESIAN_POINT('Ctrl Pts',(104.714805248023,1.74297217383987,7.14299183158766));
#40078=CARTESIAN_POINT('Ctrl Pts',(104.913316852465,-5.05429969713898,5.33988191415307));
#40079=CARTESIAN_POINT('Ctrl Pts',(105.111828456908,-7.22565077728843,-1.36123447626787));
#40080=CARTESIAN_POINT('Ctrl Pts',(105.277254793943,-3.52167204419261,-5.88403957747914));
#40081=CARTESIAN_POINT('Ctrl Pts',(105.409595863571,0.722150160936881,-6.43123931018474));
#40082=CARTESIAN_POINT('Ctrl Pts',(105.508851665792,3.71862112089202,-5.3193600409715));
#40083=CARTESIAN_POINT('Ctrl Pts',(105.608107468013,5.79200698135239,-2.88703913835982));
#40084=CARTESIAN_POINT('Ctrl Pts',(105.740448537641,6.73563905550354,1.2865699056858));
#40085=CARTESIAN_POINT('Ctrl Pts',(105.905874874676,3.76008989159166,6.31860060108252));
#40086=CARTESIAN_POINT('Ctrl Pts',(106.104386479118,-3.27915422052681,6.58083808626542));
#40087=CARTESIAN_POINT('Ctrl Pts',(106.30289808356,-7.30711325565383,0.816321489812915));
#40088=CARTESIAN_POINT('Ctrl Pts',(106.501409688003,-4.64036435591168,-5.70350883137131));
#40089=CARTESIAN_POINT('Ctrl Pts',(106.666836025037,1.10798790665508,-6.76730712296029));
#40090=CARTESIAN_POINT('Ctrl Pts',(106.799177094666,4.70262135634261,-4.44608868040009));
#40091=CARTESIAN_POINT('Ctrl Pts',(106.898432896887,6.2736721784315,-1.66275690292686));
#40092=CARTESIAN_POINT('Ctrl Pts',(106.997688699108,6.28738997577458,1.53331465981352));
#40093=CARTESIAN_POINT('Ctrl Pts',(107.130029768736,4.31428373900651,5.33021287136194));
#40094=CARTESIAN_POINT('Ctrl Pts',(107.295456105771,-1.20636992374352,7.25309034469861));
#40095=CARTESIAN_POINT('Ctrl Pts',(107.493967710213,-6.7522284862449,2.90997293473533));
#40096=CARTESIAN_POINT('Ctrl Pts',(107.692479314655,-6.10808513208516,-4.09293635920486));
#40097=CARTESIAN_POINT('Ctrl Pts',(107.890990919097,0.136997792198854,-7.35133649303282));
#40098=CARTESIAN_POINT('Ctrl Pts',(108.056417256132,5.21425114731496,-4.45398626681165));
#40099=CARTESIAN_POINT('Ctrl Pts',(108.18875832576,6.46158639258335,-0.360283155660035));
#40100=CARTESIAN_POINT('Ctrl Pts',(108.288014127981,5.8651082250223,2.77856311405613));
#40101=CARTESIAN_POINT('Ctrl Pts',(108.387269930202,3.81258651774621,5.23074243008551));
#40102=CARTESIAN_POINT('Ctrl Pts',(108.519610999831,-0.144983932043383,
6.8528582990123));
#40103=CARTESIAN_POINT('Ctrl Pts',(108.685037336866,-5.60324512615471,4.76749414642294));
#40104=CARTESIAN_POINT('Ctrl Pts',(108.883548941308,-7.03492315008415,-2.14615525054554));
#40105=CARTESIAN_POINT('Ctrl Pts',(109.048975278343,-2.8610191033943,-6.23044836115737));
#40106=CARTESIAN_POINT('Ctrl Pts',(109.181316347971,1.42154645890215,-6.31467627302082));
#40107=CARTESIAN_POINT('Ctrl Pts',(109.280572150192,4.26891450491086,-4.88386661729597));
#40108=CARTESIAN_POINT('Ctrl Pts',(109.379827952413,6.08602022828173,-2.23498829451912));
#40109=CARTESIAN_POINT('Ctrl Pts',(109.445998487227,6.30359034811574,-0.116516279140912));
#40110=CARTESIAN_POINT('Ctrl Pts',(109.479083754634,6.15279807233871,0.906722914414925));
#40111=CARTESIAN_POINT('Ctrl Pts',(109.067,6.85892174064777,1.0107826451168));
#40112=CARTESIAN_POINT('Ctrl Pts',(109.033914732593,7.0270196379767,-0.129888228207594));
#40113=CARTESIAN_POINT('Ctrl Pts',(109.000829465186,6.90574989959926,-1.31068707715371));
#40114=CARTESIAN_POINT('Ctrl Pts',(108.967744197779,6.50750749520052,-2.39323248417603));
#40115=CARTESIAN_POINT('Ctrl Pts',(108.934658930372,6.10926509080182,-3.47577789119822));
#40116=CARTESIAN_POINT('Ctrl Pts',(108.901573662965,5.4340500203817,-4.46006985629672));
#40117=CARTESIAN_POINT('Ctrl Pts',(108.868488395558,4.56741828174481,-5.21805184112751));
#40118=CARTESIAN_POINT('Ctrl Pts',(108.835403128151,3.70078654310793,-5.9760338259583));
#40119=CARTESIAN_POINT('Ctrl Pts',(108.802317860744,2.64273813625421,-6.50770583052161));
#40120=CARTESIAN_POINT('Ctrl Pts',(108.769232593337,1.51695734956969,-6.76180504555109));
#40121=CARTESIAN_POINT('Ctrl Pts',(108.73614732593,0.391176562885175,-7.01590426058057));
#40122=CARTESIAN_POINT('Ctrl Pts',(108.703062058523,-0.802336603629954,
-6.99243068607618));
#40123=CARTESIAN_POINT('Ctrl Pts',(108.669976791116,-1.90820675800765,-6.67324659991116));
#40124=CARTESIAN_POINT('Ctrl Pts',(108.603806256302,-4.11994706676328,-6.03487842758105));
#40125=CARTESIAN_POINT('Ctrl Pts',(108.537635721488,-5.98111532696877,-4.21366820860795));
#40126=CARTESIAN_POINT('Ctrl Pts',(108.471465186674,-6.64570211709476,-2.01854778325574));
#40127=CARTESIAN_POINT('Ctrl Pts',(108.451940678984,-6.84179740226082,-1.37084793098864));
#40128=CARTESIAN_POINT('Ctrl Pts',(108.432416171295,-6.93371537062503,-0.690594539326748));
#40129=CARTESIAN_POINT('Ctrl Pts',(108.412891663606,-6.92776634541837,-0.00844704756396031));
#40130=CARTESIAN_POINT('Origin',(-66.51072,1.12618006296016E-15,0.));
#40131=CARTESIAN_POINT('',(-66.51072,1.15821195975198,6.83557123116185));
#40132=CARTESIAN_POINT('Ctrl Pts',(-66.51072,4.88120307569149,-3.85434375923665));
#40133=CARTESIAN_POINT('Ctrl Pts',(-66.51072,4.99039108986081,-3.73103378318323));
#40134=CARTESIAN_POINT('Ctrl Pts',(-66.51072,5.09450400334291,-3.60353370689817));
#40135=CARTESIAN_POINT('Ctrl Pts',(-66.51072,5.19325944155552,-3.47211850304819));
#40136=CARTESIAN_POINT('Ctrl Pts',(-66.51072,5.29755106214915,-3.33333622605954));
#40137=CARTESIAN_POINT('Ctrl Pts',(-66.51072,5.39586868951527,-3.19018760651214));
#40138=CARTESIAN_POINT('Ctrl Pts',(-66.51072,5.48809659704528,-3.04312464176522));
#40139=CARTESIAN_POINT('Ctrl Pts',(-66.51072,5.54643629869445,-2.95009846653529));
#40140=CARTESIAN_POINT('Ctrl Pts',(-66.51072,5.60233858003336,-2.85550523338778));
#40141=CARTESIAN_POINT('Ctrl Pts',(-66.51072,5.65576594679515,-2.75945247809285));
#40142=CARTESIAN_POINT('Ctrl Pts',(-66.51072,5.69253044352725,-2.69335655343509));
#40143=CARTESIAN_POINT('Ctrl Pts',(-66.51072,5.72812290839306,-2.62656942226179));
#40144=CARTESIAN_POINT('Ctrl Pts',(-66.51072,5.76252923331074,-2.55912494345147));
#40145=CARTESIAN_POINT('Ctrl Pts',(-66.51072,5.77883595581305,-2.52715993693293));
#40146=CARTESIAN_POINT('Ctrl Pts',(-66.51072,5.79487826796475,-2.4950428726627));
#40147=CARTESIAN_POINT('Ctrl Pts',(-66.51072,5.81064158940516,-2.46280437671937));
#40148=CARTESIAN_POINT('Ctrl Pts',(-66.51072,5.88832126227673,-2.30393710828132));
#40149=CARTESIAN_POINT('Ctrl Pts',(-66.51072,5.95928765838032,-2.14201350648212));
#40150=CARTESIAN_POINT('Ctrl Pts',(-66.51072,6.02342466627868,-1.97750197757987));
#40151=CARTESIAN_POINT('Ctrl Pts',(-66.51072,6.0877724413544,-1.81244983052706));
#40152=CARTESIAN_POINT('Ctrl Pts',(-66.51072,6.14524621241747,-1.64479206150153));
#40153=CARTESIAN_POINT('Ctrl Pts',(-66.51072,6.19568512368219,-1.47497227311826));
#40154=CARTESIAN_POINT('Ctrl Pts',(-66.51072,6.23895047404685,-1.32930472282772));
#40155=CARTESIAN_POINT('Ctrl Pts',(-66.51072,6.27703911663385,-1.18204567723471));
#40156=CARTESIAN_POINT('Ctrl Pts',(-66.51072,6.30982117183241,-1.03346352641803));
#40157=CARTESIAN_POINT('Ctrl Pts',(-66.51072,6.31481496487166,-1.01082954248961));
#40158=CARTESIAN_POINT('Ctrl Pts',(-66.51072,6.31968556421223,-0.988164840915087));
#40159=CARTESIAN_POINT('Ctrl Pts',(-66.51072,6.32443245356077,-0.965470356345221));
#40160=CARTESIAN_POINT('Ctrl Pts',(-66.51072,6.32944638574867,-0.941499162091915));
#40161=CARTESIAN_POINT('Ctrl Pts',(-66.51072,6.33432061618718,-0.917502689271744));
#40162=CARTESIAN_POINT('Ctrl Pts',(-66.51072,6.33905393823772,-0.893486720876821));
#40163=CARTESIAN_POINT('Ctrl Pts',(-66.51072,6.35925666012823,-0.790981984196606));
#40164=CARTESIAN_POINT('Ctrl Pts',(-66.51072,6.37689836887655,-0.688095730530865));
#40165=CARTESIAN_POINT('Ctrl Pts',(-66.51072,6.39195662158433,-0.584920330828077));
#40166=CARTESIAN_POINT('Ctrl Pts',(-66.51072,6.41738598417301,-0.410684667488666));
#40167=CARTESIAN_POINT('Ctrl Pts',(-66.51072,6.43545071544452,-0.235625365624705));
#40168=CARTESIAN_POINT('Ctrl Pts',(-66.51072,6.44629977206506,-0.0601947746487687));
#40169=CARTESIAN_POINT('Ctrl Pts',(-66.51072,6.45728926013915,0.117506610346195));
#40170=CARTESIAN_POINT('Ctrl Pts',(-66.51072,6.46087513399998,0.29558962059473));
#40171=CARTESIAN_POINT('Ctrl Pts',(-66.51072,6.45716079669616,0.473599419439789));
#40172=CARTESIAN_POINT('Ctrl Pts',(-66.51072,6.4533746861754,0.655048953254274));
#40173=CARTESIAN_POINT('Ctrl Pts',(-66.51072,6.44200365346109,0.836423165438464));
#40174=CARTESIAN_POINT('Ctrl Pts',(-66.51072,6.42310242695258,1.01724540279636));
#40175=CARTESIAN_POINT('Ctrl Pts',(-66.51072,6.4089265070712,1.15286208081478));
#40176=CARTESIAN_POINT('Ctrl Pts',(-66.51072,6.39051371885256,1.28816845488067));
#40177=CARTESIAN_POINT('Ctrl Pts',(-66.51072,6.36786686174987,1.42296130007595));
#40178=CARTESIAN_POINT('Ctrl Pts',(-66.51072,6.36157323512551,1.46042061884357));
#40179=CARTESIAN_POINT('Ctrl Pts',(-66.51072,6.35495250829001,1.49784025576893));
#40180=CARTESIAN_POINT('Ctrl Pts',(-66.51072,6.34800450349549,1.53521578937394));
#40181=CARTESIAN_POINT('Ctrl Pts',(-66.51072,6.34388886263482,1.5573551340985));
#40182=CARTESIAN_POINT('Ctrl Pts',(-66.51072,6.33966014021218,1.57946951451518));
#40183=CARTESIAN_POINT('Ctrl Pts',(-66.51072,6.33531911437619,1.60155545740789));
#40184=CARTESIAN_POINT('Ctrl Pts',(-66.51072,6.3001676131708,1.78039660637772));
#40185=CARTESIAN_POINT('Ctrl Pts',(-66.51072,6.25764647419907,1.95742764186776));
#40186=CARTESIAN_POINT('Ctrl Pts',(-66.51072,6.20788490890828,2.13217995064111));
#40187=CARTESIAN_POINT('Ctrl Pts',(-66.51072,6.16217257165171,2.29271220939));
#40188=CARTESIAN_POINT('Ctrl Pts',(-66.51072,6.11034959729668,2.45132208138385));
#40189=CARTESIAN_POINT('Ctrl Pts',(-66.51072,6.05247743653113,2.60764785511938));
#40190=CARTESIAN_POINT('Ctrl Pts',(-66.51072,5.98976686720135,2.77704326289739));
#40191=CARTESIAN_POINT('Ctrl Pts',(-66.51072,5.91995403238247,2.94375748123564));
#40192=CARTESIAN_POINT('Ctrl Pts',(-66.51072,5.84334750123361,3.10743909866994));
#40193=CARTESIAN_POINT('Ctrl Pts',(-66.51072,5.76633331846032,3.27199172639848));
#40194=CARTESIAN_POINT('Ctrl Pts',(-66.51072,5.6824526225013,3.43348002678122));
#40195=CARTESIAN_POINT('Ctrl Pts',(-66.51072,5.59196984847498,3.59152795464669));
#40196=CARTESIAN_POINT('Ctrl Pts',(-66.51072,5.5455267417669,3.67265098450333));
#40197=CARTESIAN_POINT('Ctrl Pts',(-66.51072,5.49734350565571,3.75286725678217));
#40198=CARTESIAN_POINT('Ctrl Pts',(-66.51072,5.44745134134628,3.83212314758995));
#40199=CARTESIAN_POINT('Ctrl Pts',(-66.51072,5.43459757335987,3.85254192168203));
#40200=CARTESIAN_POINT('Ctrl Pts',(-66.51072,5.42163036231943,3.87289694046096));
#40201=CARTESIAN_POINT('Ctrl Pts',(-66.51072,5.40855021073457,3.89318726281891));
#40202=CARTESIAN_POINT('Ctrl Pts',(-66.51072,5.39793659485858,3.90965142121267));
#40203=CARTESIAN_POINT('Ctrl Pts',(-66.51072,5.38724950512193,3.92607155347971));
#40204=CARTESIAN_POINT('Ctrl Pts',(-66.51072,5.37649448582116,3.94243934362586));
#40205=CARTESIAN_POINT('Ctrl Pts',(-66.51072,5.27546351607111,4.0961958051333));
#40206=CARTESIAN_POINT('Ctrl Pts',(-66.51072,5.16831729088704,4.24552924635349));
#40207=CARTESIAN_POINT('Ctrl Pts',(-66.51072,5.0554088542436,4.39009677447249));
#40208=CARTESIAN_POINT('Ctrl Pts',(-66.51072,4.94170583266791,4.53568168608338));
#40209=CARTESIAN_POINT('Ctrl Pts',(-66.51072,4.82215887167875,4.67643400616859));
#40210=CARTESIAN_POINT('Ctrl Pts',(-66.51072,4.69707874333019,4.81198543660765));
#40211=CARTESIAN_POINT('Ctrl Pts',(-66.51072,4.57220526885852,4.94731291277843));
#40212=CARTESIAN_POINT('Ctrl Pts',(-66.51072,4.44181649197592,5.07745729021896));
#40213=CARTESIAN_POINT('Ctrl Pts',(-66.51072,4.3061778998763,5.2020247050942));
#40214=CARTESIAN_POINT('Ctrl Pts',(-66.51072,4.26374685226021,5.24099241944576));
#40215=CARTESIAN_POINT('Ctrl Pts',(-66.51072,4.22080176452851,5.27941413861846));
#40216=CARTESIAN_POINT('Ctrl Pts',(-66.51072,4.1773499785852,5.31727710454912));
#40217=CARTESIAN_POINT('Ctrl Pts',(-66.51072,4.07025321995506,5.41059895163238));
#40218=CARTESIAN_POINT('Ctrl Pts',(-66.51072,3.96007912027853,5.50052745896816));
#40219=CARTESIAN_POINT('Ctrl Pts',(-66.51072,3.84701398483213,5.58697437177063));
#40220=CARTESIAN_POINT('Ctrl Pts',(-66.51072,3.79754798807433,5.62479489612171));
#40221=CARTESIAN_POINT('Ctrl Pts',(-66.51072,3.7475284815066,5.66194883395774));
#40222=CARTESIAN_POINT('Ctrl Pts',(-66.51072,3.69697043257265,5.69842788582505));
#40223=CARTESIAN_POINT('Ctrl Pts',(-66.51072,3.66885907731644,5.71871101794891));
#40224=CARTESIAN_POINT('Ctrl Pts',(-66.51072,3.64058122006461,5.73878549233668));
#40225=CARTESIAN_POINT('Ctrl Pts',(-66.51072,3.61213938875156,5.75864980418902));
#40226=CARTESIAN_POINT('Ctrl Pts',(-66.51072,3.59288633876352,5.77209649771805));
#40227=CARTESIAN_POINT('Ctrl Pts',(-66.51072,3.57355735859509,5.78544736926076));
#40228=CARTESIAN_POINT('Ctrl Pts',(-66.51072,3.5541671769133,5.79869258258653));
#40229=CARTESIAN_POINT('Ctrl Pts',(-66.51072,3.40184184240323,5.90274429203488));
#40230=CARTESIAN_POINT('Ctrl Pts',(-66.51072,3.24554560446478,6.00041723965922));
#40231=CARTESIAN_POINT('Ctrl Pts',(-66.51072,3.08574808349221,6.09159803735488));
#40232=CARTESIAN_POINT('Ctrl Pts',(-66.51072,2.92308726372841,6.18441263929378));
#40233=CARTESIAN_POINT('Ctrl Pts',(-66.51072,2.75679806121725,6.27050079088333));
#40234=CARTESIAN_POINT('Ctrl Pts',(-66.51072,2.58733626350152,6.34970623172909));
#40235=CARTESIAN_POINT('Ctrl Pts',(-66.51072,2.41755160422378,6.42906257615722));
#40236=CARTESIAN_POINT('Ctrl Pts',(-66.51072,2.24458162584722,6.50151032688276));
#40237=CARTESIAN_POINT('Ctrl Pts',(-66.51072,2.06885406101389,6.5668498761021));
#40238=CARTESIAN_POINT('Ctrl Pts',(-66.51072,1.89493100273515,6.6315184682923));
#40239=CARTESIAN_POINT('Ctrl Pts',(-66.51072,1.71830605202983,6.68922437216728));
#40240=CARTESIAN_POINT('Ctrl Pts',(-66.51072,1.53937345115484,6.73972784852978));
#40241=CARTESIAN_POINT('Ctrl Pts',(-66.51072,1.41341886592483,6.77527835406541));
#40242=CARTESIAN_POINT('Ctrl Pts',(-66.51072,1.28632038834554,6.80725906508397));
#40243=CARTESIAN_POINT('Ctrl Pts',(-66.51072,1.15821195975198,6.83557123116185));
#40244=CARTESIAN_POINT('',(-66.51072,-6.933,-8.4904762584886E-16));
#40245=CARTESIAN_POINT('Origin',(-66.51072,0.,0.));
#40246=CARTESIAN_POINT('',(-66.51072,-4.64229328560453,5.14951358184791));
#40247=CARTESIAN_POINT('Origin',(-66.51072,0.,0.));
#40248=CARTESIAN_POINT('Ctrl Pts',(-66.51072,-4.64244039278575,5.14956429285679));
#40249=CARTESIAN_POINT('Ctrl Pts',(-66.51072,-4.77208351901737,5.020713217228));
#40250=CARTESIAN_POINT('Ctrl Pts',(-66.51072,-4.89641770167796,4.88689155878294));
#40251=CARTESIAN_POINT('Ctrl Pts',(-66.51072,-5.0150831726735,4.74832914407448));
#40252=CARTESIAN_POINT('Ctrl Pts',(-66.51072,-5.13744689549262,4.60544838217897));
#40253=CARTESIAN_POINT('Ctrl Pts',(-66.51072,-5.25378364734574,4.45752634517166));
#40254=CARTESIAN_POINT('Ctrl Pts',(-66.51072,-5.36388377718831,4.30499917290805));
#40255=CARTESIAN_POINT('Ctrl Pts',(-66.51072,-5.43302299971837,4.20921717773608));
#40256=CARTESIAN_POINT('Ctrl Pts',(-66.51072,-5.49970198987414,4.11161858692189));
#40257=CARTESIAN_POINT('Ctrl Pts',(-66.51072,-5.56385938958403,4.01230682937023));
#40258=CARTESIAN_POINT('Ctrl Pts',(-66.51072,-5.60405094939935,3.9500927361861));
#40259=CARTESIAN_POINT('Ctrl Pts',(-66.51072,-5.64325278175659,3.88720626027224));
#40260=CARTESIAN_POINT('Ctrl Pts',(-66.51072,-5.68144825171902,3.82367233499214));
#40261=CARTESIAN_POINT('Ctrl Pts',(-66.51072,-5.69807351632313,3.79601805242516));
#40262=CARTESIAN_POINT('Ctrl Pts',(-66.51072,-5.71450810167693,3.76824110117671));
#40263=CARTESIAN_POINT('Ctrl Pts',(-66.51072,-5.73075056271715,3.74034352052681));
#40264=CARTESIAN_POINT('Ctrl Pts',(-66.51072,-5.74433450921565,3.7170121274548));
#40265=CARTESIAN_POINT('Ctrl Pts',(-66.51072,-5.75777909807329,3.69360490600033));
#40266=CARTESIAN_POINT('Ctrl Pts',(-66.51072,-5.77108339705107,3.67012387995191));
#40267=CARTESIAN_POINT('Ctrl Pts',(-66.51072,-5.86309962123462,3.50772258691574));
#40268=CARTESIAN_POINT('Ctrl Pts',(-66.51072,-5.94841524727953,3.34178186612013));
#40269=CARTESIAN_POINT('Ctrl Pts',(-66.51072,-6.02682780981107,3.17272981240304));
#40270=CARTESIAN_POINT('Ctrl Pts',(-66.51072,-6.10484904738322,3.00452142819397));
#40271=CARTESIAN_POINT('Ctrl Pts',(-66.51072,-6.17603618743261,2.83323201149326));
#40272=CARTESIAN_POINT('Ctrl Pts',(-66.51072,-6.24014138299806,2.65926639348439));
#40273=CARTESIAN_POINT('Ctrl Pts',(-66.51072,-6.29582315113101,2.50815987053205));
#40274=CARTESIAN_POINT('Ctrl Pts',(-66.51072,-6.34616120131628,2.35503373144777));
#40275=CARTESIAN_POINT('Ctrl Pts',(-66.51072,-6.39096108360734,2.2001487288792));
#40276=CARTESIAN_POINT('Ctrl Pts',(-66.51072,-6.39811169003876,2.17542719750771));
#40277=CARTESIAN_POINT('Ctrl Pts',(-66.51072,-6.40512114147276,2.15066085480165));
#40278=CARTESIAN_POINT('Ctrl Pts',(-66.51072,-6.41198857303617,2.12585076007206));
#40279=CARTESIAN_POINT('Ctrl Pts',(-66.51072,-6.41878698647798,2.10129000836384));
#40280=CARTESIAN_POINT('Ctrl Pts',(-66.51072,-6.42544420594425,2.07669356320528));
#40281=CARTESIAN_POINT('Ctrl Pts',(-66.51072,-6.43195802548163,2.05206883857791));
#40282=CARTESIAN_POINT('Ctrl Pts',(-66.51072,-6.46008886107403,1.94572354055036));
#40283=CARTESIAN_POINT('Ctrl Pts',(-66.51072,-6.48555598077592,1.83881391444392));
#40284=CARTESIAN_POINT('Ctrl Pts',(-66.51072,-6.50831913745385,1.73142657942197));
#40285=CARTESIAN_POINT('Ctrl Pts',(-66.51072,-6.54628591077437,1.55231475130603));
#40286=CARTESIAN_POINT('Ctrl Pts',(-66.51072,-6.57673339401698,1.37187431457994));
#40287=CARTESIAN_POINT('Ctrl Pts',(-66.51072,-6.59972567046035,1.19057384607931));
#40288=CARTESIAN_POINT('Ctrl Pts',(-66.51072,-6.62284513108582,1.00827049507335));
#40289=CARTESIAN_POINT('Ctrl Pts',(-66.51072,-6.63842664969771,0.825096833283679));
#40290=CARTESIAN_POINT('Ctrl Pts',(-66.51072,-6.64648284652764,0.641526136489152));
#40291=CARTESIAN_POINT('Ctrl Pts',(-66.51072,-6.65456709998406,0.457316133756397));
#40292=CARTESIAN_POINT('Ctrl Pts',(-66.51072,-6.65507349012932,0.272705573461058));
#40293=CARTESIAN_POINT('Ctrl Pts',(-66.51072,-6.64796251940445,0.0881807892318182));
#40294=CARTESIAN_POINT('Ctrl Pts',(-66.51072,-6.6426292913608,-0.0502127989401112));
#40295=CARTESIAN_POINT('Ctrl Pts',(-66.51072,-6.63301022104618,-0.188558041365239));
#40296=CARTESIAN_POINT('Ctrl Pts',(-66.51072,-6.61906962965593,-0.326642930935964));
#40297=CARTESIAN_POINT('Ctrl Pts',(-66.51072,-6.61533149919028,-0.363670006624603));
#40298=CARTESIAN_POINT('Ctrl Pts',(-66.51072,-6.61128254879057,-0.400678319771744));
#40299=CARTESIAN_POINT('Ctrl Pts',(-66.51072,-6.60692189323121,-0.437663682307064));
#40300=CARTESIAN_POINT('Ctrl Pts',(-66.51072,-6.6043408934228,-0.459554705874133));
#40301=CARTESIAN_POINT('Ctrl Pts',(-66.51072,-6.60165067268052,-0.481437465497591));
#40302=CARTESIAN_POINT('Ctrl Pts',(-66.51072,-6.59885297598377,-0.503297068535974));
#40303=CARTESIAN_POINT('Ctrl Pts',(-66.51072,-6.57583263441499,-0.683164860883122));
#40304=CARTESIAN_POINT('Ctrl Pts',(-66.51072,-6.54551210047545,-0.861707159351045));
#40305=CARTESIAN_POINT('Ctrl Pts',(-66.51072,-6.50792768344902,-1.03847560235939));
#40306=CARTESIAN_POINT('Ctrl Pts',(-66.51072,-6.47145771003767,-1.21000255226383));
#40307=CARTESIAN_POINT('Ctrl Pts',(-66.51072,-6.42814792670735,-1.37985987693613));
#40308=CARTESIAN_POINT('Ctrl Pts',(-66.51072,-6.37798556320937,-1.54762840486411));
#40309=CARTESIAN_POINT('Ctrl Pts',(-66.51072,-6.32617544917501,-1.72090785099064));
#40310=CARTESIAN_POINT('Ctrl Pts',(-66.51072,-6.26705505663415,-1.89195973976835));
#40311=CARTESIAN_POINT('Ctrl Pts',(-66.51072,-6.20086142651017,-2.06037121308545));
#40312=CARTESIAN_POINT('Ctrl Pts',(-66.51072,-6.13492183835158,-2.22813634654181));
#40313=CARTESIAN_POINT('Ctrl Pts',(-66.51072,-6.06196276652256,-2.39328189639218));
#40314=CARTESIAN_POINT('Ctrl Pts',(-66.51072,-5.98217662776493,-2.55536986618945));
#40315=CARTESIAN_POINT('Ctrl Pts',(-66.51072,-5.94262418782639,-2.63572185201049));
#40316=CARTESIAN_POINT('Ctrl Pts',(-66.51072,-5.90139339549068,-2.71532192202713));
#40317=CARTESIAN_POINT('Ctrl Pts',(-66.51072,-5.85850434682744,-2.79411327911155));
#40318=CARTESIAN_POINT('Ctrl Pts',(-66.51072,-5.84639974950909,-2.81635060261018));
#40319=CARTESIAN_POINT('Ctrl Pts',(-66.51072,-5.83416305274489,-2.83852349344844));
#40320=CARTESIAN_POINT('Ctrl Pts',(-66.51072,-5.8217946791383,-2.8606306375173));
#40321=CARTESIAN_POINT('Ctrl Pts',(-66.51072,-5.81057979104184,-2.88067604969119));
#40322=CARTESIAN_POINT('Ctrl Pts',(-66.51072,-5.79926047745952,-2.90066050695198));
#40323=CARTESIAN_POINT('Ctrl Pts',(-66.51072,-5.78784025721056,-2.92057804100683));
#40324=CARTESIAN_POINT('Ctrl Pts',(-66.51072,-5.69892412862028,-3.0756529853261));
#40325=CARTESIAN_POINT('Ctrl Pts',(-66.51072,-5.60383915857374,-3.22677285815348));
#40326=CARTESIAN_POINT('Ctrl Pts',(-66.51072,-5.5028480490352,-3.37356178930185));
#40327=CARTESIAN_POINT('Ctrl Pts',(-66.51072,-5.40197092766091,-3.52018504051196));
#40328=CARTESIAN_POINT('Ctrl Pts',(-66.51072,-5.29520055505474,-3.66248771572367));
#40329=CARTESIAN_POINT('Ctrl Pts',(-66.51072,-5.18275615628646,-3.80006564228537));
#40330=CARTESIAN_POINT('Ctrl Pts',(-66.51072,-5.0716905546549,-3.93595658351658));
#40331=CARTESIAN_POINT('Ctrl Pts',(-66.51072,-4.9550887580849,-4.06723843117073));
#40332=CARTESIAN_POINT('Ctrl Pts',(-66.51072,-4.83312726292506,-4.19348483441543));
#40333=CARTESIAN_POINT('Ctrl Pts',(-66.51072,-4.80127883984523,-4.22645219725052));
#40334=CARTESIAN_POINT('Ctrl Pts',(-66.51072,-4.76906476512282,-4.2590759661899));
#40335=CARTESIAN_POINT('Ctrl Pts',(-66.51072,-4.73648784413042,-4.29134806370339));
#40336=CARTESIAN_POINT('Ctrl Pts',(-66.51072,-4.64348208285574,-4.38348356656057));
#40337=CARTESIAN_POINT('Ctrl Pts',(-66.51072,-4.54751927645066,-4.47275368008218));
#40338=CARTESIAN_POINT('Ctrl Pts',(-66.51072,-4.44874982948056,-4.5590458483051));
#40339=CARTESIAN_POINT('Ctrl Pts',(-66.51072,-4.40553819643115,-4.59679867190263));
#40340=CARTESIAN_POINT('Ctrl Pts',(-66.51072,-4.36178927514179,-4.63398131817575));
#40341=CARTESIAN_POINT('Ctrl Pts',(-66.51072,-4.31751533581933,-4.6705834958155));
#40342=CARTESIAN_POINT('Ctrl Pts',(-66.51072,-4.29129360863923,-4.69226153781842));
#40343=CARTESIAN_POINT('Ctrl Pts',(-66.51072,-4.26488771593151,-4.71373595681972));
#40344=CARTESIAN_POINT('Ctrl Pts',(-66.51072,-4.23830018127736,-4.73500452368828));
#40345=CARTESIAN_POINT('Ctrl Pts',(-66.51072,-4.21784594893157,-4.75136678570506));
#40346=CARTESIAN_POINT('Ctrl Pts',(-66.51072,-4.19728221990606,-4.7676086836443));
#40347=CARTESIAN_POINT('Ctrl Pts',(-66.51072,-4.17662859394966,-4.78371502962124));
#40348=CARTESIAN_POINT('Ctrl Pts',(-66.51072,-4.0386441282523,-4.89131964823186));
#40349=CARTESIAN_POINT('Ctrl Pts',(-66.51072,-3.89647958119171,-4.99301559213152));
#40350=CARTESIAN_POINT('Ctrl Pts',(-66.51072,-3.75054944970173,-5.08861922337019));
#40351=CARTESIAN_POINT('Ctrl Pts',(-66.51072,-3.6038038756398,-5.18475707787137));
#40352=CARTESIAN_POINT('Ctrl Pts',(-66.51072,-3.45324987084959,-5.27473470522527));
#40353=CARTESIAN_POINT('Ctrl Pts',(-66.51072,-3.29928025831541,-5.35832163598663));
#40354=CARTESIAN_POINT('Ctrl Pts',(-66.51072,-3.146240127214,-5.44140397042612));
#40355=CARTESIAN_POINT('Ctrl Pts',(-66.51072,-2.98982483785502,-5.51817280831344));
#40356=CARTESIAN_POINT('Ctrl Pts',(-66.51072,-2.8304017813007,-5.58835410868057));
#40357=CARTESIAN_POINT('Ctrl Pts',(-66.51072,-2.67408193606954,-5.65716931175488));
#40358=CARTESIAN_POINT('Ctrl Pts',(-66.51072,-2.51486966171192,-5.71965108202682));
#40359=CARTESIAN_POINT('Ctrl Pts',(-66.51072,-2.35310307851583,-5.77549214185151));
#40360=CARTESIAN_POINT('Ctrl Pts',(-66.51072,-2.25436054710213,-5.80957759692495));
#40361=CARTESIAN_POINT('Ctrl Pts',(-66.51072,-2.15466618504803,-5.84118782884412));
#40362=CARTESIAN_POINT('Ctrl Pts',(-66.51072,-2.05409679149563,-5.87024334535353));
#40363=CARTESIAN_POINT('Ctrl Pts',(-86.9228037546341,-4.16423880285026,
4.61932741374069));
#40364=CARTESIAN_POINT('Ctrl Pts',(-86.8897744928952,-4.93115421869368,
3.92796725519045));
#40365=CARTESIAN_POINT('Ctrl Pts',(-86.8237159694174,-6.11319170164878,
2.15655013100907));
#40366=CARTESIAN_POINT('Ctrl Pts',(-86.7246281842008,-6.40055386810954,
-1.02634989594538));
#40367=CARTESIAN_POINT('Ctrl Pts',(-86.625540398984,-5.13269180441595,-3.9591844580739));
#40368=CARTESIAN_POINT('Ctrl Pts',(-86.5264526137674,-2.61763940474365,
-5.93031580654633));
#40369=CARTESIAN_POINT('Ctrl Pts',(-86.4273648285507,0.533459855123279,
-6.46029588895267));
#40370=CARTESIAN_POINT('Ctrl Pts',(-86.3282770433341,3.55493808738742,-5.42058662271333));
#40371=CARTESIAN_POINT('Ctrl Pts',(-86.2291892581173,5.71261075920097,-3.06370552006469));
#40372=CARTESIAN_POINT('Ctrl Pts',(-86.1301014729008,6.48219330078747,0.0375972645595515));
#40373=CARTESIAN_POINT('Ctrl Pts',(-86.031013687684,5.67668603654431,3.12977391169855));
#40374=CARTESIAN_POINT('Ctrl Pts',(-85.9319259024675,3.49181736371615,5.46145112616022));
#40375=CARTESIAN_POINT('Ctrl Pts',(-85.8328381172506,0.45848197210095,6.46606838804796));
#40376=CARTESIAN_POINT('Ctrl Pts',(-85.7337503320341,-2.68625859143277,
5.89951319007443));
#40377=CARTESIAN_POINT('Ctrl Pts',(-85.6346625468174,-5.17827294326576,
3.89945285036088));
#40378=CARTESIAN_POINT('Ctrl Pts',(-85.5355747616006,-6.41203366928947,
0.951875425404776));
#40379=CARTESIAN_POINT('Ctrl Pts',(-85.4364869763841,-6.08775282190871,
-2.22699532849796));
#40380=CARTESIAN_POINT('Ctrl Pts',(-85.3373991911673,-4.28422646215156,
-4.86473497443532));
#40381=CARTESIAN_POINT('Ctrl Pts',(-85.2383114059508,-1.43968826503564,
-6.32040665848384));
#40382=CARTESIAN_POINT('Ctrl Pts',(-85.139223620734,1.75467563421941,-6.24030096387333));
#40383=CARTESIAN_POINT('Ctrl Pts',(-85.0401358355174,4.52267595876155,-4.64388251792204));
#40384=CARTESIAN_POINT('Ctrl Pts',(-84.9410480503007,6.19172428905613,-1.919060449145));
#40385=CARTESIAN_POINT('Ctrl Pts',(-84.8419602650839,6.35626338222264,1.27206858835509));
#40386=CARTESIAN_POINT('Ctrl Pts',(-84.7428724798673,4.9763123584096,4.15410134539831));
#40387=CARTESIAN_POINT('Ctrl Pts',(-84.6437846946507,2.38718153906689,6.02674099139694));
#40388=CARTESIAN_POINT('Ctrl Pts',(-84.544696909434,-0.782003641280745,
6.43496021602791));
#40389=CARTESIAN_POINT('Ctrl Pts',(-84.4456091242173,-3.76117201100048,
5.27956700696203));
#40390=CARTESIAN_POINT('Ctrl Pts',(-84.3465213390006,-5.82642403552263,
2.84130702942041));
#40391=CARTESIAN_POINT('Ctrl Pts',(-84.247433553784,-6.47593007859897,-0.287353952968906));
#40392=CARTESIAN_POINT('Ctrl Pts',(-84.1483457685672,-5.55186853905296,
-3.34619162665173));
#40393=CARTESIAN_POINT('Ctrl Pts',(-84.0492579833507,-3.27877446672824,
-5.59194784252432));
#40394=CARTESIAN_POINT('Ctrl Pts',(-83.950170198134,-0.208980437956675,
-6.47893277120133));
#40395=CARTESIAN_POINT('Ctrl Pts',(-83.8510824129173,2.91159314503785,-5.79162050163479));
#40396=CARTESIAN_POINT('Ctrl Pts',(-83.7519946277006,5.32468710252559,-3.6970190609988));
#40397=CARTESIAN_POINT('Ctrl Pts',(-83.652906842484,6.44395068963483,-0.704089615563853));
#40398=CARTESIAN_POINT('Ctrl Pts',(-83.5538190572673,5.9974172736645,2.4599245359849));
#40399=CARTESIAN_POINT('Ctrl Pts',(-83.4547312720506,4.09358872220742,5.02620871538443));
#40400=CARTESIAN_POINT('Ctrl Pts',(-83.3556434868339,1.19507084710563,6.37118892731869));
#40401=CARTESIAN_POINT('Ctrl Pts',(-83.2565557016173,-1.99383384828571,
6.16805230705936));
#40402=CARTESIAN_POINT('Ctrl Pts',(-83.1574679164006,-4.69826260420316,
4.46615843641225));
#40403=CARTESIAN_POINT('Ctrl Pts',(-83.058380131184,-6.26107407289102,1.67904560121576));
#40404=CARTESIAN_POINT('Ctrl Pts',(-82.9592923459673,-6.30252520045134,
-1.51605368469123));
#40405=CARTESIAN_POINT('Ctrl Pts',(-82.8602045607506,-4.8125438968831,-4.34277145585205));
#40406=CARTESIAN_POINT('Ctrl Pts',(-82.7611167755339,-2.15317642419824,
-6.11425170920097));
#40407=CARTESIAN_POINT('Ctrl Pts',(-82.6620289903173,1.02938518116893,-6.40004756435293));
#40408=CARTESIAN_POINT('Ctrl Pts',(-82.5629412051006,3.96181944861569,-5.13071431028474));
#40409=CARTESIAN_POINT('Ctrl Pts',(-82.4638534198839,5.93158262837659,-2.61468357548884));
#40410=CARTESIAN_POINT('Ctrl Pts',(-82.3647656346672,6.46004764333774,0.536681584365129));
#40411=CARTESIAN_POINT('Ctrl Pts',(-82.2656778494506,5.41880430283928,3.55764003304445));
#40412=CARTESIAN_POINT('Ctrl Pts',(-82.1665900642338,3.06086132475543,5.71413778516117));
#40413=CARTESIAN_POINT('Ctrl Pts',(-82.0675022790172,-0.0408315235521791,
6.4821736681359));
#40414=CARTESIAN_POINT('Ctrl Pts',(-81.9684144938005,-3.13260283765064,
5.67512485666467));
#40415=CARTESIAN_POINT('Ctrl Pts',(-81.8693267085839,-5.46319201810528,
3.48909381509022));
#40416=CARTESIAN_POINT('Ctrl Pts',(-81.7702389233672,-6.46629591799175,
0.455257924866117));
#40417=CARTESIAN_POINT('Ctrl Pts',(-81.6711511381505,-5.89817321217138,
-2.68919977621855));
#40418=CARTESIAN_POINT('Ctrl Pts',(-81.5720633529339,-3.89687039929076,
-5.18021657542632));
#40419=CARTESIAN_POINT('Ctrl Pts',(-81.4729755677172,-0.948678281001003,
-6.41250748119229));
#40420=CARTESIAN_POINT('Ctrl Pts',(-81.3738877825005,2.23003043817884,-6.08664167846161));
#40421=CARTESIAN_POINT('Ctrl Pts',(-81.274799997284,4.86687048935458,-4.28180035931612));
#40422=CARTESIAN_POINT('Ctrl Pts',(-81.1757122120671,6.32112370930806,-1.43653671335388));
#40423=CARTESIAN_POINT('Ctrl Pts',(-81.0766244268506,6.23942530007697,1.75778684770072));
#40424=CARTESIAN_POINT('Ctrl Pts',(-80.9775366416338,4.64162692262079,4.52499084953681));
#40425=CARTESIAN_POINT('Ctrl Pts',(-80.8784488564173,1.91597299894771,6.19268036834564));
#40426=CARTESIAN_POINT('Ctrl Pts',(-80.7793610712004,-1.27523768085627,
6.35562833514629));
#40427=CARTESIAN_POINT('Ctrl Pts',(-80.6802732859839,-4.15658203252233,
4.97424049319116));
#40428=CARTESIAN_POINT('Ctrl Pts',(-80.5811855007671,-6.02793049765148,
2.38417629228067));
#40429=CARTESIAN_POINT('Ctrl Pts',(-80.4820977155505,-6.4345695069531,-0.785212033389358));
#40430=CARTESIAN_POINT('Ctrl Pts',(-80.3830099303339,-5.27769101971328,
-3.76380395047722));
#40431=CARTESIAN_POINT('Ctrl Pts',(-80.2839221451171,-2.83840160478908,
-5.82783999498278));
#40432=CARTESIAN_POINT('Ctrl Pts',(-80.1848343599005,0.290582834254973,
-6.47578599813385));
#40433=CARTESIAN_POINT('Ctrl Pts',(-80.0857465746839,3.34895938802227,-5.55019942835999));
#40434=CARTESIAN_POINT('Ctrl Pts',(-79.9866587894671,5.59358195362901,-3.27598589820315));
#40435=CARTESIAN_POINT('Ctrl Pts',(-79.8875710042505,6.47903616408986,-0.205749997827326));
#40436=CARTESIAN_POINT('Ctrl Pts',(-79.7884832190337,5.79016805316885,2.91448050143638));
#40437=CARTESIAN_POINT('Ctrl Pts',(-79.6893954338172,3.69436369744359,5.32652978478494));
#40438=CARTESIAN_POINT('Ctrl Pts',(-79.5903076486004,0.700876556055815,
6.44430094970444));
#40439=CARTESIAN_POINT('Ctrl Pts',(-79.4912198633839,-2.46291455937789,
5.99619000285969));
#40440=CARTESIAN_POINT('Ctrl Pts',(-79.392132078167,-5.0282491654969,4.09108213152337));
#40441=CARTESIAN_POINT('Ctrl Pts',(-79.2930442929505,-6.37178400105954,
1.19189400578732));
#40442=CARTESIAN_POINT('Ctrl Pts',(-79.1939565077337,-6.16705740917563,
-1.99690900872377));
#40443=CARTESIAN_POINT('Ctrl Pts',(-79.0948687225172,-4.46381531427285,
-4.7004888593904));
#40444=CARTESIAN_POINT('Ctrl Pts',(-78.9957809373004,-1.67592360331519,
-6.26191047149678));
#40445=CARTESIAN_POINT('Ctrl Pts',(-78.8966931520838,1.5191959530824,-6.30176850838938));
#40446=CARTESIAN_POINT('Ctrl Pts',(-78.797605366867,4.34517046399522,-4.81037798057634));
#40447=CARTESIAN_POINT('Ctrl Pts',(-78.6985175816505,6.11532452902266,-2.15012757340671));
#40448=CARTESIAN_POINT('Ctrl Pts',(-78.5994297964337,6.39953351445713,1.03257613497986));
#40449=CARTESIAN_POINT('Ctrl Pts',(-78.5003420112172,5.12873829817387,3.96437714477757));
#40450=CARTESIAN_POINT('Ctrl Pts',(-78.4012542260003,2.61172574664976,5.93288557967174));
#40451=CARTESIAN_POINT('Ctrl Pts',(-78.3021664407838,-0.539902515628905,
6.45977924938676));
#40452=CARTESIAN_POINT('Ctrl Pts',(-78.2030786555671,-3.5603414219296,5.41702977991466));
#40453=CARTESIAN_POINT('Ctrl Pts',(-78.1039908703504,-5.71566322896938,
3.0580118590675));
#40454=CARTESIAN_POINT('Ctrl Pts',(-78.0049030851337,-6.4821525036734,-0.0440635485496543));
#40455=CARTESIAN_POINT('Ctrl Pts',(-77.9058152999171,-5.67356222662317,
-3.13543208152));
#40456=CARTESIAN_POINT('Ctrl Pts',(-77.8067275147004,-3.48636941843915,
-5.46493101103411));
#40457=CARTESIAN_POINT('Ctrl Pts',(-77.7076397294838,-0.452033754894525,
-6.46652210710101));
#40458=CARTESIAN_POINT('Ctrl Pts',(-77.608551944267,2.69214028774311,-5.89683163642142));
#40459=CARTESIAN_POINT('Ctrl Pts',(-77.5094641590505,5.18215892208465,-3.89428704430587));
#40460=CARTESIAN_POINT('Ctrl Pts',(-77.4103763738337,6.41297969776877,-0.945480868762339));
#40461=CARTESIAN_POINT('Ctrl Pts',(-77.3112885886171,6.08552902241152,2.23306497768811));
#40462=CARTESIAN_POINT('Ctrl Pts',(-77.2122008034003,4.27937319172577,4.8690048021263));
#40463=CARTESIAN_POINT('Ctrl Pts',(-77.1131130181838,1.43338480467962,6.32183918483408));
#40464=CARTESIAN_POINT('Ctrl Pts',(-77.014025232967,-1.76089762425562,6.2385480870216));
#40465=CARTESIAN_POINT('Ctrl Pts',(-76.9149374477504,-4.52730461534429,
4.63937017245579));
#40466=CARTESIAN_POINT('Ctrl Pts',(-76.8158496625337,-6.19363490812165,
1.91288507289043));
#40467=CARTESIAN_POINT('Ctrl Pts',(-76.7167618773171,-6.35499170802218,
-1.27840645655423));
#40468=CARTESIAN_POINT('Ctrl Pts',(-76.6176740921003,-4.97216739135669,
-4.15906168618827));
#40469=CARTESIAN_POINT('Ctrl Pts',(-76.5185863068837,-2.38117045277481,
-6.02911850538885));
#40470=CARTESIAN_POINT('Ctrl Pts',(-76.419498521667,0.788420230289574,-6.43417719818628));
#40471=CARTESIAN_POINT('Ctrl Pts',(-76.3204107364504,3.76643495425477,-5.27581372041868));
#40472=CARTESIAN_POINT('Ctrl Pts',(-76.2213229512337,5.82925450561374,-2.83549547451091));
#40473=CARTESIAN_POINT('Ctrl Pts',(-76.122235166017,6.47564030775746,0.293811643297502));
#40474=CARTESIAN_POINT('Ctrl Pts',(-76.0231473808003,5.54852893786079,3.3517263168271));
#40475=CARTESIAN_POINT('Ctrl Pts',(-75.9240595955837,3.27319651525233,5.59521467414165));
#40476=CARTESIAN_POINT('Ctrl Pts',(-75.824971810367,0.202519506547572,6.47913794625935));
#40477=CARTESIAN_POINT('Ctrl Pts',(-75.7258840251503,-2.91736713328106,
5.78871416523925));
#40478=CARTESIAN_POINT('Ctrl Pts',(-75.6267962399337,-5.32837114284346,
3.69170741545199));
#40479=CARTESIAN_POINT('Ctrl Pts',(-75.527708454717,-6.44464960768997,0.697663322306493));
#40480=CARTESIAN_POINT('Ctrl Pts',(-75.4286206695003,-5.99496124137334,
-2.4659039704785));
#40481=CARTESIAN_POINT('Ctrl Pts',(-75.3295328842836,-4.08857452377673,
-5.03028836556254));
#40482=CARTESIAN_POINT('Ctrl Pts',(-75.230445099067,-1.18871686815845,-6.37237749074438));
#40483=CARTESIAN_POINT('Ctrl Pts',(-75.1313573138503,1.99998367272066,-6.1660609781319));
#40484=CARTESIAN_POINT('Ctrl Pts',(-75.0322695286336,4.70271394601358,-4.46147108240762));
#40485=CARTESIAN_POINT('Ctrl Pts',(-74.933181743417,6.26274531336161,-1.67280118877204));
#40486=CARTESIAN_POINT('Ctrl Pts',(-74.8340939582003,6.30101024967761,1.52233784379415));
#40487=CARTESIAN_POINT('Ctrl Pts',(-74.7350061729836,4.8082108683866,4.34756839190818));
#40488=CARTESIAN_POINT('Ctrl Pts',(-74.635918387767,2.14707818808318,6.11639582854541));
#40489=CARTESIAN_POINT('Ctrl Pts',(-74.5368306025503,-1.03576683208741,
6.39901787360667));
#40490=CARTESIAN_POINT('Ctrl Pts',(-74.4377428173336,-3.96693385537629,
5.1267610110341));
#40491=CARTESIAN_POINT('Ctrl Pts',(-74.338655032117,-5.93418705602312,2.60876726852318));
#40492=CARTESIAN_POINT('Ctrl Pts',(-74.2395672469002,-6.45950924950371,
-0.543123312670282));
#40493=CARTESIAN_POINT('Ctrl Pts',(-74.1404794616836,-5.41525391029054,
-3.5630419256968));
#40494=CARTESIAN_POINT('Ctrl Pts',(-74.0413916764669,-3.05516163314319,
-5.71718725183634));
#40495=CARTESIAN_POINT('Ctrl Pts',(-73.9423038912502,0.047295562592674,
-6.48212972771674));
#40496=CARTESIAN_POINT('Ctrl Pts',(-73.8432161060336,3.13826054590585,-5.67199818610696));
#40497=CARTESIAN_POINT('Ctrl Pts',(-73.744128320817,5.4666686453549,-3.48364415506002));
#40498=CARTESIAN_POINT('Ctrl Pts',(-73.6450405356003,6.4667466886019,-0.448809472545249));
#40499=CARTESIAN_POINT('Ctrl Pts',(-73.5459527503835,5.89548859469092,2.6950801299886));
#40500=CARTESIAN_POINT('Ctrl Pts',(-73.446864965167,3.89170272118268,5.18409998043338));
#40501=CARTESIAN_POINT('Ctrl Pts',(-73.3477771799502,0.94228322147271,6.4134503200478));
#40502=CARTESIAN_POINT('Ctrl Pts',(-73.2486893947337,-2.23609896204665,
6.0844148534698));
#40503=CARTESIAN_POINT('Ctrl Pts',(-73.1496016095169,-4.87113790444004,
4.27694496026283));
#40504=CARTESIAN_POINT('Ctrl Pts',(-73.0505138243002,-6.32255308872057,
1.43023253965916));
#40505=CARTESIAN_POINT('Ctrl Pts',(-72.9514260390836,-6.23766932303337,
-1.76400796304286));
#40506=CARTESIAN_POINT('Ctrl Pts',(-72.8523382538668,-4.63711226892121,
-4.52961725564207));
#40507=CARTESIAN_POINT('Ctrl Pts',(-72.7532504686503,-1.90979667128091,
-6.19458790813032));
#40508=CARTESIAN_POINT('Ctrl Pts',(-72.6541626834335,1.28157491443408,-6.35435350101671));
#40509=CARTESIAN_POINT('Ctrl Pts',(-72.5550748982169,4.16154030589149,-4.97009305341768));
#40510=CARTESIAN_POINT('Ctrl Pts',(-72.4559871130002,6.03030501425848,-2.37816402129864));
#40511=CARTESIAN_POINT('Ctrl Pts',(-72.3568993277835,6.4337832898522,0.791628231184674));
#40512=CARTESIAN_POINT('Ctrl Pts',(-72.2578115425668,5.27393510953157,3.76906502167849));
#40513=CARTESIAN_POINT('Ctrl Pts',(-72.1587237573503,2.83258863931502,5.83066756706414));
#40514=CARTESIAN_POINT('Ctrl Pts',(-72.0596359721335,-0.297040379296998,
6.47549300750585));
#40515=CARTESIAN_POINT('Ctrl Pts',(-71.9605481869169,-3.35449241237668,
5.54685706797077));
#40516=CARTESIAN_POINT('Ctrl Pts',(-71.8614604017001,-5.59684600365713,
3.27040631856919));
#40517=CARTESIAN_POINT('Ctrl Pts',(-71.7623726164835,-6.47923811768414,
0.19928896492046));
#40518=CARTESIAN_POINT('Ctrl Pts',(-71.6632848312669,-5.78725883820755,
-2.92025303985438));
#40519=CARTESIAN_POINT('Ctrl Pts',(-71.5641970460501,-3.68905021568418,
-5.33021117624344));
#40520=CARTESIAN_POINT('Ctrl Pts',(-71.4651092608335,-0.694449915114697,
-6.44499666350474));
#40521=CARTESIAN_POINT('Ctrl Pts',(-71.3660214756168,2.46889276854356,-5.99373098951091));
#40522=CARTESIAN_POINT('Ctrl Pts',(-71.2669336904001,5.03232631507441,-4.0860658995909));
#40523=CARTESIAN_POINT('Ctrl Pts',(-71.1678459051835,6.37296939622566,-1.1855394350089));
#40524=CARTESIAN_POINT('Ctrl Pts',(-71.0687581199668,6.16506301417589,2.00305783951203));
#40525=CARTESIAN_POINT('Ctrl Pts',(-70.9696703347502,4.4591257413993,4.70493786351959));
#40526=CARTESIAN_POINT('Ctrl Pts',(-70.8705825495335,1.66967835836243,6.26357859827801));
#40527=CARTESIAN_POINT('Ctrl Pts',(-70.7714947643168,-1.5254793560455,6.30025042450449));
#40528=CARTESIAN_POINT('Ctrl Pts',(-70.6724069791001,-4.34996523899484,
4.8060425608526));
#40529=CARTESIAN_POINT('Ctrl Pts',(-70.5733191938834,-6.11746560750284,
2.14402826898574));
#40530=CARTESIAN_POINT('Ctrl Pts',(-70.4742314086668,-6.39850064192973,
-1.03895727169834));
#40531=CARTESIAN_POINT('Ctrl Pts',(-70.3751436234501,-5.12478244935701,
-3.96948957977628));
#40532=CARTESIAN_POINT('Ctrl Pts',(-70.2760558382335,-2.60580814184455,
-5.93548705710717));
#40533=CARTESIAN_POINT('Ctrl Pts',(-70.1769680530168,0.546343974688648,
-6.45923764375577));
#40534=CARTESIAN_POINT('Ctrl Pts',(-70.0778802678002,3.56574154367478,-5.4134766944083));
#40535=CARTESIAN_POINT('Ctrl Pts',(-69.9787924825834,5.71870985338321,-3.05231064769102));
#40536=CARTESIAN_POINT('Ctrl Pts',(-69.8797046973668,6.48210534027158,0.0505275648778713));
#40537=CARTESIAN_POINT('Ctrl Pts',(-69.7806169121501,5.67043273550486,3.14108823010512));
#40538=CARTESIAN_POINT('Ctrl Pts',(-69.6815291269334,3.4809180256302,5.46840492063578));
#40539=CARTESIAN_POINT('Ctrl Pts',(-69.5824413417167,0.445585078619785,
6.46696966243845));
#40540=CARTESIAN_POINT('Ctrl Pts',(-69.4833535565002,-2.69801930222453,
5.89414408731404));
#40541=CARTESIAN_POINT('Ctrl Pts',(-69.3842657712834,-5.18603974998983,
3.88911743056271));
#40542=CARTESIAN_POINT('Ctrl Pts',(-69.2851779860668,-6.41391934791292,
0.939085339928392));
#40543=CARTESIAN_POINT('Ctrl Pts',(-69.1860902008501,-6.08329917191227,
-2.23913239050336));
#40544=CARTESIAN_POINT('Ctrl Pts',(-69.0870024156334,-4.27451566553321,
-4.87326979575939));
#40545=CARTESIAN_POINT('Ctrl Pts',(-68.9879146304167,-1.42707991907126,
-6.32326542080269));
#40546=CARTESIAN_POINT('Ctrl Pts',(-68.8888268452001,1.76711786327968,-6.23678900830517));
#40547=CARTESIAN_POINT('Ctrl Pts',(-68.7897390599834,4.5319287698749,-4.63485321262994));
#40548=CARTESIAN_POINT('Ctrl Pts',(-68.6906512747668,6.19553936809527,-1.90670779478191));
#40549=CARTESIAN_POINT('Ctrl Pts',(-68.5915634895501,6.35371371436876,1.28474305349599));
#40550=CARTESIAN_POINT('Ctrl Pts',(-68.4924757043333,4.96801747972696,4.16401789144663));
#40551=CARTESIAN_POINT('Ctrl Pts',(-68.3933879191168,2.37515699892946,6.03149002309199));
#40552=CARTESIAN_POINT('Ctrl Pts',(-68.2943001338999,-0.794836035946308,
6.43338778381987));
#40553=CARTESIAN_POINT('Ctrl Pts',(-68.1952123486834,-3.77169415073787,
5.27205518392761));
#40554=CARTESIAN_POINT('Ctrl Pts',(-68.0961245634667,-5.83207918173385,
2.82968110720637));
#40555=CARTESIAN_POINT('Ctrl Pts',(-67.99703677825,-6.47534409183691,-0.300269056217778));
#40556=CARTESIAN_POINT('Ctrl Pts',(-67.8979489930334,-5.54518383041795,
-3.35725764403967));
#40557=CARTESIAN_POINT('Ctrl Pts',(-67.7988612078167,-3.26761528590833,
-5.59847600248888));
#40558=CARTESIAN_POINT('Ctrl Pts',(-67.6997734226,-0.196058420264034,-6.47933655521552));
#40559=CARTESIAN_POINT('Ctrl Pts',(-67.6006856373834,2.92313831475997,-5.78580232210167));
#40560=CARTESIAN_POINT('Ctrl Pts',(-67.5015978521667,5.33204969326613,-3.6863915925369));
#40561=CARTESIAN_POINT('Ctrl Pts',(-67.4025100669501,6.44534250489529,-0.691237361863573));
#40562=CARTESIAN_POINT('Ctrl Pts',(-67.3034222817333,5.99249846114462,2.47188303450135));
#40563=CARTESIAN_POINT('Ctrl Pts',(-67.2043344965166,4.08355785429189,5.03435879238504));
#40564=CARTESIAN_POINT('Ctrl Pts',(-67.1052467113001,1.18235847344737,6.37356827685746));
#40565=CARTESIAN_POINT('Ctrl Pts',(-67.0061589260833,-2.0061249511844,6.16404616060605));
#40566=CARTESIAN_POINT('Ctrl Pts',(-66.9070711408667,-4.70717390764343,
4.4568144926439));
#40567=CARTESIAN_POINT('Ctrl Pts',(-66.80798335565,-6.26438336148857,1.66648367303066));
#40568=CARTESIAN_POINT('Ctrl Pts',(-66.7088955704333,-6.29954365018284,
-1.52847431346428));
#40569=CARTESIAN_POINT('Ctrl Pts',(-66.6098077852167,-4.80376045256683,
-4.35266662668044));
#40570=CARTESIAN_POINT('Ctrl Pts',(-66.5437492617389,-3.02869324528072,
-5.529215668825));
#40571=CARTESIAN_POINT('Ctrl Pts',(-66.51072,-2.05409679149563,-5.87024334535353));
#40572=CARTESIAN_POINT('Ctrl Pts',(-86.7854425030894,-4.32354126137468,
4.79603923277341));
#40573=CARTESIAN_POINT('Ctrl Pts',(-86.7524132413505,-5.11979493494255,
4.07823117385119));
#40574=CARTESIAN_POINT('Ctrl Pts',(-86.6863547178727,-6.34705112076694,
2.23904869895045));
#40575=CARTESIAN_POINT('Ctrl Pts',(-86.5872669326561,-6.6454062926175,-1.06561278875027));
#40576=CARTESIAN_POINT('Ctrl Pts',(-86.4881791474394,-5.32904231695911,
-4.11064258710606));
#40577=CARTESIAN_POINT('Ctrl Pts',(-86.3890913622227,-2.71777688783439,
-6.15717933011816));
#40578=CARTESIAN_POINT('Ctrl Pts',(-86.2900035770061,0.553867298228359,
-6.70743373733954));
#40579=CARTESIAN_POINT('Ctrl Pts',(-86.1909157917893,3.69093181974381,-5.62795051717873));
#40580=CARTESIAN_POINT('Ctrl Pts',(-86.0918280065727,5.93114600216325,-3.18090720917224));
#40581=CARTESIAN_POINT('Ctrl Pts',(-85.992740221356,6.73016883205126,0.0390355434291301));
#40582=CARTESIAN_POINT('Ctrl Pts',(-85.8936524361394,5.89384698352793,3.24950303924472));
#40583=CARTESIAN_POINT('Ctrl Pts',(-85.7945646509227,3.62539642032013,5.67037828732898));
#40584=CARTESIAN_POINT('Ctrl Pts',(-85.695476865706,0.476021145237448,6.71342706269893));
#40585=CARTESIAN_POINT('Ctrl Pts',(-85.5963890804893,-2.78902109332259,
6.12519836322853));
#40586=CARTESIAN_POINT('Ctrl Pts',(-85.4973012952727,-5.37636715683683,
4.04862595386722));
#40587=CARTESIAN_POINT('Ctrl Pts',(-85.398213510056,-6.65732525222178,0.988289306225514));
#40588=CARTESIAN_POINT('Ctrl Pts',(-85.2991257248394,-6.32063907971779,
-2.31218876906367));
#40589=CARTESIAN_POINT('Ctrl Pts',(-85.2000379396226,-4.44811903426561,
-5.05083483042026));
#40590=CARTESIAN_POINT('Ctrl Pts',(-85.1009501544061,-1.49476336783044,
-6.56219306105075));
#40591=CARTESIAN_POINT('Ctrl Pts',(-85.0018623691893,1.82180054123787,-6.47902293265117));
#40592=CARTESIAN_POINT('Ctrl Pts',(-84.9027745839727,4.6956903879165,-4.82153368953529));
#40593=CARTESIAN_POINT('Ctrl Pts',(-84.8036867987559,6.42858796293502,-1.99247387764403));
#40594=CARTESIAN_POINT('Ctrl Pts',(-84.7045990135393,6.59942147947774,1.32073142041886));
#40595=CARTESIAN_POINT('Ctrl Pts',(-84.6055112283226,5.16668059390505,4.31301599669751));
#40596=CARTESIAN_POINT('Ctrl Pts',(-84.5064234431061,2.47850288400448,6.25729324890973));
#40597=CARTESIAN_POINT('Ctrl Pts',(-84.4073356578892,-0.811919097268936,
6.6811288512701));
#40598=CARTESIAN_POINT('Ctrl Pts',(-84.3082478726727,-3.90505519749678,
5.48153621285338));
#40599=CARTESIAN_POINT('Ctrl Pts',(-84.2091600874558,-6.04931319179036,
2.95000089080505));
#40600=CARTESIAN_POINT('Ctrl Pts',(-84.1100723022394,-6.72366601104527,
-0.298346644152522));
#40601=CARTESIAN_POINT('Ctrl Pts',(-84.0109845170225,-5.76425460756333,
-3.47419978806038));
#40602=CARTESIAN_POINT('Ctrl Pts',(-83.9118967318061,-3.4042035927283,-5.80586714000668));
#40603=CARTESIAN_POINT('Ctrl Pts',(-83.8128089465891,-0.216974959675104,
-6.72678357129485));
#40604=CARTESIAN_POINT('Ctrl Pts',(-83.7137211613727,3.02297579338882,-6.01317825286643));
#40605=CARTESIAN_POINT('Ctrl Pts',(-83.6146333761559,5.52838237228895,-3.83844808404757));
#40606=CARTESIAN_POINT('Ctrl Pts',(-83.5155455909393,6.6904632543721,-0.731024479795027));
#40607=CARTESIAN_POINT('Ctrl Pts',(-83.4164578057226,6.22684775585439,2.55402865558983));
#40608=CARTESIAN_POINT('Ctrl Pts',(-83.3173700205059,4.25018847032688,5.21848573006226));
#40609=CARTESIAN_POINT('Ctrl Pts',(-83.2182822352893,1.24078813976536,6.61491799952051));
#40610=CARTESIAN_POINT('Ctrl Pts',(-83.1191944500726,-2.07010772424683,
6.40401041209152));
#40611=CARTESIAN_POINT('Ctrl Pts',(-83.0201066648559,-4.8779940795284,4.63701079449345));
#40612=CARTESIAN_POINT('Ctrl Pts',(-82.9210188796392,-6.50059071447566,
1.74327729034592));
#40613=CARTESIAN_POINT('Ctrl Pts',(-82.8219310944226,-6.54362754997485,
-1.57405013750295));
#40614=CARTESIAN_POINT('Ctrl Pts',(-82.7228433092059,-4.99664718942376,
-4.50890365971447));
#40615=CARTESIAN_POINT('Ctrl Pts',(-82.6237555239892,-2.23554593138812,
-6.34815167878155));
#40616=CARTESIAN_POINT('Ctrl Pts',(-82.5246677387726,1.06876418844788,-6.64488062027108));
#40617=CARTESIAN_POINT('Ctrl Pts',(-82.4255799535559,4.11337837889662,-5.32698917402587));
#40618=CARTESIAN_POINT('Ctrl Pts',(-82.3264921683392,6.15849461406638,-2.71470798368413));
#40619=CARTESIAN_POINT('Ctrl Pts',(-82.2274043831226,6.70717599511822,0.557212274337937));
#40620=CARTESIAN_POINT('Ctrl Pts',(-82.1283165979058,5.62610001487058,3.69373712800955));
#40621=CARTESIAN_POINT('Ctrl Pts',(-82.0292288126892,3.17795420951081,5.93273144431935));
#40622=CARTESIAN_POINT('Ctrl Pts',(-81.9301410274726,-0.0423935286136112,
6.73014844835495));
#40623=CARTESIAN_POINT('Ctrl Pts',(-81.8310532422558,-3.25244018542155,
5.89222608089828));
#40624=CARTESIAN_POINT('Ctrl Pts',(-81.7319654570393,-5.67218577688769,
3.62256868266649));
#40625=CARTESIAN_POINT('Ctrl Pts',(-81.6328776718224,-6.71366329677356,
0.47267376246034));
#40626=CARTESIAN_POINT('Ctrl Pts',(-81.5337898866059,-6.1238071246307,-2.7920747927814));
#40627=CARTESIAN_POINT('Ctrl Pts',(-81.4347021013891,-4.04594471143955,
-5.37838514241379));
#40628=CARTESIAN_POINT('Ctrl Pts',(-81.3356143161726,-0.98496985544406,
-6.6578171897424));
#40629=CARTESIAN_POINT('Ctrl Pts',(-81.2365265309558,2.31533998650325,-6.31948542961072));
#40630=CARTESIAN_POINT('Ctrl Pts',(-81.1374387457392,5.05305203920794,-4.44560012115568));
#40631=CARTESIAN_POINT('Ctrl Pts',(-81.0383509605224,6.56293754256869,-1.49149125391514));
#40632=CARTESIAN_POINT('Ctrl Pts',(-80.9392631753059,6.47811377044076,1.82503077381967));
#40633=CARTESIAN_POINT('Ctrl Pts',(-80.8401753900891,4.81919180670493,4.69809383456215));
#40634=CARTESIAN_POINT('Ctrl Pts',(-80.7410876048726,1.98926831740783,6.42958061692366));
#40635=CARTESIAN_POINT('Ctrl Pts',(-80.6419998196558,-1.32402174617554,
6.59876213875127));
#40636=CARTESIAN_POINT('Ctrl Pts',(-80.5429120344392,-4.31559158221147,
5.16452946972989));
#40637=CARTESIAN_POINT('Ctrl Pts',(-80.4438242492225,-6.25852825958411,
2.47538267186104));
#40638=CARTESIAN_POINT('Ctrl Pts',(-80.3447364640058,-6.68072319566625,
-0.815250226034837));
#40639=CARTESIAN_POINT('Ctrl Pts',(-80.2456486787892,-5.47958845993628,
-3.90778782150415));
#40640=CARTESIAN_POINT('Ctrl Pts',(-80.1465608935725,-2.94698431950113,
-6.0507833186107));
#40641=CARTESIAN_POINT('Ctrl Pts',(-80.0474731083558,0.301699045906918,
-6.72351641879915));
#40642=CARTESIAN_POINT('Ctrl Pts',(-79.9483853231392,3.47707342981191,-5.76252164523996));
#40643=CARTESIAN_POINT('Ctrl Pts',(-79.8492975379224,5.8075637638367,-3.40130834784702));
#40644=CARTESIAN_POINT('Ctrl Pts',(-79.7502097527058,6.726890919466,-0.213620939444066));
#40645=CARTESIAN_POINT('Ctrl Pts',(-79.6511219674891,6.01167024115772,3.02597360526186));
#40646=CARTESIAN_POINT('Ctrl Pts',(-79.5520341822725,3.8356911398764,5.53029554613826));
#40647=CARTESIAN_POINT('Ctrl Pts',(-79.4529463970557,0.727688505078893,
6.69082691359887));
#40648=CARTESIAN_POINT('Ctrl Pts',(-79.3538586118392,-2.55713306197095,
6.22557353595137));
#40649=CARTESIAN_POINT('Ctrl Pts',(-79.2547708266223,-5.22060423735031,
4.2475859903153));
#40650=CARTESIAN_POINT('Ctrl Pts',(-79.1556830414058,-6.61553583773633,
1.23748976876148));
#40651=CARTESIAN_POINT('Ctrl Pts',(-79.056595256189,-6.40297745450795,-2.07330052458051));
#40652=CARTESIAN_POINT('Ctrl Pts',(-78.9575074709725,-4.6345780364962,-4.8803054998422));
#40653=CARTESIAN_POINT('Ctrl Pts',(-78.8584196857557,-1.74003586078818,
-6.50145910941029));
#40654=CARTESIAN_POINT('Ctrl Pts',(-78.7593319005392,1.57731261299649,-6.54284191074835));
#40655=CARTESIAN_POINT('Ctrl Pts',(-78.6602441153223,4.5113944416279,-4.99439841624713));
#40656=CARTESIAN_POINT('Ctrl Pts',(-78.5611563301058,6.34926553919752,-2.23238044717335));
#40657=CARTESIAN_POINT('Ctrl Pts',(-78.462068544889,6.64434690545786,1.0720772118161));
#40658=CARTESIAN_POINT('Ctrl Pts',(-78.3629807596725,5.32493756980748,4.11603391941998));
#40659=CARTESIAN_POINT('Ctrl Pts',(-78.2638929744557,2.71163700345574,6.15984740960786));
#40660=CARTESIAN_POINT('Ctrl Pts',(-78.1648051892392,-0.560556421942884,
6.70689733378866));
#40661=CARTESIAN_POINT('Ctrl Pts',(-78.0657174040223,-3.69654185820417,
5.62425760778321));
#40662=CARTESIAN_POINT('Ctrl Pts',(-77.9666296188058,-5.93431524379843,
3.17499573785298));
#40663=CARTESIAN_POINT('Ctrl Pts',(-77.867541833589,-6.73012647424846,-0.0457491943417124));
#40664=CARTESIAN_POINT('Ctrl Pts',(-77.7684540483724,-5.890603672631,-3.25537766167755));
#40665=CARTESIAN_POINT('Ctrl Pts',(-77.6693662631557,-3.6197400645466,-5.67399129478351));
#40666=CARTESIAN_POINT('Ctrl Pts',(-77.570278477939,-0.469326252251199,
-6.71389813872022));
#40667=CARTESIAN_POINT('Ctrl Pts',(-77.4711906927223,2.79512779322348,-6.12241422706049));
#40668=CARTESIAN_POINT('Ctrl Pts',(-77.3721029075058,5.38040179331176,-4.04326253051796));
#40669=CARTESIAN_POINT('Ctrl Pts',(-77.273015122289,6.65830747090767,-0.981650126581718));
#40670=CARTESIAN_POINT('Ctrl Pts',(-77.1739273370724,6.31833020903619,2.31849061195935));
#40671=CARTESIAN_POINT('Ctrl Pts',(-77.0748395518557,4.44308010255877,5.05526799986008));
#40672=CARTESIAN_POINT('Ctrl Pts',(-76.975751766639,1.48821876935064,6.56368038852559));
#40673=CARTESIAN_POINT('Ctrl Pts',(-76.8766639814223,-1.82826055276051,
6.47720299970463));
#40674=CARTESIAN_POINT('Ctrl Pts',(-76.7775761962058,-4.70049611320452,
4.81684872483164));
#40675=CARTESIAN_POINT('Ctrl Pts',(-76.678488410989,-6.4305716725049,1.98606226310769));
#40676=CARTESIAN_POINT('Ctrl Pts',(-76.5794006257724,-6.59810115753248,
-1.32731174300973));
#40677=CARTESIAN_POINT('Ctrl Pts',(-76.4803128405556,-5.1623770616321,-4.31816609473252));
#40678=CARTESIAN_POINT('Ctrl Pts',(-76.381225055339,-2.47226184432355,-6.25976171441573));
#40679=CARTESIAN_POINT('Ctrl Pts',(-76.2821372701223,0.818581152124673,
-6.68031587917437));
#40680=CARTESIAN_POINT('Ctrl Pts',(-76.1830494849057,3.91051947401727,-5.47763934478116));
#40681=CARTESIAN_POINT('Ctrl Pts',(-76.083961699689,6.05225194117708,-2.94396701555592));
#40682=CARTESIAN_POINT('Ctrl Pts',(-75.9848739144723,6.72336515505478,0.305051372654104));
#40683=CARTESIAN_POINT('Ctrl Pts',(-75.8857861292556,5.76078725032604,3.47994620714801));
#40684=CARTESIAN_POINT('Ctrl Pts',(-75.786698344039,3.39841225738424,5.80925894387774));
#40685=CARTESIAN_POINT('Ctrl Pts',(-75.6876105588223,0.210266866105867,
6.72699659530022));
#40686=CARTESIAN_POINT('Ctrl Pts',(-75.5885227736056,-3.02897066486332,
6.01016073491886));
#40687=CARTESIAN_POINT('Ctrl Pts',(-75.489434988389,-5.5322073451296,3.83293324213415));
#40688=CARTESIAN_POINT('Ctrl Pts',(-75.3903472031723,-6.69118890945404,
0.724352349455895));
#40689=CARTESIAN_POINT('Ctrl Pts',(-75.2912594179557,-6.22429776834097,
-2.56023683263652));
#40690=CARTESIAN_POINT('Ctrl Pts',(-75.1921716327389,-4.24498245433352,
-5.22272144677116));
#40691=CARTESIAN_POINT('Ctrl Pts',(-75.0930838475223,-1.23419109011172,
-6.61615203129823));
#40692=CARTESIAN_POINT('Ctrl Pts',(-74.9939960623057,2.07649280948173,-6.40194290511355));
#40693=CARTESIAN_POINT('Ctrl Pts',(-74.8949082770889,4.88261570688864,-4.63214412632067));
#40694=CARTESIAN_POINT('Ctrl Pts',(-74.7958204918723,6.50232588805105,-1.73679399864925));
#40695=CARTESIAN_POINT('Ctrl Pts',(-74.6967327066555,6.54205464494003,1.58057469636253));
#40696=CARTESIAN_POINT('Ctrl Pts',(-74.5976449214389,4.99214840143916,4.51388410198705));
#40697=CARTESIAN_POINT('Ctrl Pts',(-74.4985571362223,2.22921440797812,6.35037782115567));
#40698=CARTESIAN_POINT('Ctrl Pts',(-74.3994693510056,-1.07538996866078,
6.64381153882819));
#40699=CARTESIAN_POINT('Ctrl Pts',(-74.3003815657889,-4.1186884366776,5.3228846417841));
#40700=CARTESIAN_POINT('Ctrl Pts',(-74.2012937805723,-6.16119867378176,
2.70856534910143));
#40701=CARTESIAN_POINT('Ctrl Pts',(-74.1022059953555,-6.70661700509232,
-0.563900430190774));
#40702=CARTESIAN_POINT('Ctrl Pts',(-74.0031182101389,-5.6224138024785,-3.69934566942076));
#40703=CARTESIAN_POINT('Ctrl Pts',(-73.9040304249222,-3.17203647687603,
-5.93589756797832));
#40704=CARTESIAN_POINT('Ctrl Pts',(-73.8049426397056,0.0491048486963081,
-6.73010282700029));
#40705=CARTESIAN_POINT('Ctrl Pts',(-73.7058548544888,3.25831432863099,-5.88897979993147));
#40706=CARTESIAN_POINT('Ctrl Pts',(-73.6067670692723,5.6757954020979,-3.61691054654209));
#40707=CARTESIAN_POINT('Ctrl Pts',(-73.5076792840555,6.71413131155964,-0.465978625365368));
#40708=CARTESIAN_POINT('Ctrl Pts',(-73.4085914988389,6.12101980742883,2.79818009878328));
#40709=CARTESIAN_POINT('Ctrl Pts',(-73.3095037136222,4.04057934442206,5.38241710661602));
#40710=CARTESIAN_POINT('Ctrl Pts',(-73.2104159284055,0.978330153676572,
6.65879609678583));
#40711=CARTESIAN_POINT('Ctrl Pts',(-73.111328143189,-2.32164066102752,6.31717341769455));
#40712=CARTESIAN_POINT('Ctrl Pts',(-73.0122403579722,-5.0574827037483,4.44055897939096));
#40713=CARTESIAN_POINT('Ctrl Pts',(-72.9131525727555,-6.56442160272008,
1.48494591480795));
#40714=CARTESIAN_POINT('Ctrl Pts',(-72.8140647875389,-6.47629061870488,
-1.83148987718692));
#40715=CARTESIAN_POINT('Ctrl Pts',(-72.7149770023222,-4.81450444546676,
-4.70289722328094));
#40716=CARTESIAN_POINT('Ctrl Pts',(-72.6158892171056,-1.9828557150631,-6.4315611294152));
#40717=CARTESIAN_POINT('Ctrl Pts',(-72.5168014318888,1.33060140986772,-6.59743853599417));
#40718=CARTESIAN_POINT('Ctrl Pts',(-72.4177136466722,4.32073953373673,-5.16022337014276));
#40719=CARTESIAN_POINT('Ctrl Pts',(-72.3186258614555,6.26099361304058,-2.46914040216998));
#40720=CARTESIAN_POINT('Ctrl Pts',(-72.2195380762389,6.67990690192397,0.821911874711229));
#40721=CARTESIAN_POINT('Ctrl Pts',(-72.1204502910221,5.47568886785872,3.91325015435648));
#40722=CARTESIAN_POINT('Ctrl Pts',(-72.0213625058056,2.94094897972646,6.05371905912464));
#40723=CARTESIAN_POINT('Ctrl Pts',(-71.9222747205888,-0.308403623564008,
6.72321221984963));
#40724=CARTESIAN_POINT('Ctrl Pts',(-71.8231869353721,-3.48281811935279,
5.75905142325286));
#40725=CARTESIAN_POINT('Ctrl Pts',(-71.7240991501555,-5.81095267970918,
3.39551532205993));
#40726=CARTESIAN_POINT('Ctrl Pts',(-71.6250113649388,-6.72710059877092,
0.206912740494278));
#40727=CARTESIAN_POINT('Ctrl Pts',(-71.5259235797222,-6.00864973452521,
-3.03196697144825));
#40728=CARTESIAN_POINT('Ctrl Pts',(-71.4268357945055,-3.83017439150629,
-5.53411776878775));
#40729=CARTESIAN_POINT('Ctrl Pts',(-71.3277480092887,-0.721016013755397,
-6.69154924184759));
#40730=CARTESIAN_POINT('Ctrl Pts',(-71.2286602240722,2.56333996681492,-6.22302045334035));
#40731=CARTESIAN_POINT('Ctrl Pts',(-71.1295724388554,5.22483735779844,-4.24237786302878));
#40732=CARTESIAN_POINT('Ctrl Pts',(-71.0304846536388,6.61676658005308,-1.23089210463616));
#40733=CARTESIAN_POINT('Ctrl Pts',(-70.9313968684221,6.40090676416547,2.0796845781569));
#40734=CARTESIAN_POINT('Ctrl Pts',(-70.8323090832055,4.62970906457193,4.88492470009349));
#40735=CARTESIAN_POINT('Ctrl Pts',(-70.7332212979887,1.73355170473494,6.50319105018249));
#40736=CARTESIAN_POINT('Ctrl Pts',(-70.6341335127722,-1.58383638679021,
6.54126575274558));
#40737=CARTESIAN_POINT('Ctrl Pts',(-70.5350457275554,-4.51637264017302,
4.98989714555916));
#40738=CARTESIAN_POINT('Ctrl Pts',(-70.4359579423388,-6.35148852437948,
2.22604781458953));
#40739=CARTESIAN_POINT('Ctrl Pts',(-70.3368701571221,-6.64327452051517,
-1.07870245815835));
#40740=CARTESIAN_POINT('Ctrl Pts',(-70.2377823719054,-5.32083039046614,
-4.12134193000955));
#40741=CARTESIAN_POINT('Ctrl Pts',(-70.1386945866887,-2.7054930213848,-6.16254840625216));
#40742=CARTESIAN_POINT('Ctrl Pts',(-70.0396068014721,0.567244298250361,
-6.7063350090989));
#40743=CARTESIAN_POINT('Ctrl Pts',(-69.9405190162554,3.70214856096237,-5.62056859941476));
#40744=CARTESIAN_POINT('Ctrl Pts',(-69.8414312310388,5.93747841646568,-3.16907642731557));
#40745=CARTESIAN_POINT('Ctrl Pts',(-69.7423434458221,6.73007750661633,0.0524604908432818));
#40746=CARTESIAN_POINT('Ctrl Pts',(-69.6432556606054,5.88735446320337,3.26125018555189));
#40747=CARTESIAN_POINT('Ctrl Pts',(-69.5441678753887,3.6140801293562,5.67759809838248));
#40748=CARTESIAN_POINT('Ctrl Pts',(-69.445080090172,0.462630882635026,6.71436281523369));
#40749=CARTESIAN_POINT('Ctrl Pts',(-69.3459923049555,-2.80123170870239,
6.11962386608269));
#40750=CARTESIAN_POINT('Ctrl Pts',(-69.2469045197386,-5.3844310818254,4.0378951538179));
#40751=CARTESIAN_POINT('Ctrl Pts',(-69.1478167345221,-6.65928306725597,
0.975009937555351));
#40752=CARTESIAN_POINT('Ctrl Pts',(-69.0487289493054,-6.31601505587215,
-2.3247901329279));
#40753=CARTESIAN_POINT('Ctrl Pts',(-68.9496411640887,-4.43803675228133,
-5.0596961503157));
#40754=CARTESIAN_POINT('Ctrl Pts',(-68.850553378872,-1.48167269109562,-6.56516118498099));
#40755=CARTESIAN_POINT('Ctrl Pts',(-68.7514655936554,1.83471874628623,-6.4753766276418));
#40756=CARTESIAN_POINT('Ctrl Pts',(-68.6523778084387,4.70529716421494,-4.81215896924662));
#40757=CARTESIAN_POINT('Ctrl Pts',(-68.5532900232221,6.43254898736757,-1.9796486739622));
#40758=CARTESIAN_POINT('Ctrl Pts',(-68.4542022380054,6.59677427438435,1.33389074571141));
#40759=CARTESIAN_POINT('Ctrl Pts',(-68.3551144527886,5.15806839562815,4.32331189903167));
#40760=CARTESIAN_POINT('Ctrl Pts',(-68.256026667572,2.46601834651887,6.26222395424562));
#40761=CARTESIAN_POINT('Ctrl Pts',(-68.1569388823553,-0.825242393661263,
6.67949626585557));
#40762=CARTESIAN_POINT('Ctrl Pts',(-68.0578510971387,-3.91597986043431,
5.47373702592509));
#40763=CARTESIAN_POINT('Ctrl Pts',(-67.9587633119221,-6.0551846749451,2.93793022032393));
#40764=CARTESIAN_POINT('Ctrl Pts',(-67.8596755267053,-6.72305760742956,
-0.311755813135147));
#40765=CARTESIAN_POINT('Ctrl Pts',(-67.7605877414888,-5.7573141761971,-3.48568913462309));
#40766=CARTESIAN_POINT('Ctrl Pts',(-67.6614999562719,-3.39261751877765,
-5.81264503395175));
#40767=CARTESIAN_POINT('Ctrl Pts',(-67.5624121710554,-0.203558611737488,
-6.72720280201832));
#40768=CARTESIAN_POINT('Ctrl Pts',(-67.4633243858386,3.03496262220109,-6.00713749956949));
#40769=CARTESIAN_POINT('Ctrl Pts',(-67.3642366006221,5.53602661805977,-3.82741406304774));
#40770=CARTESIAN_POINT('Ctrl Pts',(-67.2651488154053,6.69190831335928,-0.717680564662976));
#40771=CARTESIAN_POINT('Ctrl Pts',(-67.1660610301887,6.22174077474846,2.56644462504013));
#40772=CARTESIAN_POINT('Ctrl Pts',(-67.066973244972,4.23977387275612,5.22694758728607));
#40773=CARTESIAN_POINT('Ctrl Pts',(-66.9678854597554,1.22758945576965,6.61738837079199));
#40774=CARTESIAN_POINT('Ctrl Pts',(-66.8687976745386,-2.08286902182032,
6.39985101098365));
#40775=CARTESIAN_POINT('Ctrl Pts',(-66.769709889322,-4.88724628381849,4.62730939927117));
#40776=CARTESIAN_POINT('Ctrl Pts',(-66.6706221041053,-6.50402659951364,
1.73023480709699));
#40777=CARTESIAN_POINT('Ctrl Pts',(-66.5715343188887,-6.54053194085659,
-1.58694591594768));
#40778=CARTESIAN_POINT('Ctrl Pts',(-66.4724465336719,-4.98752773549323,
-4.5191773691222));
#40779=CARTESIAN_POINT('Ctrl Pts',(-66.4063880101942,-3.1445555439941,-5.74073515448772));
#40780=CARTESIAN_POINT('Ctrl Pts',(-66.3733587484553,-2.13267601915869,
-6.0948088040903));
#40781=CARTESIAN_POINT('Ctrl Pts',(-86.6480812515447,-4.48284371989911,
4.97275105180613));
#40782=CARTESIAN_POINT('Ctrl Pts',(-86.6150519898058,-5.30843565119142,
4.22849509251194));
#40783=CARTESIAN_POINT('Ctrl Pts',(-86.5489934663281,-6.58091053988509,
2.32154726689182));
#40784=CARTESIAN_POINT('Ctrl Pts',(-86.4499056811113,-6.89025871712545,
-1.10487568155517));
#40785=CARTESIAN_POINT('Ctrl Pts',(-86.3508178958947,-5.52539282950227,
-4.26210071613823));
#40786=CARTESIAN_POINT('Ctrl Pts',(-86.251730110678,-2.81791437092512,-6.38404285368998));
#40787=CARTESIAN_POINT('Ctrl Pts',(-86.1526423254614,0.574274741333435,
-6.9545715857264));
#40788=CARTESIAN_POINT('Ctrl Pts',(-86.0535545402446,3.8269255521002,-5.83531441164414));
#40789=CARTESIAN_POINT('Ctrl Pts',(-85.9544667550281,6.14968124512553,-3.2981088982798));
#40790=CARTESIAN_POINT('Ctrl Pts',(-85.8553789698113,6.97814436331505,0.0404738222987098));
#40791=CARTESIAN_POINT('Ctrl Pts',(-85.7562911845946,6.11100793051157,3.36923216679088));
#40792=CARTESIAN_POINT('Ctrl Pts',(-85.657203399378,3.75897547692409,5.87930544849775));
#40793=CARTESIAN_POINT('Ctrl Pts',(-85.5581156141613,0.49356031837395,6.96078573734991));
#40794=CARTESIAN_POINT('Ctrl Pts',(-85.4590278289446,-2.8917835952124,6.35088353638262));
#40795=CARTESIAN_POINT('Ctrl Pts',(-85.359940043728,-5.5744613704079,4.19779905737357));
#40796=CARTESIAN_POINT('Ctrl Pts',(-85.2608522585113,-6.90261683515409,
1.02470318704625));
#40797=CARTESIAN_POINT('Ctrl Pts',(-85.1617644732947,-6.55352533752688,
-2.39738220962939));
#40798=CARTESIAN_POINT('Ctrl Pts',(-85.0626766880779,-4.61201160637967,
-5.23693468640519));
#40799=CARTESIAN_POINT('Ctrl Pts',(-84.9635889028613,-1.54983847062524,
-6.80397946361766));
#40800=CARTESIAN_POINT('Ctrl Pts',(-84.8645011176447,1.88892544825633,-6.71774490142901));
#40801=CARTESIAN_POINT('Ctrl Pts',(-84.7654133324279,4.86870481707144,-4.99918486114854));
#40802=CARTESIAN_POINT('Ctrl Pts',(-84.6663255472113,6.6654516368139,-2.06588730614305));
#40803=CARTESIAN_POINT('Ctrl Pts',(-84.5672377619945,6.84257957673285,1.36939425248265));
#40804=CARTESIAN_POINT('Ctrl Pts',(-84.4681499767779,5.3570488294005,4.47193064799671));
#40805=CARTESIAN_POINT('Ctrl Pts',(-84.3690621915613,2.56982422894208,6.48784550642254));
#40806=CARTESIAN_POINT('Ctrl Pts',(-84.2699744063446,-0.841834553257127,
6.92729748651229));
#40807=CARTESIAN_POINT('Ctrl Pts',(-84.1708866211279,-4.04893838399307,
5.68350541874474));
#40808=CARTESIAN_POINT('Ctrl Pts',(-84.0717988359113,-6.27220234805808,
3.05869475218969));
#40809=CARTESIAN_POINT('Ctrl Pts',(-83.9727110506946,-6.97140194349158,
-0.309339335336139));
#40810=CARTESIAN_POINT('Ctrl Pts',(-83.8736232654778,-5.9766406760737,-3.60220794946903));
#40811=CARTESIAN_POINT('Ctrl Pts',(-83.7745354802614,-3.52963271872836,
-6.01978643748904));
#40812=CARTESIAN_POINT('Ctrl Pts',(-83.6754476950444,-0.224969481393537,
-6.97463437138838));
#40813=CARTESIAN_POINT('Ctrl Pts',(-83.576359909828,3.1343584417398,-6.23473600409806));
#40814=CARTESIAN_POINT('Ctrl Pts',(-83.4772721246112,5.73207764205231,-3.97987710709635));
#40815=CARTESIAN_POINT('Ctrl Pts',(-83.3781843393946,6.93697581910938,-0.757959344026197));
#40816=CARTESIAN_POINT('Ctrl Pts',(-83.2790965541779,6.45627823804426,2.64813277519475));
#40817=CARTESIAN_POINT('Ctrl Pts',(-83.1800087689611,4.40678821844635,5.4107627447401));
#40818=CARTESIAN_POINT('Ctrl Pts',(-83.0809209837446,1.28650543242509,6.85864707172234));
#40819=CARTESIAN_POINT('Ctrl Pts',(-82.9818331985278,-2.14638160020794,
6.63996851712368));
#40820=CARTESIAN_POINT('Ctrl Pts',(-82.8827454133112,-5.05772555485365,
4.80786315257465));
#40821=CARTESIAN_POINT('Ctrl Pts',(-82.7836576280946,-6.7401073560603,1.80750897947607));
#40822=CARTESIAN_POINT('Ctrl Pts',(-82.6845698428778,-6.78472989949836,
-1.63204659031467));
#40823=CARTESIAN_POINT('Ctrl Pts',(-82.5854820576613,-5.18075048196443,
-4.67503586357689));
#40824=CARTESIAN_POINT('Ctrl Pts',(-82.4863942724445,-2.317915438578,-6.58205164836212));
#40825=CARTESIAN_POINT('Ctrl Pts',(-82.3873064872279,1.10814319572684,-6.88971367618925));
#40826=CARTESIAN_POINT('Ctrl Pts',(-82.2882187020112,4.26493730917755,-5.52326403776699));
#40827=CARTESIAN_POINT('Ctrl Pts',(-82.1891309167945,6.38540659975617,-2.81473239187942));
#40828=CARTESIAN_POINT('Ctrl Pts',(-82.0900431315779,6.9543043468987,0.577742964310748));
#40829=CARTESIAN_POINT('Ctrl Pts',(-81.9909553463612,5.83339572690187,3.82983422297465));
#40830=CARTESIAN_POINT('Ctrl Pts',(-81.8918675611445,3.29504709426618,6.15132510347753));
#40831=CARTESIAN_POINT('Ctrl Pts',(-81.7927797759278,-0.0439555336750358,
6.97812322857401));
#40832=CARTESIAN_POINT('Ctrl Pts',(-81.6936919907111,-3.37227753319247,
6.10932730513189));
#40833=CARTESIAN_POINT('Ctrl Pts',(-81.5946042054945,-5.88117953567009,
3.75604355024275));
#40834=CARTESIAN_POINT('Ctrl Pts',(-81.4955164202778,-6.9610306755554,0.490089600054565));
#40835=CARTESIAN_POINT('Ctrl Pts',(-81.3964286350611,-6.34944103708999,
-2.89494980934425));
#40836=CARTESIAN_POINT('Ctrl Pts',(-81.2973408498445,-4.19501902358835,
-5.57655370940124));
#40837=CARTESIAN_POINT('Ctrl Pts',(-81.1982530646278,-1.02126142988711,
-6.90312689829252));
#40838=CARTESIAN_POINT('Ctrl Pts',(-81.0991652794112,2.40064953482766,-6.55232918075981));
#40839=CARTESIAN_POINT('Ctrl Pts',(-81.0000774941945,5.2392335890613,-4.60939988299525));
#40840=CARTESIAN_POINT('Ctrl Pts',(-80.9009897089778,6.80475137582932,-1.54644579447639));
#40841=CARTESIAN_POINT('Ctrl Pts',(-80.8019019237612,6.71680224080455,1.89227469993862));
#40842=CARTESIAN_POINT('Ctrl Pts',(-80.7028141385443,4.99675669078907,4.8711968195875));
#40843=CARTESIAN_POINT('Ctrl Pts',(-80.603726353328,2.06256363586796,6.66648086550168));
#40844=CARTESIAN_POINT('Ctrl Pts',(-80.504638568111,-1.37280581149482,6.84189594235625));
#40845=CARTESIAN_POINT('Ctrl Pts',(-80.4055507828946,-4.4746011319006,5.35481844626862));
#40846=CARTESIAN_POINT('Ctrl Pts',(-80.3064629976777,-6.48912602151675,
2.56658905144142));
#40847=CARTESIAN_POINT('Ctrl Pts',(-80.2073752124612,-6.9268768843794,-0.845288418680318));
#40848=CARTESIAN_POINT('Ctrl Pts',(-80.1082874272444,-5.68148590015928,
-4.05177169253108));
#40849=CARTESIAN_POINT('Ctrl Pts',(-80.0091996420278,-3.05556703421317,
-6.27372664223861));
#40850=CARTESIAN_POINT('Ctrl Pts',(-79.910111856811,0.312815257558859,-6.97124683946445));
#40851=CARTESIAN_POINT('Ctrl Pts',(-79.8110240715945,3.60518747160154,-5.97484386211992));
#40852=CARTESIAN_POINT('Ctrl Pts',(-79.7119362863777,6.02154557404439,-3.52663079749089));
#40853=CARTESIAN_POINT('Ctrl Pts',(-79.6128485011612,6.97474567484213,-0.221491881060804));
#40854=CARTESIAN_POINT('Ctrl Pts',(-79.5137607159443,6.2331724291466,3.13746670908733));
#40855=CARTESIAN_POINT('Ctrl Pts',(-79.4146729307278,3.97701858230921,5.73406130749159));
#40856=CARTESIAN_POINT('Ctrl Pts',(-79.315585145511,0.754500454101965,6.93735287749331));
#40857=CARTESIAN_POINT('Ctrl Pts',(-79.2164973602945,-2.651351564564,6.45495706904306));
#40858=CARTESIAN_POINT('Ctrl Pts',(-79.1174095750777,-5.41295930920374,
4.40408984910723));
#40859=CARTESIAN_POINT('Ctrl Pts',(-79.0183217898611,-6.85928767441309,
1.28308553173565));
#40860=CARTESIAN_POINT('Ctrl Pts',(-78.9192340046443,-6.63889749984028,
-2.14969204043726));
#40861=CARTESIAN_POINT('Ctrl Pts',(-78.8201462194278,-4.80534075871954,
-5.060122140294));
#40862=CARTESIAN_POINT('Ctrl Pts',(-78.721058434211,-1.80414811826117,-6.74100774732379));
#40863=CARTESIAN_POINT('Ctrl Pts',(-78.6219706489944,1.63542927291058,-6.78391531310733));
#40864=CARTESIAN_POINT('Ctrl Pts',(-78.5228828637777,4.67761841926058,-5.17841885191792));
#40865=CARTESIAN_POINT('Ctrl Pts',(-78.4237950785611,6.58320654937237,-2.31463332093999));
#40866=CARTESIAN_POINT('Ctrl Pts',(-78.3247072933443,6.88916029645859,1.11157828865235));
#40867=CARTESIAN_POINT('Ctrl Pts',(-78.2256195081277,5.52113684144108,4.2676906940624));
#40868=CARTESIAN_POINT('Ctrl Pts',(-78.126531722911,2.81154826026171,6.38680923954397));
#40869=CARTESIAN_POINT('Ctrl Pts',(-78.0274439376944,-0.581210328256866,
6.95401541819058));
#40870=CARTESIAN_POINT('Ctrl Pts',(-77.9283561524777,-3.83274229447874,
5.83148543565175));
#40871=CARTESIAN_POINT('Ctrl Pts',(-77.8292683672611,-6.15296725862748,
3.29197961663846));
#40872=CARTESIAN_POINT('Ctrl Pts',(-77.7301805820443,-6.97810044482352,
-0.0474348401337781));
#40873=CARTESIAN_POINT('Ctrl Pts',(-77.6310927968278,-6.10764511863883,
-3.3753232418351));
#40874=CARTESIAN_POINT('Ctrl Pts',(-77.532005011611,-3.75311071065405,-5.88305157853291));
#40875=CARTESIAN_POINT('Ctrl Pts',(-77.4329172263944,-0.48661874960787,
-6.96127417033943));
#40876=CARTESIAN_POINT('Ctrl Pts',(-77.3338294411776,2.89811529870384,-6.34799681769954));
#40877=CARTESIAN_POINT('Ctrl Pts',(-77.2347416559611,5.57864466453888,-4.19223801673006));
#40878=CARTESIAN_POINT('Ctrl Pts',(-77.1356538707443,6.90363524404658,-1.0178193844011));
#40879=CARTESIAN_POINT('Ctrl Pts',(-77.0365660855277,6.55113139566086,2.40391624623061));
#40880=CARTESIAN_POINT('Ctrl Pts',(-76.937478300311,4.60678701339179,5.24153119759385));
#40881=CARTESIAN_POINT('Ctrl Pts',(-76.8383905150943,1.54305273402164,6.8055215922171));
#40882=CARTESIAN_POINT('Ctrl Pts',(-76.7393027298776,-1.89562348126539,
6.71585791238766));
#40883=CARTESIAN_POINT('Ctrl Pts',(-76.640214944661,-4.87368761106475,4.9943272772075));
#40884=CARTESIAN_POINT('Ctrl Pts',(-76.5411271594443,-6.66750843688816,
2.05923945332494));
#40885=CARTESIAN_POINT('Ctrl Pts',(-76.4420393742277,-6.84121060704279,
-1.37621702946524));
#40886=CARTESIAN_POINT('Ctrl Pts',(-76.3429515890109,-5.35258673190751,
-4.47727050327678));
#40887=CARTESIAN_POINT('Ctrl Pts',(-76.2438638037943,-2.56335323587229,
-6.4904049234426));
#40888=CARTESIAN_POINT('Ctrl Pts',(-76.1447760185776,0.848742073959769,
-6.92645456016245));
#40889=CARTESIAN_POINT('Ctrl Pts',(-76.0456882333609,4.05460399377978,-5.67946496914364));
#40890=CARTESIAN_POINT('Ctrl Pts',(-75.9466004481443,6.27524937674041,-3.05243855660093));
#40891=CARTESIAN_POINT('Ctrl Pts',(-75.8475126629276,6.97109000235212,0.316291102010706));
#40892=CARTESIAN_POINT('Ctrl Pts',(-75.7484248777109,5.97304556279128,3.60816609746892));
#40893=CARTESIAN_POINT('Ctrl Pts',(-75.6493370924943,3.52362799951616,6.02330321361383));
#40894=CARTESIAN_POINT('Ctrl Pts',(-75.5502493072776,0.218014225664164,
6.97485524434111));
#40895=CARTESIAN_POINT('Ctrl Pts',(-75.4511615220609,-3.14057419644558,
6.23160730459846));
#40896=CARTESIAN_POINT('Ctrl Pts',(-75.3520737368443,-5.73604354741575,
3.97415906881632));
#40897=CARTESIAN_POINT('Ctrl Pts',(-75.2529859516275,-6.93772821121811,
0.751041376605294));
#40898=CARTESIAN_POINT('Ctrl Pts',(-75.153898166411,-6.45363429530861,-2.65456969479452));
#40899=CARTESIAN_POINT('Ctrl Pts',(-75.0548103811942,-4.40139038489031,
-5.41515452797977));
#40900=CARTESIAN_POINT('Ctrl Pts',(-74.9557225959776,-1.27966531206499,
-6.85992657185209));
#40901=CARTESIAN_POINT('Ctrl Pts',(-74.8566348107609,2.15300194624281,-6.63782483209519));
#40902=CARTESIAN_POINT('Ctrl Pts',(-74.7575470255443,5.06251746776372,-4.80281717023373));
#40903=CARTESIAN_POINT('Ctrl Pts',(-74.6584592403275,6.74190646274048,-1.80078680852646));
#40904=CARTESIAN_POINT('Ctrl Pts',(-74.5593714551109,6.78309904020246,1.63881154893091));
#40905=CARTESIAN_POINT('Ctrl Pts',(-74.4602836698942,5.17608593449171,4.68019981206593));
#40906=CARTESIAN_POINT('Ctrl Pts',(-74.3611958846776,2.31135062787306,6.58435981376593));
#40907=CARTESIAN_POINT('Ctrl Pts',(-74.2621080994609,-1.11501310523416,
6.88860520404971));
#40908=CARTESIAN_POINT('Ctrl Pts',(-74.1630203142442,-4.27044301797891,
5.5190082725341));
#40909=CARTESIAN_POINT('Ctrl Pts',(-74.0639325290276,-6.3882102915404,2.80836342967968));
#40910=CARTESIAN_POINT('Ctrl Pts',(-73.9648447438108,-6.95372476068093,
-0.584677547711268));
#40911=CARTESIAN_POINT('Ctrl Pts',(-73.8657569585942,-5.82957369466647,
-3.83564941314472));
#40912=CARTESIAN_POINT('Ctrl Pts',(-73.7666691733775,-3.28891132060887,
-6.15460788412029));
#40913=CARTESIAN_POINT('Ctrl Pts',(-73.6675813881609,0.0509141347999404,
-6.97807592628386));
#40914=CARTESIAN_POINT('Ctrl Pts',(-73.5684936029441,3.37836811135612,-6.10596141375596));
#40915=CARTESIAN_POINT('Ctrl Pts',(-73.4694058177276,5.88492215884091,-3.75017693802415));
#40916=CARTESIAN_POINT('Ctrl Pts',(-73.3703180325108,6.96151593451736,-0.483147778185493));
#40917=CARTESIAN_POINT('Ctrl Pts',(-73.2712302472942,6.34655102016675,2.90128006757796));
#40918=CARTESIAN_POINT('Ctrl Pts',(-73.1721424620775,4.18945596766144,5.58073423279865));
#40919=CARTESIAN_POINT('Ctrl Pts',(-73.0730546768608,1.01437708588044,6.90414187352386));
#40920=CARTESIAN_POINT('Ctrl Pts',(-72.9739668916443,-2.4071823600084,6.5499319819193));
#40921=CARTESIAN_POINT('Ctrl Pts',(-72.8748791064274,-5.24382750305657,
4.60417299851909));
#40922=CARTESIAN_POINT('Ctrl Pts',(-72.7757913212108,-6.80629011671958,
1.53965928995673));
#40923=CARTESIAN_POINT('Ctrl Pts',(-72.6767035359942,-6.7149119143764,-1.89897179133098));
#40924=CARTESIAN_POINT('Ctrl Pts',(-72.5776157507775,-4.99189662201232,
-4.87617719091982));
#40925=CARTESIAN_POINT('Ctrl Pts',(-72.4785279655608,-2.05591475884529,
-6.66853435070007));
#40926=CARTESIAN_POINT('Ctrl Pts',(-72.3794401803442,1.37962790530135,-6.84052357097165));
#40927=CARTESIAN_POINT('Ctrl Pts',(-72.2803523951275,4.47993876158198,-5.35035368686783));
#40928=CARTESIAN_POINT('Ctrl Pts',(-72.1812646099109,6.49168221182268,-2.56011678304133));
#40929=CARTESIAN_POINT('Ctrl Pts',(-72.0821768246941,6.92603051399574,0.852195518237787));
#40930=CARTESIAN_POINT('Ctrl Pts',(-71.9830890394775,5.67744262618587,4.05743528703446));
#40931=CARTESIAN_POINT('Ctrl Pts',(-71.8840012542608,3.0493093201379,6.27677055118515));
#40932=CARTESIAN_POINT('Ctrl Pts',(-71.7849134690441,-0.319766867831018,
6.97093143219341));
#40933=CARTESIAN_POINT('Ctrl Pts',(-71.6858256838275,-3.6111438263289,5.97124577853496));
#40934=CARTESIAN_POINT('Ctrl Pts',(-71.5867378986107,-6.02505935576122,
3.52062432555065));
#40935=CARTESIAN_POINT('Ctrl Pts',(-71.4876501133942,-6.97496307985772,
0.214536516068103));
#40936=CARTESIAN_POINT('Ctrl Pts',(-71.3885623281774,-6.23004063084288,
-3.14368090304213));
#40937=CARTESIAN_POINT('Ctrl Pts',(-71.2894745429608,-3.9712985673284,-5.73802436133205));
#40938=CARTESIAN_POINT('Ctrl Pts',(-71.190386757744,-0.747582112396103,
-6.93810182019046));
#40939=CARTESIAN_POINT('Ctrl Pts',(-71.0912989725275,2.65778716508629,-6.45230991716978));
#40940=CARTESIAN_POINT('Ctrl Pts',(-70.9922111873108,5.41734840052245,-4.39868982646668));
#40941=CARTESIAN_POINT('Ctrl Pts',(-70.8931234020941,6.8605637638805,-1.27624477426342));
#40942=CARTESIAN_POINT('Ctrl Pts',(-70.7940356168774,6.63675051415506,2.15631131680177));
#40943=CARTESIAN_POINT('Ctrl Pts',(-70.6949478316608,4.80029238774456,5.0649115366674));
#40944=CARTESIAN_POINT('Ctrl Pts',(-70.5958600464441,1.79742505110744,6.74280350208697));
#40945=CARTESIAN_POINT('Ctrl Pts',(-70.4967722612274,-1.64219341753491,
6.78228108098667));
#40946=CARTESIAN_POINT('Ctrl Pts',(-70.3976844760107,-4.6827800413512,5.17375173026572));
#40947=CARTESIAN_POINT('Ctrl Pts',(-70.2985966907941,-6.58551144125611,
2.30806736019331));
#40948=CARTESIAN_POINT('Ctrl Pts',(-70.1995089055774,-6.8880483991006,-1.11844764461836));
#40949=CARTESIAN_POINT('Ctrl Pts',(-70.1004211203607,-5.51687833157526,
-4.27319428024283));
#40950=CARTESIAN_POINT('Ctrl Pts',(-70.001333335144,-2.80517790092504,-6.38960975539716));
#40951=CARTESIAN_POINT('Ctrl Pts',(-69.9022455499274,0.588144621812076,
-6.95343237444202));
#40952=CARTESIAN_POINT('Ctrl Pts',(-69.8031577647108,3.83855557824996,-5.82766050442122));
#40953=CARTESIAN_POINT('Ctrl Pts',(-69.704069979494,6.15624697954815,-3.28584220694011));
#40954=CARTESIAN_POINT('Ctrl Pts',(-69.6049821942774,6.97804967296109,0.0543934168086905));
#40955=CARTESIAN_POINT('Ctrl Pts',(-69.5058944090607,6.10427619090187,3.38141214099867));
#40956=CARTESIAN_POINT('Ctrl Pts',(-69.406806623844,3.74724223308222,5.88679127612919));
#40957=CARTESIAN_POINT('Ctrl Pts',(-69.3077188386274,0.479676686650263,
6.96175596802892));
#40958=CARTESIAN_POINT('Ctrl Pts',(-69.2086310534108,-2.90444411518026,
6.34510364485133));
#40959=CARTESIAN_POINT('Ctrl Pts',(-69.109543268194,-5.58282241366096,4.18667287707308));
#40960=CARTESIAN_POINT('Ctrl Pts',(-69.0104554829774,-6.90464678659901,
1.01093453518231));
#40961=CARTESIAN_POINT('Ctrl Pts',(-68.9113676977607,-6.54873093983205,
-2.41044787535243));
#40962=CARTESIAN_POINT('Ctrl Pts',(-68.812279912544,-4.60155783902944,-5.24612250487201));
#40963=CARTESIAN_POINT('Ctrl Pts',(-68.7131921273274,-1.53626546311999,
-6.8070569491593));
#40964=CARTESIAN_POINT('Ctrl Pts',(-68.6141043421107,1.90231962929278,-6.71396424697843));
#40965=CARTESIAN_POINT('Ctrl Pts',(-68.515016556894,4.87866555855498,-4.98946472586331));
#40966=CARTESIAN_POINT('Ctrl Pts',(-68.4159287716774,6.66955860663988,-2.05258955314249));
#40967=CARTESIAN_POINT('Ctrl Pts',(-68.3168409864607,6.83983483439994,1.38303843792684));
#40968=CARTESIAN_POINT('Ctrl Pts',(-68.2177532012439,5.34811931152934,4.4826059066167));
#40969=CARTESIAN_POINT('Ctrl Pts',(-68.1186654160274,2.55687969410828,6.49295788539925));
#40970=CARTESIAN_POINT('Ctrl Pts',(-68.0195776308106,-0.85564875137622,
6.92560474789127));
#40971=CARTESIAN_POINT('Ctrl Pts',(-67.920489845594,-4.06026557013075,5.67541886792257));
#40972=CARTESIAN_POINT('Ctrl Pts',(-67.8214020603773,-6.27829016815635,
3.04617933344148));
#40973=CARTESIAN_POINT('Ctrl Pts',(-67.7223142751607,-6.9707711230222,-0.323242570052509));
#40974=CARTESIAN_POINT('Ctrl Pts',(-67.623226489944,-5.96944452197626,-3.61412062520652));
#40975=CARTESIAN_POINT('Ctrl Pts',(-67.5241387047273,-3.51761975164696,
-6.02681406541461));
#40976=CARTESIAN_POINT('Ctrl Pts',(-67.4250509195106,-0.211058803210948,
-6.97506904882113));
#40977=CARTESIAN_POINT('Ctrl Pts',(-67.325963134294,3.1467869296422,-6.22847267703732));
#40978=CARTESIAN_POINT('Ctrl Pts',(-67.2268753490773,5.7400035428534,-3.96843653355858));
#40979=CARTESIAN_POINT('Ctrl Pts',(-67.1277875638606,6.93847412182326,-0.744123767462383));
#40980=CARTESIAN_POINT('Ctrl Pts',(-67.0286997786439,6.45098308835231,2.66100621557892));
#40981=CARTESIAN_POINT('Ctrl Pts',(-66.9296119934273,4.39598989122037,5.41953638218708));
#40982=CARTESIAN_POINT('Ctrl Pts',(-66.8305242082107,1.27282043809193,6.86120846472652));
#40983=CARTESIAN_POINT('Ctrl Pts',(-66.7314364229939,-2.15961309245625,
6.63565586136125));
#40984=CARTESIAN_POINT('Ctrl Pts',(-66.6323486377773,-5.06731865999354,
4.79780430589844));
#40985=CARTESIAN_POINT('Ctrl Pts',(-66.5332608525606,-6.74366983753873,
1.79398594116332));
#40986=CARTESIAN_POINT('Ctrl Pts',(-66.4341730673439,-6.78152023153034,
-1.64541751843109));
#40987=CARTESIAN_POINT('Ctrl Pts',(-66.3350852821273,-5.17129501841962,
-4.68568811156397));
#40988=CARTESIAN_POINT('Ctrl Pts',(-66.2690267586495,-3.26041784270748,
-5.95225464015044));
#40989=CARTESIAN_POINT('Ctrl Pts',(-66.2359974969106,-2.21125524682175,
-6.31937426282706));
#40990=CARTESIAN_POINT('Ctrl Pts',(-86.51072,-4.64214617842353,5.14946287083884));
#40991=CARTESIAN_POINT('Ctrl Pts',(-86.4776907382611,-5.49707636744029,
4.37875901117269));
#40992=CARTESIAN_POINT('Ctrl Pts',(-86.4116322147833,-6.81476995900323,
2.40404583483319));
#40993=CARTESIAN_POINT('Ctrl Pts',(-86.3125444295667,-7.1351111416334,-1.14413857436007));
#40994=CARTESIAN_POINT('Ctrl Pts',(-86.2134566443499,-5.72174334204543,
-4.41355884517039));
#40995=CARTESIAN_POINT('Ctrl Pts',(-86.1143688591333,-2.91805185401586,
-6.61090637726181));
#40996=CARTESIAN_POINT('Ctrl Pts',(-86.0152810739167,0.594682184438515,
-7.20170943411326));
#40997=CARTESIAN_POINT('Ctrl Pts',(-85.9161932886999,3.96291928445659,-6.04267830610954));
#40998=CARTESIAN_POINT('Ctrl Pts',(-85.8171055034833,6.36821648808781,-3.41531058738736));
#40999=CARTESIAN_POINT('Ctrl Pts',(-85.7180177182667,7.22611989457885,0.0419121011682899));
#41000=CARTESIAN_POINT('Ctrl Pts',(-85.6189299330499,6.32816887749518,3.48896129433705));
#41001=CARTESIAN_POINT('Ctrl Pts',(-85.5198421478333,3.89255453352808,6.08823260966652));
#41002=CARTESIAN_POINT('Ctrl Pts',(-85.4207543626166,0.511099491510444,
7.20814441200088));
#41003=CARTESIAN_POINT('Ctrl Pts',(-85.3216665774,-2.99454609710222,6.57656870953671));
#41004=CARTESIAN_POINT('Ctrl Pts',(-85.2225787921833,-5.77255558397897,
4.34697216087991));
#41005=CARTESIAN_POINT('Ctrl Pts',(-85.1234910069666,-7.14790841808639,
1.06111706786699));
#41006=CARTESIAN_POINT('Ctrl Pts',(-85.02440322175,-6.78641159533597,-2.4825756501951));
#41007=CARTESIAN_POINT('Ctrl Pts',(-84.9253154365331,-4.77590417849372,
-5.42303454239013));
#41008=CARTESIAN_POINT('Ctrl Pts',(-84.8262276513167,-1.60491357342004,
-7.04576586618457));
#41009=CARTESIAN_POINT('Ctrl Pts',(-84.7271398660999,1.95605035527479,-6.95646687020684));
#41010=CARTESIAN_POINT('Ctrl Pts',(-84.6280520808833,5.04171924622639,-5.1768360327618));
#41011=CARTESIAN_POINT('Ctrl Pts',(-84.5289642956666,6.90231531069278,-2.13930073464208));
#41012=CARTESIAN_POINT('Ctrl Pts',(-84.4298765104498,7.08573767398796,1.41805708454642));
#41013=CARTESIAN_POINT('Ctrl Pts',(-84.3307887252333,5.54741706489595,4.63084529929592));
#41014=CARTESIAN_POINT('Ctrl Pts',(-84.2317009400165,2.66114557387967,6.71839776393533));
#41015=CARTESIAN_POINT('Ctrl Pts',(-84.1326131547999,-0.871750009245318,
7.17346612175447));
#41016=CARTESIAN_POINT('Ctrl Pts',(-84.0335253695832,-4.19282157048937,
5.88547462463609));
#41017=CARTESIAN_POINT('Ctrl Pts',(-83.9344375843665,-6.4950915043258,3.16738861357433));
#41018=CARTESIAN_POINT('Ctrl Pts',(-83.8353497991499,-7.21913787593788,
-0.320332026519753));
#41019=CARTESIAN_POINT('Ctrl Pts',(-83.7362620139332,-6.18902674458406,
-3.73021611087769));
#41020=CARTESIAN_POINT('Ctrl Pts',(-83.6371742287166,-3.65506184472842,
-6.2337057349714));
#41021=CARTESIAN_POINT('Ctrl Pts',(-83.5380864434999,-0.232964003111965,
-7.2224851714819));
#41022=CARTESIAN_POINT('Ctrl Pts',(-83.4389986582832,3.24574109009077,-6.4562937553297));
#41023=CARTESIAN_POINT('Ctrl Pts',(-83.3399108730665,5.93577291181568,-4.12130613014512));
#41024=CARTESIAN_POINT('Ctrl Pts',(-83.2408230878499,7.18348838384663,-0.784894208257366));
#41025=CARTESIAN_POINT('Ctrl Pts',(-83.1417353026331,6.68570872023415,2.74223689479967));
#41026=CARTESIAN_POINT('Ctrl Pts',(-83.0426475174165,4.56338796656581,5.60303975941794));
#41027=CARTESIAN_POINT('Ctrl Pts',(-82.9435597321999,1.33222272508483,7.10237614392416));
#41028=CARTESIAN_POINT('Ctrl Pts',(-82.8444719469831,-2.22265547616906,
6.87592662215584));
#41029=CARTESIAN_POINT('Ctrl Pts',(-82.7453841617666,-5.2374570301789,4.97871551065585));
#41030=CARTESIAN_POINT('Ctrl Pts',(-82.6462963765498,-6.97962399764495,
1.87174066860623));
#41031=CARTESIAN_POINT('Ctrl Pts',(-82.5472085913332,-7.02583224902186,
-1.6900430431264));
#41032=CARTESIAN_POINT('Ctrl Pts',(-82.4481208061165,-5.3648537745051,-4.84116806743931));
#41033=CARTESIAN_POINT('Ctrl Pts',(-82.3490330208998,-2.40028494576787,
-6.8159516179427));
#41034=CARTESIAN_POINT('Ctrl Pts',(-82.2499452356832,1.14752220300579,-7.13454673210741));
#41035=CARTESIAN_POINT('Ctrl Pts',(-82.1508574504664,4.41649623945849,-5.71953890150811));
#41036=CARTESIAN_POINT('Ctrl Pts',(-82.0517696652499,6.61231858544595,-2.91475680007471));
#41037=CARTESIAN_POINT('Ctrl Pts',(-81.9526818800332,7.20143269867919,0.598273654283556));
#41038=CARTESIAN_POINT('Ctrl Pts',(-81.8535940948164,6.04069143893316,3.96593131793975));
#41039=CARTESIAN_POINT('Ctrl Pts',(-81.7545063095999,3.41213997902156,6.36991876263571));
#41040=CARTESIAN_POINT('Ctrl Pts',(-81.655418524383,-0.0455175387364694,
7.22609800879306));
#41041=CARTESIAN_POINT('Ctrl Pts',(-81.5563307391665,-3.49211488096338,
6.3264285293655));
#41042=CARTESIAN_POINT('Ctrl Pts',(-81.4572429539498,-6.09017329445249,
3.88951841781901));
#41043=CARTESIAN_POINT('Ctrl Pts',(-81.3581551687331,-7.20839805433722,
0.507505437648791));
#41044=CARTESIAN_POINT('Ctrl Pts',(-81.2590673835164,-6.57507494954929,
-2.9978248259071));
#41045=CARTESIAN_POINT('Ctrl Pts',(-81.1599795982998,-4.34409333573713,
-5.7747222763887));
#41046=CARTESIAN_POINT('Ctrl Pts',(-81.0608918130831,-1.05755300433017,
-7.14843660684264));
#41047=CARTESIAN_POINT('Ctrl Pts',(-80.9618040278664,2.48595908315207,-6.78517293190891));
#41048=CARTESIAN_POINT('Ctrl Pts',(-80.8627162426498,5.42541513891466,-4.77319964483483));
#41049=CARTESIAN_POINT('Ctrl Pts',(-80.7636284574331,7.04656520908996,-1.60140033503765));
#41050=CARTESIAN_POINT('Ctrl Pts',(-80.6645406722165,6.95549071116834,1.95951862605758));
#41051=CARTESIAN_POINT('Ctrl Pts',(-80.5654528869997,5.17432157487322,5.04429980461283));
#41052=CARTESIAN_POINT('Ctrl Pts',(-80.4663651017832,2.13585895432808,6.9033811140797));
#41053=CARTESIAN_POINT('Ctrl Pts',(-80.3672773165663,-1.42158987681409,
7.08502974596122));
#41054=CARTESIAN_POINT('Ctrl Pts',(-80.2681895313499,-4.63361068158974,
5.54510742280736));
#41055=CARTESIAN_POINT('Ctrl Pts',(-80.1691017461329,-6.71972378344938,
2.65779543102179));
#41056=CARTESIAN_POINT('Ctrl Pts',(-80.0700139609165,-7.17303057309256,
-0.875326611325795));
#41057=CARTESIAN_POINT('Ctrl Pts',(-79.9709261756997,-5.88338334038227,
-4.19575556355802));
#41058=CARTESIAN_POINT('Ctrl Pts',(-79.8718383904831,-3.16414974892521,
-6.49666996586653));
#41059=CARTESIAN_POINT('Ctrl Pts',(-79.7727506052664,0.323931469210802,
-7.21897726012976));
#41060=CARTESIAN_POINT('Ctrl Pts',(-79.6736628200498,3.73330151339117,-6.18716607899989));
#41061=CARTESIAN_POINT('Ctrl Pts',(-79.574575034833,6.23552738425208,-3.65195324713476));
#41062=CARTESIAN_POINT('Ctrl Pts',(-79.4754872496165,7.22260043021827,-0.22936282267754));
#41063=CARTESIAN_POINT('Ctrl Pts',(-79.3763994643997,6.45467461713548,3.24895981291281));
#41064=CARTESIAN_POINT('Ctrl Pts',(-79.2773116791831,4.11834602474202,5.93782706884491));
#41065=CARTESIAN_POINT('Ctrl Pts',(-79.1782238939663,0.781312403125045,
7.18387884138775));
#41066=CARTESIAN_POINT('Ctrl Pts',(-79.0791361087498,-2.74557006715706,
6.68434060213473));
#41067=CARTESIAN_POINT('Ctrl Pts',(-78.980048323533,-5.60531438105715,4.56059370789917));
#41068=CARTESIAN_POINT('Ctrl Pts',(-78.8809605383164,-7.10303951108988,
1.32868129470981));
#41069=CARTESIAN_POINT('Ctrl Pts',(-78.7818727530996,-6.87481754517261,
-2.226083556294));
#41070=CARTESIAN_POINT('Ctrl Pts',(-78.6827849678831,-4.97610348094288,
-5.2399387807458));
#41071=CARTESIAN_POINT('Ctrl Pts',(-78.5836971826663,-1.86826037573416,
-6.9805563852373));
#41072=CARTESIAN_POINT('Ctrl Pts',(-78.4846093974497,1.69354593282467,-7.02498871546629));
#41073=CARTESIAN_POINT('Ctrl Pts',(-78.385521612233,4.84384239689327,-5.36243928758871));
#41074=CARTESIAN_POINT('Ctrl Pts',(-78.2864338270164,6.81714755954721,-2.39688619470662));
#41075=CARTESIAN_POINT('Ctrl Pts',(-78.1873460417996,7.13397368745932,1.15107936548859));
#41076=CARTESIAN_POINT('Ctrl Pts',(-78.0882582565831,5.71733611307469,4.41934746870483));
#41077=CARTESIAN_POINT('Ctrl Pts',(-77.9891704713662,2.91145951706769,6.61377106948008));
#41078=CARTESIAN_POINT('Ctrl Pts',(-77.8900826861498,-0.601864234570844,
7.20113350259251));
#41079=CARTESIAN_POINT('Ctrl Pts',(-77.7909949009329,-3.96894273075332,
6.03871326352029));
#41080=CARTESIAN_POINT('Ctrl Pts',(-77.6919071157164,-6.37161927345652,
3.40896349542395));
#41081=CARTESIAN_POINT('Ctrl Pts',(-77.5928193304996,-7.22607441539859,
-0.049120485925841));
#41082=CARTESIAN_POINT('Ctrl Pts',(-77.493731545283,-6.32468656464665,-3.49526882199265));
#41083=CARTESIAN_POINT('Ctrl Pts',(-77.3946437600663,-3.8864813567615,-6.0921118622823));
#41084=CARTESIAN_POINT('Ctrl Pts',(-77.2955559748497,-0.503911246964539,
-7.20865020195864));
#41085=CARTESIAN_POINT('Ctrl Pts',(-77.1964681896329,3.0011028041842,-6.57357940833861));
#41086=CARTESIAN_POINT('Ctrl Pts',(-77.0973804044164,5.77688753576599,-4.34121350294215));
#41087=CARTESIAN_POINT('Ctrl Pts',(-76.9982926191996,7.14896301718548,-1.05398864222048));
#41088=CARTESIAN_POINT('Ctrl Pts',(-76.899204833983,6.78393258228553,2.48934188050186));
#41089=CARTESIAN_POINT('Ctrl Pts',(-76.8001170487663,4.77049392422479,5.42779439532762));
#41090=CARTESIAN_POINT('Ctrl Pts',(-76.7010292635497,1.59788669869266,7.04736279590861));
#41091=CARTESIAN_POINT('Ctrl Pts',(-76.6019414783329,-1.96298640977028,
6.95451282507069));
#41092=CARTESIAN_POINT('Ctrl Pts',(-76.5028536931164,-5.04687910892497,
5.17180582958336));
#41093=CARTESIAN_POINT('Ctrl Pts',(-76.4037659078996,-6.90444520127142,
2.1324166435422));
#41094=CARTESIAN_POINT('Ctrl Pts',(-76.304678122683,-7.08432005655309,-1.42512231592074));
#41095=CARTESIAN_POINT('Ctrl Pts',(-76.2055903374662,-5.54279640218294,
-4.63637491182103));
#41096=CARTESIAN_POINT('Ctrl Pts',(-76.1065025522496,-2.65444462742102,
-6.72104813246947));
#41097=CARTESIAN_POINT('Ctrl Pts',(-76.0074147670329,0.878902995794858,
-7.17259324115054));
#41098=CARTESIAN_POINT('Ctrl Pts',(-75.9083269818163,4.19868851354229,-5.88129059350613));
#41099=CARTESIAN_POINT('Ctrl Pts',(-75.8092391965996,6.49824681230373,-3.16091009764594));
#41100=CARTESIAN_POINT('Ctrl Pts',(-75.7101514113829,7.21881484964945,0.327530831367305));
#41101=CARTESIAN_POINT('Ctrl Pts',(-75.6110636261662,6.18530387525653,3.73638598778983));
#41102=CARTESIAN_POINT('Ctrl Pts',(-75.5119758409496,3.64884374164807,6.2373474833499));
#41103=CARTESIAN_POINT('Ctrl Pts',(-75.4128880557329,0.22576158522246,7.22271389338201));
#41104=CARTESIAN_POINT('Ctrl Pts',(-75.3138002705162,-3.25217772802784,
6.45305387427807));
#41105=CARTESIAN_POINT('Ctrl Pts',(-75.2147124852996,-5.93987974970189,
4.11538489549849));
#41106=CARTESIAN_POINT('Ctrl Pts',(-75.1156247000829,-7.18426751298218,
0.777730403754694));
#41107=CARTESIAN_POINT('Ctrl Pts',(-75.0165369148663,-6.68297082227624,
-2.74890255695254));
#41108=CARTESIAN_POINT('Ctrl Pts',(-74.9174491296495,-4.5577983154471,-5.60758760918838));
#41109=CARTESIAN_POINT('Ctrl Pts',(-74.8183613444329,-1.32513953401825,
-7.10370111240595));
#41110=CARTESIAN_POINT('Ctrl Pts',(-74.7192735592163,2.22951108300389,-6.87370675907684));
#41111=CARTESIAN_POINT('Ctrl Pts',(-74.6201857739995,5.24241922863879,-4.97349021414678));
#41112=CARTESIAN_POINT('Ctrl Pts',(-74.5210979887829,6.98148703742991,-1.86477961840367));
#41113=CARTESIAN_POINT('Ctrl Pts',(-74.4220102035662,7.02414343546488,1.69704840149928));
#41114=CARTESIAN_POINT('Ctrl Pts',(-74.3229224183495,5.36002346754426,4.8465155221448));
#41115=CARTESIAN_POINT('Ctrl Pts',(-74.223834633133,2.393486847768,6.8183418063762));
#41116=CARTESIAN_POINT('Ctrl Pts',(-74.1247468479161,-1.15463624180754,
7.13339886927123));
#41117=CARTESIAN_POINT('Ctrl Pts',(-74.0256590626995,-4.42219759928022,
5.71513190328411));
#41118=CARTESIAN_POINT('Ctrl Pts',(-73.9265712774829,-6.61522190929904,
2.90816151025792));
#41119=CARTESIAN_POINT('Ctrl Pts',(-73.8274834922662,-7.20083251626954,
-0.605454665231755));
#41120=CARTESIAN_POINT('Ctrl Pts',(-73.7283957070495,-6.03673358685444,
-3.97195315686868));
#41121=CARTESIAN_POINT('Ctrl Pts',(-73.6293079218328,-3.40578616434171,
-6.37331820026227));
#41122=CARTESIAN_POINT('Ctrl Pts',(-73.5302201366162,0.0527234209035772,
-7.22604902556742));
#41123=CARTESIAN_POINT('Ctrl Pts',(-73.4311323513995,3.49842189408126,-6.32294302758046));
#41124=CARTESIAN_POINT('Ctrl Pts',(-73.3320445661829,6.09404891558392,-3.88344332950621));
#41125=CARTESIAN_POINT('Ctrl Pts',(-73.2329567809661,7.20890055747509,-0.500316931005614));
#41126=CARTESIAN_POINT('Ctrl Pts',(-73.1338689957495,6.57208223290466,3.00438003637265));
#41127=CARTESIAN_POINT('Ctrl Pts',(-73.0347812105329,4.33833259090082,5.77905135898128));
#41128=CARTESIAN_POINT('Ctrl Pts',(-72.9356934253161,1.0504240180843,7.1494876502619));
#41129=CARTESIAN_POINT('Ctrl Pts',(-72.8366056400996,-2.49272405898927,
6.78269054614404));
#41130=CARTESIAN_POINT('Ctrl Pts',(-72.7375178548828,-5.43017230236482,
4.76778701764722));
#41131=CARTESIAN_POINT('Ctrl Pts',(-72.6384300696661,-7.04815863071909,
1.59437266510551));
#41132=CARTESIAN_POINT('Ctrl Pts',(-72.5393422844495,-6.95353321004791,
-1.96645370547505));
#41133=CARTESIAN_POINT('Ctrl Pts',(-72.4402544992328,-5.16928879855788,
-5.04945715855869));
#41134=CARTESIAN_POINT('Ctrl Pts',(-72.3411667140161,-2.12897380262748,
-6.90550757198495));
#41135=CARTESIAN_POINT('Ctrl Pts',(-72.2420789287995,1.42865440073498,-7.08360860594911));
#41136=CARTESIAN_POINT('Ctrl Pts',(-72.1429911435827,4.63913798942724,-5.5404840035929));
#41137=CARTESIAN_POINT('Ctrl Pts',(-72.0439033583662,6.72237081060478,-2.65109316391267));
#41138=CARTESIAN_POINT('Ctrl Pts',(-71.9448155731494,7.17215412606752,0.882479161764341));
#41139=CARTESIAN_POINT('Ctrl Pts',(-71.8457277879328,5.87919638451302,4.20162041971245));
#41140=CARTESIAN_POINT('Ctrl Pts',(-71.7466400027162,3.15766966054934,6.49982204324565));
#41141=CARTESIAN_POINT('Ctrl Pts',(-71.6475522174994,-0.331130112098027,
7.21865064453721));
#41142=CARTESIAN_POINT('Ctrl Pts',(-71.5484644322828,-3.739469533305,6.18344013381704));
#41143=CARTESIAN_POINT('Ctrl Pts',(-71.4493766470661,-6.23916603181327,
3.64573332904139));
#41144=CARTESIAN_POINT('Ctrl Pts',(-71.3502888618495,-7.2228255609445,0.222160291641919));
#41145=CARTESIAN_POINT('Ctrl Pts',(-71.2512010766328,-6.45143152716054,
-3.25539483463601));
#41146=CARTESIAN_POINT('Ctrl Pts',(-71.1521132914161,-4.11242274315051,
-5.94193095387636));
#41147=CARTESIAN_POINT('Ctrl Pts',(-71.0530255061994,-0.774148211036802,
-7.18465439853331));
#41148=CARTESIAN_POINT('Ctrl Pts',(-70.9539377209828,2.75223436335765,-6.68159938099921));
#41149=CARTESIAN_POINT('Ctrl Pts',(-70.854849935766,5.60985944324648,-4.55500178990458));
#41150=CARTESIAN_POINT('Ctrl Pts',(-70.7557621505494,7.1043609477079,-1.32159744389068));
#41151=CARTESIAN_POINT('Ctrl Pts',(-70.6566743653327,6.87259426414465,2.23293805544664));
#41152=CARTESIAN_POINT('Ctrl Pts',(-70.5575865801161,4.97087571091718,5.2448983732413));
#41153=CARTESIAN_POINT('Ctrl Pts',(-70.4584987948994,1.86129839747995,6.98241595399145));
#41154=CARTESIAN_POINT('Ctrl Pts',(-70.3594110096826,-1.70055044827962,
7.02329640922776));
#41155=CARTESIAN_POINT('Ctrl Pts',(-70.2603232244661,-4.84918744252938,
5.35760631497228));
#41156=CARTESIAN_POINT('Ctrl Pts',(-70.1612354392494,-6.81953435813275,
2.3900869057971));
#41157=CARTESIAN_POINT('Ctrl Pts',(-70.0621476540327,-7.13282227768603,
-1.15819283107837));
#41158=CARTESIAN_POINT('Ctrl Pts',(-69.963059868816,-5.7129262726844,-4.42504663047611));
#41159=CARTESIAN_POINT('Ctrl Pts',(-69.8639720835993,-2.90486278046528,
-6.61667110454216));
#41160=CARTESIAN_POINT('Ctrl Pts',(-69.7648842983827,0.60904494537379,-7.20052973978515));
#41161=CARTESIAN_POINT('Ctrl Pts',(-69.6657965131661,3.97496259553755,-6.03475240942767));
#41162=CARTESIAN_POINT('Ctrl Pts',(-69.5667087279493,6.37501554263063,-3.40260798656466));
#41163=CARTESIAN_POINT('Ctrl Pts',(-69.4676209427327,7.22602183930585,0.0563263427741025));
#41164=CARTESIAN_POINT('Ctrl Pts',(-69.368533157516,6.32119791860038,3.50157409644544));
#41165=CARTESIAN_POINT('Ctrl Pts',(-69.2694453722993,3.88040433680823,6.09598445387589));
#41166=CARTESIAN_POINT('Ctrl Pts',(-69.1703575870827,0.496722490665502,
7.20914912082417));
#41167=CARTESIAN_POINT('Ctrl Pts',(-69.0712698018661,-3.00765652165812,
6.57058342361997));
#41168=CARTESIAN_POINT('Ctrl Pts',(-68.9721820166493,-5.78121374549653,
4.33545060032828));
#41169=CARTESIAN_POINT('Ctrl Pts',(-68.8730942314327,-7.15001050594207,
1.04685913280926));
#41170=CARTESIAN_POINT('Ctrl Pts',(-68.774006446216,-6.78144682379192,-2.49610561777696));
#41171=CARTESIAN_POINT('Ctrl Pts',(-68.6749186609993,-4.76507892577756,
-5.43254885942832));
#41172=CARTESIAN_POINT('Ctrl Pts',(-68.5758308757826,-1.59085823514435,
-7.0489527133376));
#41173=CARTESIAN_POINT('Ctrl Pts',(-68.4767430905659,1.96992051229933,-6.95255186631505));
#41174=CARTESIAN_POINT('Ctrl Pts',(-68.3776553053493,5.05203395289501,-5.16677048247999));
#41175=CARTESIAN_POINT('Ctrl Pts',(-68.2785675201327,6.90656822591218,-2.12553043232278));
#41176=CARTESIAN_POINT('Ctrl Pts',(-68.179479734916,7.08289539441553,1.43218613014226));
#41177=CARTESIAN_POINT('Ctrl Pts',(-68.0803919496992,5.53817022743053,4.64189991420173));
#41178=CARTESIAN_POINT('Ctrl Pts',(-67.9813041644827,2.64774104169769,6.72369181655289));
#41179=CARTESIAN_POINT('Ctrl Pts',(-67.8822163792659,-0.886055109091175,
7.17171322992696));
#41180=CARTESIAN_POINT('Ctrl Pts',(-67.7831285940493,-4.2045512798272,5.87710070992006));
#41181=CARTESIAN_POINT('Ctrl Pts',(-67.6840408088326,-6.5013956613676,3.15442844655903));
#41182=CARTESIAN_POINT('Ctrl Pts',(-67.5849530236159,-7.21848463861485,
-0.334729326969879));
#41183=CARTESIAN_POINT('Ctrl Pts',(-67.4858652383994,-6.18157486775541,
-3.74255211578994));
#41184=CARTESIAN_POINT('Ctrl Pts',(-67.3867774531825,-3.64262198451628,
-6.24098309687747));
#41185=CARTESIAN_POINT('Ctrl Pts',(-67.287689667966,-0.218558994684405,
-7.22293529562393));
#41186=CARTESIAN_POINT('Ctrl Pts',(-67.1886018827493,3.25861123708332,-6.44980785450514));
#41187=CARTESIAN_POINT('Ctrl Pts',(-67.0895140975325,5.94398046764703,-4.10945900406941));
#41188=CARTESIAN_POINT('Ctrl Pts',(-66.990426312316,7.18503993028725,-0.770566970261787));
#41189=CARTESIAN_POINT('Ctrl Pts',(-66.8913385270992,6.68022540195615,2.7555678061177));
#41190=CARTESIAN_POINT('Ctrl Pts',(-66.7922507418826,4.5522059096846,5.6121251770881));
#41191=CARTESIAN_POINT('Ctrl Pts',(-66.693162956666,1.31805142041421,7.10502855866105));
#41192=CARTESIAN_POINT('Ctrl Pts',(-66.5940751714492,-2.23635716309218,
6.87146071173886));
#41193=CARTESIAN_POINT('Ctrl Pts',(-66.4949873862326,-5.2473910361686,4.96829921252571));
#41194=CARTESIAN_POINT('Ctrl Pts',(-66.395899601016,-6.9833130755638,1.85773707522965));
#41195=CARTESIAN_POINT('Ctrl Pts',(-66.2968118157991,-7.02250852220407,
-1.70388912091449));
#41196=CARTESIAN_POINT('Ctrl Pts',(-66.1977240305827,-5.35506230134601,
-4.85219885400573));
#41197=CARTESIAN_POINT('Ctrl Pts',(-66.1316655071048,-3.37628014142085,
-6.16377412581316));
#41198=CARTESIAN_POINT('Ctrl Pts',(-66.0986362453659,-2.28983447448481,
-6.54393972156383));
#41199=CARTESIAN_POINT('Ctrl Pts',(-67.5941716636062,-6.9334612849287,-0.000104716709421631));
#41200=CARTESIAN_POINT('Ctrl Pts',(-67.5910987836095,-6.93353940129172,
-0.107169118010251));
#41201=CARTESIAN_POINT('Ctrl Pts',(-67.5880259036127,-6.93111060609849,
-0.214229973520828));
#41202=CARTESIAN_POINT('Ctrl Pts',(-67.5849530236159,-6.92615151393041,
-0.321173496184973));
#41203=CARTESIAN_POINT('Ctrl Pts',(-67.5519237618771,-6.87284804832839,
-1.47067025657647));
#41204=CARTESIAN_POINT('Ctrl Pts',(-67.5188945001382,-6.52721145804193,
-2.60661118618316));
#41205=CARTESIAN_POINT('Ctrl Pts',(-67.4858652383993,-5.93123434902551,
-3.59098681450111));
#41206=CARTESIAN_POINT('Ctrl Pts',(-67.4528359766604,-5.33525724000907,
-4.57536244281908));
#41207=CARTESIAN_POINT('Ctrl Pts',(-67.4198067149215,-4.48893961226268,
-5.40817276984829));
#41208=CARTESIAN_POINT('Ctrl Pts',(-67.3867774531826,-3.49510363341746,
-5.98823663315398));
#41209=CARTESIAN_POINT('Ctrl Pts',(-67.3537481914437,-2.50126765457231,
-6.56830049645963));
#41210=CARTESIAN_POINT('Ctrl Pts',(-67.3207189297048,-1.35991332462838,
-6.89561789604178));
#41211=CARTESIAN_POINT('Ctrl Pts',(-67.2876896679659,-0.209707787695129,
-6.93042202231306));
#41212=CARTESIAN_POINT('Ctrl Pts',(-67.2546604062271,0.940497749238154,
-6.96522614858434));
#41213=CARTESIAN_POINT('Ctrl Pts',(-67.2216311444882,2.09955449316073,-6.70751700154474));
#41214=CARTESIAN_POINT('Ctrl Pts',(-67.1886018827493,3.12664440354932,-6.18860428628565));
#41215=CARTESIAN_POINT('Ctrl Pts',(-67.1555726210104,4.15373431393791,-5.66969157102655));
#41216=CARTESIAN_POINT('Ctrl Pts',(-67.1225433592715,5.04885739079248,-4.88957528754798));
#41217=CARTESIAN_POINT('Ctrl Pts',(-67.0895140975326,5.70326217299314,-3.94303514017407));
#41218=CARTESIAN_POINT('Ctrl Pts',(-67.0564848357937,6.35766695519376,-2.99649499280022));
#41219=CARTESIAN_POINT('Ctrl Pts',(-67.0234555740548,6.77135344274051,-1.88353098153098));
#41220=CARTESIAN_POINT('Ctrl Pts',(-66.9904263123159,6.89406093179203,-0.739359846499843));
#41221=CARTESIAN_POINT('Ctrl Pts',(-66.9573970505771,7.01676842084356,0.404811288531357));
#41222=CARTESIAN_POINT('Ctrl Pts',(-66.9243677888382,6.84849691139986,1.58018954732452));
#41223=CARTESIAN_POINT('Ctrl Pts',(-66.8913385270993,6.40969124129941,2.64397157188285));
#41224=CARTESIAN_POINT('Ctrl Pts',(-66.8583092653603,5.97088557119897,3.70775359644117));
#41225=CARTESIAN_POINT('Ctrl Pts',(-66.8252800036215,5.26154574044179,4.65993938676463));
#41226=CARTESIAN_POINT('Ctrl Pts',(-66.7922507418826,4.36785007685146,5.38484951218853));
#41227=CARTESIAN_POINT('Ctrl Pts',(-66.7592214801437,3.47415441326111,6.10975963761244));
#41228=CARTESIAN_POINT('Ctrl Pts',(-66.7261922184048,2.39610291683771,6.60739409813673));
#41229=CARTESIAN_POINT('Ctrl Pts',(-66.6931629566659,1.26467573804154,6.81728335391186));
#41230=CARTESIAN_POINT('Ctrl Pts',(-66.6601336949271,0.133248559245465,
7.02717260968697));
#41231=CARTESIAN_POINT('Ctrl Pts',(-66.6271044331882,-1.05155430192337,
6.94931666071291));
#41232=CARTESIAN_POINT('Ctrl Pts',(-66.5940751714492,-2.14579471135379,
6.59319510302372));
#41233=CARTESIAN_POINT('Ctrl Pts',(-66.5662901142995,-3.06629764453912,
6.29361656836326));
#41234=CARTESIAN_POINT('Ctrl Pts',(-66.5385050571497,-3.92271312249685,
5.79712049892313));
#41235=CARTESIAN_POINT('Ctrl Pts',(-66.51072,-4.64244039278582,5.14956429285673));
#41236=CARTESIAN_POINT('',(-86.51072,-2.05430500584057,-5.87042930427706));
#41237=CARTESIAN_POINT('Ctrl Pts',(-86.51072,-2.0543050058407,-5.87042930427701));
#41238=CARTESIAN_POINT('Ctrl Pts',(-86.51072,-2.21258203238063,-5.82486884494219));
#41239=CARTESIAN_POINT('Ctrl Pts',(-86.51072,-2.36882106524609,-5.77305057653388));
#41240=CARTESIAN_POINT('Ctrl Pts',(-86.51072,-2.52263632570939,-5.71505524575264));
#41241=CARTESIAN_POINT('Ctrl Pts',(-86.51072,-2.68507439158213,-5.65380872617208));
#41242=CARTESIAN_POINT('Ctrl Pts',(-86.51072,-2.84481012954198,-5.58567374017774));
#41243=CARTESIAN_POINT('Ctrl Pts',(-86.51072,-3.00150353946984,-5.510969810184));
#41244=CARTESIAN_POINT('Ctrl Pts',(-86.51072,-3.10062155384214,-5.46371507745341));
#41245=CARTESIAN_POINT('Ctrl Pts',(-86.51072,-3.19852205088825,-5.41383083132198));
#41246=CARTESIAN_POINT('Ctrl Pts',(-86.51072,-3.29511573121791,-5.36138774998078));
#41247=CARTESIAN_POINT('Ctrl Pts',(-86.51072,-3.36158388237246,-5.32530055829598));
#41248=CARTESIAN_POINT('Ctrl Pts',(-86.51072,-3.42743318663604,-5.28800156865333));
#41249=CARTESIAN_POINT('Ctrl Pts',(-86.51072,-3.49263358329869,-5.24951180053227));
#41250=CARTESIAN_POINT('Ctrl Pts',(-86.51072,-3.5235350127469,-5.23126975117442));
#41251=CARTESIAN_POINT('Ctrl Pts',(-86.51072,-3.55429475124542,-5.21275759435068));
#41252=CARTESIAN_POINT('Ctrl Pts',(-86.51072,-3.5848840724756,-5.19399336730484));
#41253=CARTESIAN_POINT('Ctrl Pts',(-86.51072,-3.73562442368972,-5.10152560203904));
#41254=CARTESIAN_POINT('Ctrl Pts',(-86.51072,-3.88233609651536,-5.00287892045257));
#41255=CARTESIAN_POINT('Ctrl Pts',(-86.51072,-4.02466996944556,-4.89838649052438));
#41256=CARTESIAN_POINT('Ctrl Pts',(-86.51072,-4.16747158240373,-4.79355067577084));
#41257=CARTESIAN_POINT('Ctrl Pts',(-86.51072,-4.30586721806361,-4.68283025738495));
#41258=CARTESIAN_POINT('Ctrl Pts',(-86.51072,-4.43948328000296,-4.56651347834845));
#41259=CARTESIAN_POINT('Ctrl Pts',(-86.51072,-4.55409609756718,-4.46673959202169));
#41260=CARTESIAN_POINT('Ctrl Pts',(-86.51072,-4.66519208352877,-4.36284708277001));
#41261=CARTESIAN_POINT('Ctrl Pts',(-86.51072,-4.7725177187907,-4.25499289066315));
#41262=CARTESIAN_POINT('Ctrl Pts',(-86.51072,-4.78886696746902,-4.23856312527251));
#41263=CARTESIAN_POINT('Ctrl Pts',(-86.51072,-4.80512868733647,-4.222041387261));
#41264=CARTESIAN_POINT('Ctrl Pts',(-86.51072,-4.82130194150653,-4.20542818885453));
#41265=CARTESIAN_POINT('Ctrl Pts',(-86.51072,-4.83838504707905,-4.18788038930284));
#41266=CARTESIAN_POINT('Ctrl Pts',(-86.51072,-4.85536377248283,-4.17023635893039));
#41267=CARTESIAN_POINT('Ctrl Pts',(-86.51072,-4.87223399895435,-4.1525003326935));
#41268=CARTESIAN_POINT('Ctrl Pts',(-86.51072,-4.94423933928611,-4.07679959402962));
#41269=CARTESIAN_POINT('Ctrl Pts',(-86.51072,-5.01428728250921,-3.99940388048743));
#41270=CARTESIAN_POINT('Ctrl Pts',(-86.51072,-5.08230936468395,-3.92037913736578));
#41271=CARTESIAN_POINT('Ctrl Pts',(-86.51072,-5.19718047715216,-3.78692747189664));
#41272=CARTESIAN_POINT('Ctrl Pts',(-86.51072,-5.30627615206813,-3.64883247781431));
#41273=CARTESIAN_POINT('Ctrl Pts',(-86.51072,-5.40947963808152,-3.50655586542704));
#41274=CARTESIAN_POINT('Ctrl Pts',(-86.51072,-5.51401899965164,-3.3624376112879));
#41275=CARTESIAN_POINT('Ctrl Pts',(-86.51072,-5.61251306134529,-3.214028262726));
#41276=CARTESIAN_POINT('Ctrl Pts',(-86.51072,-5.70480528363513,-3.06176720920456));
#41277=CARTESIAN_POINT('Ctrl Pts',(-86.51072,-5.7988808937585,-2.90656397373501));
#41278=CARTESIAN_POINT('Ctrl Pts',(-86.51072,-5.88651318998411,-2.74735818652822));
#41279=CARTESIAN_POINT('Ctrl Pts',(-86.51072,-5.96749284788747,-2.58458156019617));
#41280=CARTESIAN_POINT('Ctrl Pts',(-86.51072,-6.02822759131498,-2.46249909044713));
#41281=CARTESIAN_POINT('Ctrl Pts',(-86.51072,-6.08521936563103,-2.33840726205514));
#41282=CARTESIAN_POINT('Ctrl Pts',(-86.51072,-6.13836158920561,-2.21247913102859));
#41283=CARTESIAN_POINT('Ctrl Pts',(-86.51072,-6.15312996736535,-2.17748333795005));
#41284=CARTESIAN_POINT('Ctrl Pts',(-86.51072,-6.16760094584908,-2.14234569051137));
#41285=CARTESIAN_POINT('Ctrl Pts',(-86.51072,-6.18177200434075,-2.10706982588161));
#41286=CARTESIAN_POINT('Ctrl Pts',(-86.51072,-6.19016620801788,-2.0861742242748));
#41287=CARTESIAN_POINT('Ctrl Pts',(-86.51072,-6.19845156921919,-2.06523907577952));
#41288=CARTESIAN_POINT('Ctrl Pts',(-86.51072,-6.20662688291449,-2.04426772949609));
#41289=CARTESIAN_POINT('Ctrl Pts',(-86.51072,-6.27282658558699,-1.87445199638191));
#41290=CARTESIAN_POINT('Ctrl Pts',(-86.51072,-6.33183472169884,-1.70221357249591));
#41291=CARTESIAN_POINT('Ctrl Pts',(-86.51072,-6.38350915294916,-1.52801731240776));
#41292=CARTESIAN_POINT('Ctrl Pts',(-86.51072,-6.43097870038066,-1.36799585826559));
#41293=CARTESIAN_POINT('Ctrl Pts',(-86.51072,-6.47225930007859,-1.20632141719495));
#41294=CARTESIAN_POINT('Ctrl Pts',(-86.51072,-6.5072089203001,-1.04333227579861));
#41295=CARTESIAN_POINT('Ctrl Pts',(-86.51072,-6.54508051000339,-0.866716397001247));
#41296=CARTESIAN_POINT('Ctrl Pts',(-86.51072,-6.57551927259713,-0.688556492077032));
#41297=CARTESIAN_POINT('Ctrl Pts',(-86.51072,-6.59859730560256,-0.509314630244122));
#41298=CARTESIAN_POINT('Ctrl Pts',(-86.51072,-6.62179814420949,-0.329118965084463));
#41299=CARTESIAN_POINT('Ctrl Pts',(-86.51072,-6.63755977647099,-0.147829089728884));
#41300=CARTESIAN_POINT('Ctrl Pts',(-86.51072,-6.64590383774985,0.0340957911597833));
#41301=CARTESIAN_POINT('Ctrl Pts',(-86.51072,-6.65018668746203,0.127474410721004));
#41302=CARTESIAN_POINT('Ctrl Pts',(-86.51072,-6.65251448290405,0.221020427310341));
#41303=CARTESIAN_POINT('Ctrl Pts',(-86.51072,-6.65288481617016,0.314671846891448));
#41304=CARTESIAN_POINT('Ctrl Pts',(-86.51072,-6.65298022561412,0.338799384669037));
#41305=CARTESIAN_POINT('Ctrl Pts',(-86.51072,-6.65294569190618,0.362933917091072));
#41306=CARTESIAN_POINT('Ctrl Pts',(-86.51072,-6.65278113473496,0.387074380312947));
#41307=CARTESIAN_POINT('Ctrl Pts',(-86.51072,-6.65264760834661,0.406662641602241));
#41308=CARTESIAN_POINT('Ctrl Pts',(-86.51072,-6.65242845612529,0.426253125446996));
#41309=CARTESIAN_POINT('Ctrl Pts',(-86.51072,-6.65212390032766,0.44583583961078));
#41310=CARTESIAN_POINT('Ctrl Pts',(-86.51072,-6.64926295208706,0.629792710789254));
#41311=CARTESIAN_POINT('Ctrl Pts',(-86.51072,-6.63886861132718,0.813294091649382));
#41312=CARTESIAN_POINT('Ctrl Pts',(-86.51072,-6.62105508637465,0.99586126198024));
#41313=CARTESIAN_POINT('Ctrl Pts',(-86.51072,-6.60311620074966,1.17971322817846));
#41314=CARTESIAN_POINT('Ctrl Pts',(-86.51072,-6.57765339445709,1.3626185090582));
#41315=CARTESIAN_POINT('Ctrl Pts',(-86.51072,-6.54473157195455,1.54409959934158));
#41316=CARTESIAN_POINT('Ctrl Pts',(-86.51072,-6.51186414550787,1.72528083212095));
#41317=CARTESIAN_POINT('Ctrl Pts',(-86.51072,-6.47156232283033,1.90504331604601));
#41318=CARTESIAN_POINT('Ctrl Pts',(-86.51072,-6.42383907511914,2.08291224064793));
#41319=CARTESIAN_POINT('Ctrl Pts',(-86.51072,-6.40891009319694,2.13855392656113));
#41320=CARTESIAN_POINT('Ctrl Pts',(-86.51072,-6.39325447880982,2.19401026896043));
#41321=CARTESIAN_POINT('Ctrl Pts',(-86.51072,-6.37687159035412,2.2492665620533));
#41322=CARTESIAN_POINT('Ctrl Pts',(-86.51072,-6.33649222484637,2.38545830024617));
#41323=CARTESIAN_POINT('Ctrl Pts',(-86.51072,-6.29169596317493,2.5204351980553));
#41324=CARTESIAN_POINT('Ctrl Pts',(-86.51072,-6.24259276678192,2.65402287965289));
#41325=CARTESIAN_POINT('Ctrl Pts',(-86.51072,-6.22111011835998,2.71246749035183));
#41326=CARTESIAN_POINT('Ctrl Pts',(-86.51072,-6.19880287065572,2.77064611712136));
#41327=CARTESIAN_POINT('Ctrl Pts',(-86.51072,-6.17567920954438,2.8285437301309));
#41328=CARTESIAN_POINT('Ctrl Pts',(-86.51072,-6.16282195963146,2.86073604069284));
#41329=CARTESIAN_POINT('Ctrl Pts',(-86.51072,-6.14971229671456,2.89284146794668));
#41330=CARTESIAN_POINT('Ctrl Pts',(-86.51072,-6.13635154810387,2.92485738642242));
#41331=CARTESIAN_POINT('Ctrl Pts',(-86.51072,-6.12730729434025,2.94652983155313));
#41332=CARTESIAN_POINT('Ctrl Pts',(-86.51072,-6.11814757446991,2.96816209171322));
#41333=CARTESIAN_POINT('Ctrl Pts',(-86.51072,-6.1088795489188,2.98973796773027));
#41334=CARTESIAN_POINT('Ctrl Pts',(-86.51072,-6.03607183109103,3.15923364771886));
#41335=CARTESIAN_POINT('Ctrl Pts',(-86.51072,-5.95649247563341,3.32547331851885));
#41336=CARTESIAN_POINT('Ctrl Pts',(-86.51072,-5.87047713602277,3.48810950866876));
#41337=CARTESIAN_POINT('Ctrl Pts',(-86.51072,-5.7829205374938,3.65365988226137));
#41338=CARTESIAN_POINT('Ctrl Pts',(-86.51072,-5.68869505582976,3.8154771215784));
#41339=CARTESIAN_POINT('Ctrl Pts',(-86.51072,-5.58810168441886,3.9731849792754));
#41340=CARTESIAN_POINT('Ctrl Pts',(-86.51072,-5.48731664960083,4.13119332223216));
#41341=CARTESIAN_POINT('Ctrl Pts',(-86.51072,-5.38013910716857,4.28507725418091));
#41342=CARTESIAN_POINT('Ctrl Pts',(-86.51072,-5.26682312986106,4.4344389749387));
#41343=CARTESIAN_POINT('Ctrl Pts',(-86.51072,-5.15467074727413,4.58226696220309));
#41344=CARTESIAN_POINT('Ctrl Pts',(-86.51072,-5.03650494943115,4.72566571734121));
#41345=CARTESIAN_POINT('Ctrl Pts',(-86.51072,-4.91253002400078,4.8642215159004));
#41346=CARTESIAN_POINT('Ctrl Pts',(-86.51072,-4.82526136656507,4.96175396835574));
#41347=CARTESIAN_POINT('Ctrl Pts',(-86.51072,-4.73511337439158,5.0568861415784));
#41348=CARTESIAN_POINT('Ctrl Pts',(-86.51072,-4.64214617842369,5.1494628708387));
#41349=CARTESIAN_POINT('Ctrl Pts',(-86.51072,-2.05430500584057,-5.87042930427706));
#41350=CARTESIAN_POINT('Ctrl Pts',(-86.4829349428503,-1.2342747841181,-6.15647891042869));
#41351=CARTESIAN_POINT('Ctrl Pts',(-86.4221206239616,0.693371089156462,
-6.40526944857501));
#41352=CARTESIAN_POINT('Ctrl Pts',(-86.3282770433341,3.55493808738742,-5.42058662271333));
#41353=CARTESIAN_POINT('Ctrl Pts',(-86.2291892581173,5.71261075920097,-3.06370552006469));
#41354=CARTESIAN_POINT('Ctrl Pts',(-86.1301014729008,6.48219330078747,0.0375972645595515));
#41355=CARTESIAN_POINT('Ctrl Pts',(-86.031013687684,5.67668603654431,3.12977391169855));
#41356=CARTESIAN_POINT('Ctrl Pts',(-85.9319259024675,3.49181736371615,5.46145112616022));
#41357=CARTESIAN_POINT('Ctrl Pts',(-85.8328381172506,0.45848197210095,6.46606838804796));
#41358=CARTESIAN_POINT('Ctrl Pts',(-85.7337503320341,-2.68625859143277,
5.89951319007443));
#41359=CARTESIAN_POINT('Ctrl Pts',(-85.6346625468174,-5.17827294326576,
3.89945285036088));
#41360=CARTESIAN_POINT('Ctrl Pts',(-85.5588309088861,-6.12246698761767,
1.64367910817076));
#41361=CARTESIAN_POINT('Ctrl Pts',(-85.5160285326938,-6.21932780933381,
0.305694574820658));
#41362=CARTESIAN_POINT('Ctrl Pts',(-85.5062554182403,-6.21904930984993,
0.000151106537523774));
#41363=CARTESIAN_POINT('Origin',(-86.51072,-1.12618006296016E-15,0.));
#41364=CARTESIAN_POINT('',(-86.51072,4.88092761120804,-3.85429840783598));
#41365=CARTESIAN_POINT('Ctrl Pts',(-86.51072,1.15840596835156,6.83581456945577));
#41366=CARTESIAN_POINT('Ctrl Pts',(-86.51072,1.33692099159029,6.79654210588011));
#41367=CARTESIAN_POINT('Ctrl Pts',(-86.51072,1.51361902021433,6.75022761845211));
#41368=CARTESIAN_POINT('Ctrl Pts',(-86.51072,1.68807314422841,6.69687225419658));
#41369=CARTESIAN_POINT('Ctrl Pts',(-86.51072,1.8679641935395,6.64185405089215));
#41370=CARTESIAN_POINT('Ctrl Pts',(-86.51072,2.04547001034044,6.57934922676145));
#41371=CARTESIAN_POINT('Ctrl Pts',(-86.51072,2.22017980815463,6.5096135659802));
#41372=CARTESIAN_POINT('Ctrl Pts',(-86.51072,2.32989175485023,6.46582188861501));
#41373=CARTESIAN_POINT('Ctrl Pts',(-86.51072,2.43850069933779,6.41917781777568));
#41374=CARTESIAN_POINT('Ctrl Pts',(-86.51072,2.54589939897303,6.36973577164565));
#41375=CARTESIAN_POINT('Ctrl Pts',(-86.51072,2.61317957816801,6.33876268040066));
#41376=CARTESIAN_POINT('Ctrl Pts',(-86.51072,2.67998471465285,6.30669141181624));
#41377=CARTESIAN_POINT('Ctrl Pts',(-86.51072,2.746287399481,6.27353409609559));
#41378=CARTESIAN_POINT('Ctrl Pts',(-86.51072,2.77514683716407,6.25910177726479));
#41379=CARTESIAN_POINT('Ctrl Pts',(-86.51072,2.80391107023024,6.24446368602063));
#41380=CARTESIAN_POINT('Ctrl Pts',(-86.51072,2.8325777855864,6.22962076918156));
#41381=CARTESIAN_POINT('Ctrl Pts',(-86.51072,2.85655241758811,6.21720729715912));
#41382=CARTESIAN_POINT('Ctrl Pts',(-86.51072,2.88045005876997,6.20465510637532));
#41383=CARTESIAN_POINT('Ctrl Pts',(-86.51072,2.9042688372644,6.19196540548103));
#41384=CARTESIAN_POINT('Ctrl Pts',(-86.51072,3.06900614318828,6.10419989984044));
#41385=CARTESIAN_POINT('Ctrl Pts',(-86.51072,3.22998445162522,6.00985446247505));
#41386=CARTESIAN_POINT('Ctrl Pts',(-86.51072,3.3868033547833,5.90918193833376));
#41387=CARTESIAN_POINT('Ctrl Pts',(-86.51072,3.542839639644,5.80901182913002));
#41388=CARTESIAN_POINT('Ctrl Pts',(-86.51072,3.69475849445778,5.70257718309574));
#41389=CARTESIAN_POINT('Ctrl Pts',(-86.51072,3.84213367303502,5.59008687856596));
#41390=CARTESIAN_POINT('Ctrl Pts',(-86.51072,3.9701437417514,5.49237780874973));
#41391=CARTESIAN_POINT('Ctrl Pts',(-86.51072,4.09472550320262,5.3900991786712));
#41392=CARTESIAN_POINT('Ctrl Pts',(-86.51072,4.21557502487895,5.28336686568389));
#41393=CARTESIAN_POINT('Ctrl Pts',(-86.51072,4.23486407962035,5.26633108929578));
#41394=CARTESIAN_POINT('Ctrl Pts',(-86.51072,4.25405799861312,5.24918181409541));
#41395=CARTESIAN_POINT('Ctrl Pts',(-86.51072,4.27315548388442,5.23191947067406));
#41396=CARTESIAN_POINT('Ctrl Pts',(-86.51072,4.29206103730179,5.21483061572666));
#41397=CARTESIAN_POINT('Ctrl Pts',(-86.51072,4.31086653414738,5.19763593809285));
#41398=CARTESIAN_POINT('Ctrl Pts',(-86.51072,4.32956613773457,5.18034051383287));
#41399=CARTESIAN_POINT('Ctrl Pts',(-86.51072,4.41032297928591,5.10564781620356));
#41400=CARTESIAN_POINT('Ctrl Pts',(-86.51072,4.4891337278863,5.0290507628448));
#41401=CARTESIAN_POINT('Ctrl Pts',(-86.51072,4.56591797340772,4.95060089892119));
#41402=CARTESIAN_POINT('Ctrl Pts',(-86.51072,4.6939867687781,4.81975401097639));
#41403=CARTESIAN_POINT('Ctrl Pts',(-86.51072,4.81642027662916,4.6837546034005));
#41404=CARTESIAN_POINT('Ctrl Pts',(-86.51072,4.93302139785161,4.54303258748792));
#41405=CARTESIAN_POINT('Ctrl Pts',(-86.51072,5.05026750854921,4.40153215522537));
#41406=CARTESIAN_POINT('Ctrl Pts',(-86.51072,5.16161690091574,4.25525608476221));
#41407=CARTESIAN_POINT('Ctrl Pts',(-86.51072,5.26682651345902,4.10461066568728));
#41408=CARTESIAN_POINT('Ctrl Pts',(-86.51072,5.37240253202624,3.95344060454123));
#41409=CARTESIAN_POINT('Ctrl Pts',(-86.51072,5.47179630518351,3.79787005449489));
#41410=CARTESIAN_POINT('Ctrl Pts',(-86.51072,5.56471377525825,3.63828838878779));
#41411=CARTESIAN_POINT('Ctrl Pts',(-86.51072,5.63440187781431,3.51860213950746));
#41412=CARTESIAN_POINT('Ctrl Pts',(-86.51072,5.70044609905939,3.39665914206459));
#41413=CARTESIAN_POINT('Ctrl Pts',(-86.51072,5.76270266675695,3.27261923926715));
#41414=CARTESIAN_POINT('Ctrl Pts',(-86.51072,5.77939659018424,3.23935828840188));
#41415=CARTESIAN_POINT('Ctrl Pts',(-86.51072,5.79581807160992,3.2059465515095));
#41416=CARTESIAN_POINT('Ctrl Pts',(-86.51072,5.81196411860362,3.17238708947047));
#41417=CARTESIAN_POINT('Ctrl Pts',(-86.51072,5.82152069713481,3.15252379819144));
#41418=CARTESIAN_POINT('Ctrl Pts',(-86.51072,5.83098064485861,3.13260893175539));
#41419=CARTESIAN_POINT('Ctrl Pts',(-86.51072,5.84033745115676,3.11265599748321));
#41420=CARTESIAN_POINT('Ctrl Pts',(-86.51072,5.91732823406407,2.94847689812347));
#41421=CARTESIAN_POINT('Ctrl Pts',(-86.51072,5.98744586695114,2.78150324016161));
#41422=CARTESIAN_POINT('Ctrl Pts',(-86.51072,6.05048064190744,2.61213298066552));
#41423=CARTESIAN_POINT('Ctrl Pts',(-86.51072,6.11164633069412,2.4477848317392));
#41424=CARTESIAN_POINT('Ctrl Pts',(-86.51072,6.16614302472095,2.28117943087884));
#41425=CARTESIAN_POINT('Ctrl Pts',(-86.51072,6.21373523303752,2.11266378330039));
#41426=CARTESIAN_POINT('Ctrl Pts',(-86.51072,6.26289076481001,1.9386126820444));
#41427=CARTESIAN_POINT('Ctrl Pts',(-86.51072,6.30468105067439,1.76252310782449));
#41428=CARTESIAN_POINT('Ctrl Pts',(-86.51072,6.33908486826123,1.58487065370346));
#41429=CARTESIAN_POINT('Ctrl Pts',(-86.51072,6.37335665238351,1.40789998639134));
#41430=CARTESIAN_POINT('Ctrl Pts',(-86.51072,6.40029851150814,1.22937766976392));
#41431=CARTESIAN_POINT('Ctrl Pts',(-86.51072,6.41983807680747,1.04977659578172));
#41432=CARTESIAN_POINT('Ctrl Pts',(-86.51072,6.42952443815511,0.960742839177272));
#41433=CARTESIAN_POINT('Ctrl Pts',(-86.51072,6.43739090288072,0.871444091179049));
#41434=CARTESIAN_POINT('Ctrl Pts',(-86.51072,6.44342398767677,0.781939070998599));
#41435=CARTESIAN_POINT('Ctrl Pts',(-86.51072,6.44512671191955,0.756677969445425));
#41436=CARTESIAN_POINT('Ctrl Pts',(-86.51072,6.44668338047881,0.731400443643511));
#41437=CARTESIAN_POINT('Ctrl Pts',(-86.51072,6.44809364563389,0.706107829474976));
#41438=CARTESIAN_POINT('Ctrl Pts',(-86.51072,6.44937238190223,0.683174140060691));
#41439=CARTESIAN_POINT('Ctrl Pts',(-86.51072,6.45053028956465,0.660235926315252));
#41440=CARTESIAN_POINT('Ctrl Pts',(-86.51072,6.45156713961303,0.6373001126248));
#41441=CARTESIAN_POINT('Ctrl Pts',(-86.51072,6.45963992153548,0.458724799418353));
#41442=CARTESIAN_POINT('Ctrl Pts',(-86.51072,6.46038493546743,0.280181222650435));
#41443=CARTESIAN_POINT('Ctrl Pts',(-86.51072,6.45382244972886,0.102127507862334));
#41444=CARTESIAN_POINT('Ctrl Pts',(-86.51072,6.4472673704612,-0.0757252541600348));
#41445=CARTESIAN_POINT('Ctrl Pts',(-86.51072,6.43342122692505,-0.25308999531447));
#41446=CARTESIAN_POINT('Ctrl Pts',(-86.51072,6.41225241327616,-0.429508005108766));
#41447=CARTESIAN_POINT('Ctrl Pts',(-86.51072,6.3913431695847,-0.603762794230776));
#41448=CARTESIAN_POINT('Ctrl Pts',(-86.51072,6.36328960685773,-0.777094595050165));
#41449=CARTESIAN_POINT('Ctrl Pts',(-86.51072,6.32801215972376,-0.949048880875677));
#41450=CARTESIAN_POINT('Ctrl Pts',(-86.51072,6.31879999759548,-0.993952094922312));
#41451=CARTESIAN_POINT('Ctrl Pts',(-86.51072,6.30909497216788,-1.03876127814759));
#41452=CARTESIAN_POINT('Ctrl Pts',(-86.51072,6.29889512145856,-1.08346810792257));
#41453=CARTESIAN_POINT('Ctrl Pts',(-86.51072,6.26977492480713,-1.21110445396444));
#41454=CARTESIAN_POINT('Ctrl Pts',(-86.51072,6.23662241077162,-1.33790715393257));
#41455=CARTESIAN_POINT('Ctrl Pts',(-86.51072,6.19950420606752,-1.46370056227431));
#41456=CARTESIAN_POINT('Ctrl Pts',(-86.51072,6.18326499150948,-1.51873517842382));
#41457=CARTESIAN_POINT('Ctrl Pts',(-86.51072,6.16626655521156,-1.57357650063582));
#41458=CARTESIAN_POINT('Ctrl Pts',(-86.51072,6.14851373823978,-1.62820926346126));
#41459=CARTESIAN_POINT('Ctrl Pts',(-86.51072,6.13799943741682,-1.66056611725236));
#41460=CARTESIAN_POINT('Ctrl Pts',(-86.51072,6.1272205118688,-1.69284980717819));
#41461=CARTESIAN_POINT('Ctrl Pts',(-86.51072,6.11617789691174,-1.72505709862759));
#41462=CARTESIAN_POINT('Ctrl Pts',(-86.51072,6.1076826296012,-1.74983470350426));
#41463=CARTESIAN_POINT('Ctrl Pts',(-86.51072,6.09903040399726,-1.77456940026785));
#41464=CARTESIAN_POINT('Ctrl Pts',(-86.51072,6.09022962359805,-1.79923786075214));
#41465=CARTESIAN_POINT('Ctrl Pts',(-86.51072,6.03143262794601,-1.96404499126166));
#41466=CARTESIAN_POINT('Ctrl Pts',(-86.51072,5.96593941819338,-2.12610508285074));
#41467=CARTESIAN_POINT('Ctrl Pts',(-86.51072,5.89400145244168,-2.28504090903752));
#41468=CARTESIAN_POINT('Ctrl Pts',(-86.51072,5.82166151986319,-2.44486481885369));
#41469=CARTESIAN_POINT('Ctrl Pts',(-86.51072,5.74280425690578,-2.60153010257179));
#41470=CARTESIAN_POINT('Ctrl Pts',(-86.51072,5.65763771959783,-2.75463161937262));
#41471=CARTESIAN_POINT('Ctrl Pts',(-86.51072,5.5729853246012,-2.90680887683164));
#41472=CARTESIAN_POINT('Ctrl Pts',(-86.51072,5.48209918836071,-3.05546585368127));
#41473=CARTESIAN_POINT('Ctrl Pts',(-86.51072,5.38514254021834,-3.20017426124779));
#41474=CARTESIAN_POINT('Ctrl Pts',(-86.51072,5.29007319202304,-3.34206586176525));
#41475=CARTESIAN_POINT('Ctrl Pts',(-86.51072,5.18916691890737,-3.48016157013249));
#41476=CARTESIAN_POINT('Ctrl Pts',(-86.51072,5.08254442327496,-3.61402073215818));
#41477=CARTESIAN_POINT('Ctrl Pts',(-86.51072,5.01746184271968,-3.69572862732539));
#41478=CARTESIAN_POINT('Ctrl Pts',(-86.51072,4.95024883314754,-3.77585727781971));
#41479=CARTESIAN_POINT('Ctrl Pts',(-86.51072,4.88092761120814,-3.85429840783586));
#41480=CARTESIAN_POINT('Origin',(-86.51072,0.,0.));
#41481=CARTESIAN_POINT('Origin',(-88.8777445817596,0.,0.));
#41482=CARTESIAN_POINT('Ctrl Pts',(-86.51072,4.88092761120804,-3.85429840783599));
#41483=CARTESIAN_POINT('Ctrl Pts',(-86.4776907382611,5.52083048049534,-3.04395129593469));
#41484=CARTESIAN_POINT('Ctrl Pts',(-86.4116322147833,6.38855598297889,-1.09916744813806));
#41485=CARTESIAN_POINT('Ctrl Pts',(-86.3125444295668,6.13724916597635,2.08678167705531));
#41486=CARTESIAN_POINT('Ctrl Pts',(-86.2134566443499,4.39481025566226,4.7650088956501));
#41487=CARTESIAN_POINT('Ctrl Pts',(-86.1143688591334,1.5844221326576,6.28572095298091));
#41488=CARTESIAN_POINT('Ctrl Pts',(-86.0152810739166,-1.61092755177724,
6.27892628422283));
#41489=CARTESIAN_POINT('Ctrl Pts',(-85.9161932886999,-4.41485865379402,
4.7465110522202));
#41490=CARTESIAN_POINT('Ctrl Pts',(-85.8286811246477,-5.94378959897448,
2.37447606712619));
#41491=CARTESIAN_POINT('Ctrl Pts',(-85.7741982223342,-6.21841544098032,
0.670637576511123));
#41492=CARTESIAN_POINT('Ctrl Pts',(-85.7527445817596,-6.21890566139956,
-0.00012576145485773));
#41493=CARTESIAN_POINT('Ctrl Pts',(-86.9228037546341,5.44108552132573,-4.29663558492217));
#41494=CARTESIAN_POINT('Ctrl Pts',(-86.8897744928952,6.15442661434643,-3.39328927679633));
#41495=CARTESIAN_POINT('Ctrl Pts',(-86.8237159694174,7.12173632351047,-1.22531300686443));
#41496=CARTESIAN_POINT('Ctrl Pts',(-86.7246281842008,6.84158836961276,2.32627042923568));
#41497=CARTESIAN_POINT('Ctrl Pts',(-86.625540398984,4.89917908148197,5.31186343587118));
#41498=CARTESIAN_POINT('Ctrl Pts',(-86.5264526137675,1.76625777155052,7.00709946810573));
#41499=CARTESIAN_POINT('Ctrl Pts',(-86.4273648285506,-1.79580507560737,
6.99952501161989));
#41500=CARTESIAN_POINT('Ctrl Pts',(-86.3282770433341,-4.92152832684868,
5.29124269406165));
#41501=CARTESIAN_POINT('Ctrl Pts',(-86.2291892581174,-6.85137477063435,
2.29721389573782));
#41502=CARTESIAN_POINT('Ctrl Pts',(-86.1301014729007,-7.11642976004538,
-1.25498724546614));
#41503=CARTESIAN_POINT('Ctrl Pts',(-86.0310136876841,-5.65228184978238,
-4.50225302768583));
#41504=CARTESIAN_POINT('Ctrl Pts',(-85.9319259024674,-2.8147033238205,-6.65552420937686));
#41505=CARTESIAN_POINT('Ctrl Pts',(-85.8328381172507,0.706812370959138,
-7.19159127052686));
#41506=CARTESIAN_POINT('Ctrl Pts',(-85.7337503320341,4.05658150791202,-5.98019305530335));
#41507=CARTESIAN_POINT('Ctrl Pts',(-85.6346625468173,6.42065372437976,-3.31568558097902));
#41508=CARTESIAN_POINT('Ctrl Pts',(-85.5355747616008,7.22458973766228,0.154491077408247));
#41509=CARTESIAN_POINT('Ctrl Pts',(-85.4364869763839,6.2730435466505,3.58712824513611));
#41510=CARTESIAN_POINT('Ctrl Pts',(-85.3373991911675,3.79722857138034,6.14813953415812));
#41511=CARTESIAN_POINT('Ctrl Pts',(-85.2383114059506,0.398735978739728,
7.21523208383319));
#41512=CARTESIAN_POINT('Ctrl Pts',(-85.1392236207341,-3.09664432369599,
6.52911620558032));
#41513=CARTESIAN_POINT('Ctrl Pts',(-85.0401358355173,-5.83957994631889,
4.25650919220943));
#41514=CARTESIAN_POINT('Ctrl Pts',(-84.9410480503007,-7.16357287155185,
0.949625284159334));
#41515=CARTESIAN_POINT('Ctrl Pts',(-84.8419602650841,-6.74690987362332,
-2.58800533649108));
#41516=CARTESIAN_POINT('Ctrl Pts',(-84.7428724798672,-4.69083469401064,
-5.49678399941974));
#41517=CARTESIAN_POINT('Ctrl Pts',(-84.6437846946508,-1.49494711354703,
-7.06991496359203));
#41518=CARTESIAN_POINT('Ctrl Pts',(-84.544696909434,2.06419335672799,-6.92514766987085));
#41519=CARTESIAN_POINT('Ctrl Pts',(-84.4456091242173,5.12176143341354,-5.09765870604247));
#41520=CARTESIAN_POINT('Ctrl Pts',(-84.3465213390008,6.93480746310232,-2.0315043474144));
#41521=CARTESIAN_POINT('Ctrl Pts',(-84.2474335537839,7.06278461725108,1.52827939665304));
#41522=CARTESIAN_POINT('Ctrl Pts',(-84.1483457685673,5.47459609606395,4.71671093548111));
#41523=CARTESIAN_POINT('Ctrl Pts',(-84.0492579833507,2.5561512502798,6.75904248023308));
#41524=CARTESIAN_POINT('Ctrl Pts',(-83.9501701981339,-0.983405419582861,
7.15901377597882));
#41525=CARTESIAN_POINT('Ctrl Pts',(-83.8510824129173,-4.28400724125367,
5.81943695049585));
#41526=CARTESIAN_POINT('Ctrl Pts',(-83.7519946277006,-6.54365049222737,
3.06581191521701));
#41527=CARTESIAN_POINT('Ctrl Pts',(-83.652906842484,-7.21327097247888,-0.432765919991988));
#41528=CARTESIAN_POINT('Ctrl Pts',(-83.5538190572673,-6.13015953172498,
-3.82618721177028));
#41529=CARTESIAN_POINT('Ctrl Pts',(-83.4547312720506,-3.55749829683403,
-6.28989430212752));
#41530=CARTESIAN_POINT('Ctrl Pts',(-83.3556434868339,-0.120410805453714,
-7.22523810693066));
#41531=CARTESIAN_POINT('Ctrl Pts',(-83.2565557016174,3.34593496045394,-6.40494213122378));
#41532=CARTESIAN_POINT('Ctrl Pts',(-83.1574679164006,5.99926163513778,-4.02832772960159));
#41533=CARTESIAN_POINT('Ctrl Pts',(-83.058380131184,7.19484501825694,-0.67288158481008));
#41534=CARTESIAN_POINT('Ctrl Pts',(-82.9592923459673,6.64217374987331,2.84606611666121));
#41535=CARTESIAN_POINT('Ctrl Pts',(-82.8602045607506,4.4755398283902,5.67345641636614));
#41536=CARTESIAN_POINT('Ctrl Pts',(-82.7611167755339,1.22140738496329,7.12226989546663));
#41537=CARTESIAN_POINT('Ctrl Pts',(-82.6620289903173,-2.32951131817089,
6.84046354294992));
#41538=CARTESIAN_POINT('Ctrl Pts',(-82.5629412051006,-5.31438878103006,
4.89651267209378));
#41539=CARTESIAN_POINT('Ctrl Pts',(-82.463853419884,-7.00793823296552,1.76277230147661));
#41540=CARTESIAN_POINT('Ctrl Pts',(-82.3647656346673,-6.99864897438848,
-1.79929902940124));
#41541=CARTESIAN_POINT('Ctrl Pts',(-82.2656778494506,-5.28877817546381,
-4.92416387569006));
#41542=CARTESIAN_POINT('Ctrl Pts',(-82.1665900642339,-2.29380241283818,
-6.85252033596187));
#41543=CARTESIAN_POINT('Ctrl Pts',(-82.0675022790173,1.25853778608825,-7.11580263251456));
#41544=CARTESIAN_POINT('Ctrl Pts',(-81.9684144938005,4.50506951616823,-5.6500365590326));
#41545=CARTESIAN_POINT('Ctrl Pts',(-81.8693267085839,6.65692739059195,-2.81138438857082));
#41546=CARTESIAN_POINT('Ctrl Pts',(-81.7702389233673,7.19123766728605,0.710397970520364));
#41547=CARTESIAN_POINT('Ctrl Pts',(-81.6711511381505,5.97816983229143,4.0595627745108));
#41548=CARTESIAN_POINT('Ctrl Pts',(-81.5720633529339,3.31248374210761,6.42230612180593));
#41549=CARTESIAN_POINT('Ctrl Pts',(-81.4729755677172,-0.158093224178774,
7.22451181716674));
#41550=CARTESIAN_POINT('Ctrl Pts',(-81.3738877825005,-3.59025557363318,
6.27125421107364));
#41551=CARTESIAN_POINT('Ctrl Pts',(-81.2747999972839,-6.15003207033319,
3.79416262142076));
#41552=CARTESIAN_POINT('Ctrl Pts',(-81.1757122120672,-7.21543000202332,
0.395138393243329));
#41553=CARTESIAN_POINT('Ctrl Pts',(-81.0766244268506,-6.52757139634248,
-3.09989937410306));
#41554=CARTESIAN_POINT('Ctrl Pts',(-80.9775366416338,-4.25359703309988,
-5.84170152814375));
#41555=CARTESIAN_POINT('Ctrl Pts',(-80.8784488564172,-0.946053387980383,
-7.16404546684372));
#41556=CARTESIAN_POINT('Ctrl Pts',(-80.7793610712005,2.59136904284052,-6.74561864825762));
#41557=CARTESIAN_POINT('Ctrl Pts',(-80.6802732859838,5.49912217968629,-4.68809339889848));
#41558=CARTESIAN_POINT('Ctrl Pts',(-80.5811855007673,7.07065946957171,-1.49142184819354));
#41559=CARTESIAN_POINT('Ctrl Pts',(-80.4820977155504,6.92411759645864,2.06764599830945));
#41560=CARTESIAN_POINT('Ctrl Pts',(-80.383009930334,5.09510434768085,5.12430250377131));
#41561=CARTESIAN_POINT('Ctrl Pts',(-80.2839221451171,2.02804638034109,6.93581951488781));
#41562=CARTESIAN_POINT('Ctrl Pts',(-80.1848343599005,-1.53180073101746,
7.06202173491186));
#41563=CARTESIAN_POINT('Ctrl Pts',(-80.0857465746839,-4.71943999823467,
5.47224365018372));
#41564=CARTESIAN_POINT('Ctrl Pts',(-79.9866587894672,-6.76031614429142,
2.5527808549004));
#41565=CARTESIAN_POINT('Ctrl Pts',(-79.8875710042505,-7.15852255738009,
-0.986974801802736));
#41566=CARTESIAN_POINT('Ctrl Pts',(-79.7884832190338,-5.81730020903324,
-4.2869082964177));
#41567=CARTESIAN_POINT('Ctrl Pts',(-79.6893954338172,-3.06254885153835,
-6.54517830130352));
#41568=CARTESIAN_POINT('Ctrl Pts',(-79.5903076486005,0.436362423448914,
-7.21305429754379));
#41569=CARTESIAN_POINT('Ctrl Pts',(-79.4912198633838,3.82924325099778,-6.1282510219965));
#41570=CARTESIAN_POINT('Ctrl Pts',(-79.3921320781672,6.29166729896275,-3.55436169558977));
#41571=CARTESIAN_POINT('Ctrl Pts',(-79.2930442929505,7.22529724598348,-0.116808266388605));
#41572=CARTESIAN_POINT('Ctrl Pts',(-79.1939565077338,6.40327304246616,3.34912806675697));
#41573=CARTESIAN_POINT('Ctrl Pts',(-79.0948687225171,4.02533598009955,6.00126942498245));
#41574=CARTESIAN_POINT('Ctrl Pts',(-78.9957809373005,0.669294131151232,
7.19517962457642));
#41575=CARTESIAN_POINT('Ctrl Pts',(-78.8966931520838,-2.84937756945328,
6.64075386764256));
#41576=CARTESIAN_POINT('Ctrl Pts',(-78.7976053668671,-5.67568722792293,
4.47271047069959));
#41577=CARTESIAN_POINT('Ctrl Pts',(-78.6985175816505,-7.12287800731837,
1.21785604928229));
#41578=CARTESIAN_POINT('Ctrl Pts',(-78.5994297964338,-6.83930119175066,
-2.33292170302204));
#41579=CARTESIAN_POINT('Ctrl Pts',(-78.500342011217,-4.89386229421091,-5.31682953546696));
#41580=CARTESIAN_POINT('Ctrl Pts',(-78.4012542260005,-1.75927790459205,
-7.00881628510317));
#41581=CARTESIAN_POINT('Ctrl Pts',(-78.3021664407838,1.8027883518613,-6.99775096886895));
#41582=CARTESIAN_POINT('Ctrl Pts',(-78.2030786555671,4.92680026331916,-5.28632231605976));
#41583=CARTESIAN_POINT('Ctrl Pts',(-78.1039908703505,6.85366318052953,-2.29038544174708));
#41584=CARTESIAN_POINT('Ctrl Pts',(-78.0049030851337,7.11517423751361,1.26208558891056));
#41585=CARTESIAN_POINT('Ctrl Pts',(-77.9058152999171,5.64778961635293,4.50788608034069));
#41586=CARTESIAN_POINT('Ctrl Pts',(-77.8067275147004,2.80806487633721,6.65832832730517));
#41587=CARTESIAN_POINT('Ctrl Pts',(-77.7076397294838,-0.713983453598893,
7.19088256696632));
#41588=CARTESIAN_POINT('Ctrl Pts',(-77.6085519442671,-4.06254300223632,
5.97614497974186));
#41589=CARTESIAN_POINT('Ctrl Pts',(-77.5094641590504,-6.42395693723408,
3.30928115041248));
#41590=CARTESIAN_POINT('Ctrl Pts',(-77.4103763738338,-7.22443209341518,
-0.161695366495079));
#41591=CARTESIAN_POINT('Ctrl Pts',(-77.3112885886171,-6.26946331998695,
-3.59338199239259));
#41592=CARTESIAN_POINT('Ctrl Pts',(-77.2122008034004,-3.79109572646178,
-6.15192308605336));
#41593=CARTESIAN_POINT('Ctrl Pts',(-77.1131130181837,-0.391540710377681,
-7.21562612224539));
#41594=CARTESIAN_POINT('Ctrl Pts',(-77.014025232967,3.10315365428635,-6.52602496637903));
#41595=CARTESIAN_POINT('Ctrl Pts',(-76.9149374477504,5.84382165748359,-4.25068381551004));
#41596=CARTESIAN_POINT('Ctrl Pts',(-76.8158496625337,7.16451628122316,-0.942481257108831));
#41597=CARTESIAN_POINT('Ctrl Pts',(-76.7167618773171,6.74432574584776,2.59473210521012));
#41598=CARTESIAN_POINT('Ctrl Pts',(-76.6176740921004,4.68535093832905,5.50145899272296));
#41599=CARTESIAN_POINT('Ctrl Pts',(-76.5185863068837,1.487896212053,7.07140221781165));
#41600=CARTESIAN_POINT('Ctrl Pts',(-76.4194985216671,-2.07109812585812,
6.92308580164801));
#41601=CARTESIAN_POINT('Ctrl Pts',(-76.3204107364503,-5.12684230020594,
5.0925487226665));
#41602=CARTESIAN_POINT('Ctrl Pts',(-76.2213229512338,-6.93682984239387,
2.02458790907854));
#41603=CARTESIAN_POINT('Ctrl Pts',(-76.122235166017,-7.06125709692096,-1.53532168456533));
#41604=CARTESIAN_POINT('Ctrl Pts',(-76.0231473808003,-5.46988984387717,
-4.72216788771455));
#41605=CARTESIAN_POINT('Ctrl Pts',(-75.9240595955837,-2.54940982488769,
-6.76158812770189));
#41606=CARTESIAN_POINT('Ctrl Pts',(-75.824971810367,0.990543938655987,-7.15802955913882));
#41607=CARTESIAN_POINT('Ctrl Pts',(-75.7258840251504,4.28980828583576,-5.81516202136175));
#41608=CARTESIAN_POINT('Ctrl Pts',(-75.6267962399337,6.54670448321702,-3.05928502649549));
#41609=CARTESIAN_POINT('Ctrl Pts',(-75.527708454717,7.21283582940884,0.439958818424079));
#41610=CARTESIAN_POINT('Ctrl Pts',(-75.4286206695004,6.1263409887555,3.83229833825699));
#41611=CARTESIAN_POINT('Ctrl Pts',(-75.3295328842836,3.55122421071421,6.29343873165936));
#41612=CARTESIAN_POINT('Ctrl Pts',(-75.2304450990671,0.113205698284411,
7.2253545887928));
#41613=CARTESIAN_POINT('Ctrl Pts',(-75.1313573138503,-3.35232034045075,
6.40160236182422));
#41614=CARTESIAN_POINT('Ctrl Pts',(-75.0322695286337,-6.00327572288282,
4.02234322987969));
#41615=CARTESIAN_POINT('Ctrl Pts',(-74.9331817434169,-7.1955124421398,0.665706511102669));
#41616=CARTESIAN_POINT('Ctrl Pts',(-74.8340939582003,-6.63933233448859,
-2.85268831387646));
#41617=CARTESIAN_POINT('Ctrl Pts',(-74.7350061729836,-4.46988000107174,
-5.6779166284767));
#41618=CARTESIAN_POINT('Ctrl Pts',(-74.635918387767,-1.21430441083646,-7.12348434838852));
#41619=CARTESIAN_POINT('Ctrl Pts',(-74.5368306025503,2.33633150789764,-6.83813714026838));
#41620=CARTESIAN_POINT('Ctrl Pts',(-74.4377428173337,5.31926896811458,-4.89121069969046));
#41621=CARTESIAN_POINT('Ctrl Pts',(-74.3386550321169,7.00969259481552,-1.75578307034256));
#41622=CARTESIAN_POINT('Ctrl Pts',(-74.2395672469003,6.99685122367504,1.80627722613956));
#41623=CARTESIAN_POINT('Ctrl Pts',(-74.1404794616836,5.28386514245066,4.92943542612214));
#41624=CARTESIAN_POINT('Ctrl Pts',(-74.041391676467,2.28696790125519,6.85480432124371));
#41625=CARTESIAN_POINT('Ctrl Pts',(-73.9423038912502,-1.26563307797238,
7.11454407364629));
#41626=CARTESIAN_POINT('Ctrl Pts',(-73.8432161060337,-4.51070152383107,
5.64554126960569));
#41627=CARTESIAN_POINT('Ctrl Pts',(-73.7441283208169,-6.65972760872605,
2.80474466600528));
#41628=CARTESIAN_POINT('Ctrl Pts',(-73.6450405356003,-7.19052567895877,
-0.717568759177671));
#41629=CARTESIAN_POINT('Ctrl Pts',(-73.5459527503836,-5.97411864149405,
-4.0655222199942));
#41630=CARTESIAN_POINT('Ctrl Pts',(-73.446864965167,-3.30607773601422,-6.42560615563577));
#41631=CARTESIAN_POINT('Ctrl Pts',(-73.3477771799502,0.165297468613132,
-7.2243505736352));
#41632=CARTESIAN_POINT('Ctrl Pts',(-73.2486893947336,3.59650751781999,-6.26767087028167));
#41633=CARTESIAN_POINT('Ctrl Pts',(-73.1496016095169,6.15381257237603,-3.78802788901824));
#41634=CARTESIAN_POINT('Ctrl Pts',(-73.0505138243002,7.21582044862827,-0.387942930173093));
#41635=CARTESIAN_POINT('Ctrl Pts',(-72.9514260390835,6.52447691401449,3.10640716301083));
#41636=CARTESIAN_POINT('Ctrl Pts',(-72.8523382538669,4.24776954117984,5.84594033402139));
#41637=CARTESIAN_POINT('Ctrl Pts',(-72.7532504686502,0.938908891931892,
7.16498531446955));
#41638=CARTESIAN_POINT('Ctrl Pts',(-72.6541626834336,-2.59809452251698,
6.74303116676621));
#41639=CARTESIAN_POINT('Ctrl Pts',(-72.5550748982169,-5.50379443807064,
4.68260731295887));
#41640=CARTESIAN_POINT('Ctrl Pts',(-72.4559871130002,-7.07214320806714,
1.48437020601429));
#41641=CARTESIAN_POINT('Ctrl Pts',(-72.3568993277835,-6.9220522857251,-2.07454973852188));
#41642=CARTESIAN_POINT('Ctrl Pts',(-72.2578115425669,-5.08999183162014,
-5.12938082208305));
#41643=CARTESIAN_POINT('Ctrl Pts',(-72.1587237573501,-2.02112893449372,
-6.93783844537082));
#41644=CARTESIAN_POINT('Ctrl Pts',(-72.0596359721336,1.5388422564249,-7.06049070346774));
#41645=CARTESIAN_POINT('Ctrl Pts',(-71.9605481869168,4.72489460324093,-5.46753467772979));
#41646=CARTESIAN_POINT('Ctrl Pts',(-71.8614604017002,6.76285843014922,-2.54603816107944));
#41647=CARTESIAN_POINT('Ctrl Pts',(-71.7623726164835,7.15753478137712,0.994112829255322));
#41648=CARTESIAN_POINT('Ctrl Pts',(-71.6632848312669,5.81302238801313,4.29270720878692));
#41649=CARTESIAN_POINT('Ctrl Pts',(-71.5641970460502,3.05602044089978,6.5482290375884));
#41650=CARTESIAN_POINT('Ctrl Pts',(-71.4651092608335,-0.443555104023324,
7.21261556812839));
#41651=CARTESIAN_POINT('Ctrl Pts',(-71.3660214756168,-3.83535247278855,
6.12442943247679));
#41652=CARTESIAN_POINT('Ctrl Pts',(-71.2669336904002,-6.29520859977706,
3.5480858429872));
#41653=CARTESIAN_POINT('Ctrl Pts',(-71.1678459051835,-7.22541013534436,
0.109603102036615));
#41654=CARTESIAN_POINT('Ctrl Pts',(-71.0687581199668,-6.39993008971324,
-3.35551178074168));
#41655=CARTESIAN_POINT('Ctrl Pts',(-70.9696703347502,-4.01934947968604,
-6.0052805283401));
#41656=CARTESIAN_POINT('Ctrl Pts',(-70.8705825495335,-0.662118725556255,
-7.19584347086433));
#41657=CARTESIAN_POINT('Ctrl Pts',(-70.7714947643167,2.85599834910767,-6.63790915076483));
#41658=CARTESIAN_POINT('Ctrl Pts',(-70.6724069791002,5.68014461747322,-4.46704842021029));
#41659=CARTESIAN_POINT('Ctrl Pts',(-70.5733191938834,7.12408891852638,-1.21075247050868));
#41660=CARTESIAN_POINT('Ctrl Pts',(-70.4742314086668,6.83697138879244,2.33974073195018));
#41661=CARTESIAN_POINT('Ctrl Pts',(-70.3751436234501,4.88855788919152,5.32170707836653));
#41662=CARTESIAN_POINT('Ctrl Pts',(-70.2760558382335,1.75228779959694,7.01056716188476));
#41663=CARTESIAN_POINT('Ctrl Pts',(-70.1769680530168,-1.80976565136866,
6.99594973903039));
#41664=CARTESIAN_POINT('Ctrl Pts',(-70.0778802678002,-4.93206936344387,
5.28140665524739));
#41665=CARTESIAN_POINT('Ctrl Pts',(-69.9787924825834,-6.85594375782075,
2.2835497922121));
#41666=CARTESIAN_POINT('Ctrl Pts',(-69.8797046973668,-7.1139121410692,-1.26918025239179));
#41667=CARTESIAN_POINT('Ctrl Pts',(-69.7806169121502,-5.64329151934991,
-4.51351584593945));
#41668=CARTESIAN_POINT('Ctrl Pts',(-69.6815291269334,-2.80142375840029,
-6.66112523450688));
#41669=CARTESIAN_POINT('Ctrl Pts',(-69.5824413417168,0.721153886365357,
-7.19016700335191));
#41670=CARTESIAN_POINT('Ctrl Pts',(-69.4833535565001,4.06850042704398,-5.97209081805211));
#41671=CARTESIAN_POINT('Ctrl Pts',(-69.3842657712834,6.42725377660052,-3.3028734997085));
#41672=CARTESIAN_POINT('Ctrl Pts',(-69.2851779860668,7.22426725784799,0.168899529635844));
#41673=CARTESIAN_POINT('Ctrl Pts',(-69.1860902008501,6.26587686240158,3.59963214914153));
#41674=CARTESIAN_POINT('Ctrl Pts',(-69.0870024156334,3.78495910985655,6.15570052882507));
#41675=CARTESIAN_POINT('Ctrl Pts',(-68.9879146304168,0.384345053516504,
7.21601298113648));
#41676=CARTESIAN_POINT('Ctrl Pts',(-68.8888268452,-3.10965989945231,6.52292723960769));
#41677=CARTESIAN_POINT('Ctrl Pts',(-68.7897390599835,-5.84805755726145,
4.24485421088667));
#41678=CARTESIAN_POINT('Ctrl Pts',(-68.6906512747667,-7.16545256640336,
0.935336293230516));
#41679=CARTESIAN_POINT('Ctrl Pts',(-68.5915634895501,-6.74173491146246,
-2.60145629370749));
#41680=CARTESIAN_POINT('Ctrl Pts',(-68.4924757043334,-4.6798625232114,-5.50612851558968));
#41681=CARTESIAN_POINT('Ctrl Pts',(-68.3933879191167,-1.48084383147897,
-7.0728824392594));
#41682=CARTESIAN_POINT('Ctrl Pts',(-68.2943001339001,2.07800083650708,-6.92101705076112));
#41683=CARTESIAN_POINT('Ctrl Pts',(-68.1952123486835,5.13191806661274,-5.08743367149795));
#41684=CARTESIAN_POINT('Ctrl Pts',(-68.0961245634667,6.9388453279461,-2.01766946490889));
#41685=CARTESIAN_POINT('Ctrl Pts',(-67.9970367782501,7.0597225458634,1.54236246085508));
#41686=CARTESIAN_POINT('Ctrl Pts',(-67.8979489930334,5.46517817033512,4.72762011344252));
#41687=CARTESIAN_POINT('Ctrl Pts',(-67.7988612078167,2.54266582779222,6.76412711356621));
#41688=CARTESIAN_POINT('Ctrl Pts',(-67.6997734226,-0.997681398644423,7.15703809797258));
#41689=CARTESIAN_POINT('Ctrl Pts',(-67.6006856373834,-4.29560521476863,
5.8108815655554));
#41690=CARTESIAN_POINT('Ctrl Pts',(-67.5015978521667,-6.54975165938407,
3.0527545763004));
#41691=CARTESIAN_POINT('Ctrl Pts',(-67.4025100669501,-7.21239413162189,
-0.447150226246016));
#41692=CARTESIAN_POINT('Ctrl Pts',(-67.3034222817333,-6.12251510055504,
-3.83840778962029));
#41693=CARTESIAN_POINT('Ctrl Pts',(-67.2043344965167,-3.54494913454001,
-6.29697257132185));
#41694=CARTESIAN_POINT('Ctrl Pts',(-67.1052467113,-0.105995324468443,-7.22547267039505));
#41695=CARTESIAN_POINT('Ctrl Pts',(-67.0061589260834,3.3586919338921,-6.39823840999051));
#41696=CARTESIAN_POINT('Ctrl Pts',(-66.9070711408666,6.00730504114269,-4.01639086919487));
#41697=CARTESIAN_POINT('Ctrl Pts',(-66.8079833556501,7.19612970031069,-0.658457417060504));
#41698=CARTESIAN_POINT('Ctrl Pts',(-66.7088955704333,6.63657172317509,2.85915744447726));
#41699=CARTESIAN_POINT('Ctrl Pts',(-66.6098077852167,4.4640346981544,5.68268549543904));
#41700=CARTESIAN_POINT('Ctrl Pts',(-66.5437492617389,2.29307521661488,6.64328120120947));
#41701=CARTESIAN_POINT('Ctrl Pts',(-66.51072,1.15821195975198,6.83557123116185));
#41702=CARTESIAN_POINT('Ctrl Pts',(-86.7854425030894,5.25436621795317,-4.14918985922678));
#41703=CARTESIAN_POINT('Ctrl Pts',(-86.7524132413505,5.94322790306273,-3.27684328317578));
#41704=CARTESIAN_POINT('Ctrl Pts',(-86.6863547178727,6.87734287666661,-1.18326448728897));
#41705=CARTESIAN_POINT('Ctrl Pts',(-86.587266932656,6.60680863506729,2.24644084517556));
#41706=CARTESIAN_POINT('Ctrl Pts',(-86.4881791474394,4.73105613954207,5.12957858913082));
#41707=CARTESIAN_POINT('Ctrl Pts',(-86.3890913622228,1.70564589191955,6.76663996306412));
#41708=CARTESIAN_POINT('Ctrl Pts',(-86.290003577006,-1.73417923433066,6.75932543582087));
#41709=CARTESIAN_POINT('Ctrl Pts',(-86.1909157917894,-4.75263843583045,
5.1096654801145));
#41710=CARTESIAN_POINT('Ctrl Pts',(-86.0918280065727,-6.6162592005329,2.2183814317692));
#41711=CARTESIAN_POINT('Ctrl Pts',(-85.992740221356,-6.87221841617152,-1.21192040828883));
#41712=CARTESIAN_POINT('Ctrl Pts',(-85.8936524361393,-5.45831501626719,
-4.34775121997823));
#41713=CARTESIAN_POINT('Ctrl Pts',(-85.7945646509228,-2.71811240611401,
-6.42712955557415));
#41714=CARTESIAN_POINT('Ctrl Pts',(-85.6954768657059,0.682557006289124,
-6.94480064264385));
#41715=CARTESIAN_POINT('Ctrl Pts',(-85.5963890804895,3.91737361083659,-5.77497343930147));
#41716=CARTESIAN_POINT('Ctrl Pts',(-85.4973012952726,6.20031901618341,-3.20190267875179));
#41717=CARTESIAN_POINT('Ctrl Pts',(-85.3982135100561,6.97666671611046,0.149189476057238));
#41718=CARTESIAN_POINT('Ctrl Pts',(-85.2991257248392,6.05777431104196,3.4640303661532));
#41719=CARTESIAN_POINT('Ctrl Pts',(-85.2000379396228,3.66692077327355,5.93715657379921));
#41720=CARTESIAN_POINT('Ctrl Pts',(-85.1009501544059,0.385052734120952,
6.96763018471131));
#41721=CARTESIAN_POINT('Ctrl Pts',(-85.0018623691894,-2.99037816253259,
6.30505943882551));
#41722=CARTESIAN_POINT('Ctrl Pts',(-84.9027745839727,-5.63918568761968,
4.11044046602357));
#41723=CARTESIAN_POINT('Ctrl Pts',(-84.8036867987559,-6.91774373856132,
0.917037417119129));
#41724=CARTESIAN_POINT('Ctrl Pts',(-84.7045990135394,-6.51537917876785,
-2.49919391243608));
#41725=CARTESIAN_POINT('Ctrl Pts',(-84.6055112283226,-4.52986141342742,
-5.30815331623375));
#41726=CARTESIAN_POINT('Ctrl Pts',(-84.506423443106,-1.44364568067551,-6.82729984722759));
#41727=CARTESIAN_POINT('Ctrl Pts',(-84.4073356578893,1.993357354595,-6.68750046811258));
#41728=CARTESIAN_POINT('Ctrl Pts',(-84.3082478726727,4.94600023224528,-4.92272462741185));
#41729=CARTESIAN_POINT('Ctrl Pts',(-84.209160087456,6.69682877053108,-1.96179011942424));
#41730=CARTESIAN_POINT('Ctrl Pts',(-84.1100723022392,6.82041418979961,1.47583411469907));
#41731=CARTESIAN_POINT('Ctrl Pts',(-84.0109845170227,5.28672682525449,4.55484967146845));
#41732=CARTESIAN_POINT('Ctrl Pts',(-83.9118967318059,2.46843294868416,6.52709543613163));
#41733=CARTESIAN_POINT('Ctrl Pts',(-83.8128089465894,-0.949658334712104,
6.91334109543625));
#41734=CARTESIAN_POINT('Ctrl Pts',(-83.7137211613725,-4.13699487679171,
5.61973392999406));
#41735=CARTESIAN_POINT('Ctrl Pts',(-83.614633376156,-6.31909495884465,2.96060381605423));
#41736=CARTESIAN_POINT('Ctrl Pts',(-83.5155455909392,-6.96573637194007,
-0.417914885067527));
#41737=CARTESIAN_POINT('Ctrl Pts',(-83.4164578057226,-5.91979358308471,
-3.69488565292608));
#41738=CARTESIAN_POINT('Ctrl Pts',(-83.3173700205059,-3.43541721556255,
-6.07404680666412));
#41739=CARTESIAN_POINT('Ctrl Pts',(-83.2182822352893,-0.11627872158463,
-6.97729283558003));
#41740=CARTESIAN_POINT('Ctrl Pts',(-83.1191944500726,3.23111400377219,-6.18514659075735));
#41741=CARTESIAN_POINT('Ctrl Pts',(-83.0201066648558,5.79338765119243,-3.89008940482619));
#41742=CARTESIAN_POINT('Ctrl Pts',(-82.9210188796393,6.9479427329653,-0.649790607784323));
#41743=CARTESIAN_POINT('Ctrl Pts',(-82.8219310944226,6.41423723783079,2.74839893599067));
#41744=CARTESIAN_POINT('Ctrl Pts',(-82.7228433092059,4.32195472562018,5.47876294470015));
#41745=CARTESIAN_POINT('Ctrl Pts',(-82.6237555239893,1.17949289287146,6.87785813827209));
#41746=CARTESIAN_POINT('Ctrl Pts',(-82.5246677387725,-2.24957051797165,
6.60572240857901));
#41747=CARTESIAN_POINT('Ctrl Pts',(-82.425579953556,-5.132017273147,4.72848123213478));
#41748=CARTESIAN_POINT('Ctrl Pts',(-82.3264921683392,-6.76744994440458,
1.70228003116653));
#41749=CARTESIAN_POINT('Ctrl Pts',(-82.2274043831225,-6.75847946116814,
-1.7375532876716));
#41750=CARTESIAN_POINT('Ctrl Pts',(-82.1283165979059,-5.10728553530141,
-4.75518354171855));
#41751=CARTESIAN_POINT('Ctrl Pts',(-82.0292288126892,-2.21508701920563,
-6.61736545400635));
#41752=CARTESIAN_POINT('Ctrl Pts',(-81.9301410274726,1.21534910659308,-6.87161280949628));
#41753=CARTESIAN_POINT('Ctrl Pts',(-81.8310532422559,4.35047105628243,-5.45614677615795));
#41754=CARTESIAN_POINT('Ctrl Pts',(-81.7319654570392,6.42848458444576,-2.71490736528399));
#41755=CARTESIAN_POINT('Ctrl Pts',(-81.6328776718226,6.94445917384764,0.68601956043053));
#41756=CARTESIAN_POINT('Ctrl Pts',(-81.5337898866059,5.77301964633066,3.92025257064009));
#41757=CARTESIAN_POINT('Ctrl Pts',(-81.4347021013892,3.19881071595589,6.20191470902461));
#41758=CARTESIAN_POINT('Ctrl Pts',(-81.3356143161725,-0.152668009564746,
6.97659146957779));
#41759=CARTESIAN_POINT('Ctrl Pts',(-81.2365265309558,-3.46705037551403,
6.05604637929548));
#41760=CARTESIAN_POINT('Ctrl Pts',(-81.1374387457392,-5.93898416465503,
3.66396003615034));
#41761=CARTESIAN_POINT('Ctrl Pts',(-81.0383509605224,-6.96782131103125,
0.38157860536036));
#41762=CARTESIAN_POINT('Ctrl Pts',(-80.9392631753059,-6.30356764211681,
-2.99352151082763));
#41763=CARTESIAN_POINT('Ctrl Pts',(-80.8401753900891,-4.10762824217843,
-5.64123446406796));
#41764=CARTESIAN_POINT('Ctrl Pts',(-80.7410876048726,-0.913588096107144,
-6.91820011601149));
#41765=CARTESIAN_POINT('Ctrl Pts',(-80.6419998196559,2.502442187976,-6.51413226380673));
#41766=CARTESIAN_POINT('Ctrl Pts',(-80.5429120344391,5.31041125821166,-4.52721419011613));
#41767=CARTESIAN_POINT('Ctrl Pts',(-80.4438242492226,6.82801880432787,-1.44024139027976));
#41768=CARTESIAN_POINT('Ctrl Pts',(-80.3447364640057,6.6865057432699,1.99669151341629));
#41769=CARTESIAN_POINT('Ctrl Pts',(-80.2456486787892,4.92025792582607,4.94845410182571));
#41770=CARTESIAN_POINT('Ctrl Pts',(-80.1465608935724,1.95845081786362,6.69780609218714));
#41771=CARTESIAN_POINT('Ctrl Pts',(-80.0474731083559,-1.47923460900375,
6.81967748695314));
#41772=CARTESIAN_POINT('Ctrl Pts',(-79.9483853231391,-4.55748508219353,
5.28445510720959));
#41773=CARTESIAN_POINT('Ctrl Pts',(-79.8492975379226,-6.52832539242893,
2.46517821365873));
#41774=CARTESIAN_POINT('Ctrl Pts',(-79.7502097527057,-6.91286673376692,
-0.953105228035428));
#41775=CARTESIAN_POINT('Ctrl Pts',(-79.6511219674892,-5.61767051413456,
-4.13979637774047));
#41776=CARTESIAN_POINT('Ctrl Pts',(-79.5520341822724,-2.95745272947546,
-6.32057033877863));
#41777=CARTESIAN_POINT('Ctrl Pts',(-79.4529463970558,0.421387968920513,
-6.96552713254201));
#41778=CARTESIAN_POINT('Ctrl Pts',(-79.3538586118391,3.69783681941937,-5.91795056683278));
#41779=CARTESIAN_POINT('Ctrl Pts',(-79.2547708266225,6.07575896035828,-3.43238825166325));
#41780=CARTESIAN_POINT('Ctrl Pts',(-79.1556830414058,6.97734994518436,-0.112799809244738));
#41781=CARTESIAN_POINT('Ctrl Pts',(-79.0565952561891,6.18353477937369,3.23419753367137));
#41782=CARTESIAN_POINT('Ctrl Pts',(-78.9575074709724,3.88720032185653,5.79532654060911));
#41783=CARTESIAN_POINT('Ctrl Pts',(-78.8584196857559,0.646326263171543,
6.94826585674906));
#41784=CARTESIAN_POINT('Ctrl Pts',(-78.759331900539,-2.75159675113525,6.41286608106483));
#41785=CARTESIAN_POINT('Ctrl Pts',(-78.6602441153225,-5.48091720249239,
4.31922246173463));
#41786=CARTESIAN_POINT('Ctrl Pts',(-78.5611563301058,-6.87844538182083,
1.17606342679199));
#41787=CARTESIAN_POINT('Ctrl Pts',(-78.4620685448891,-6.60459994526706,
-2.25286387016798));
#41788=CARTESIAN_POINT('Ctrl Pts',(-78.3629807596724,-4.7259218060868,-5.13437426930324));
#41789=CARTESIAN_POINT('Ctrl Pts',(-78.2638929744557,-1.69890554994023,
-6.76829786481892));
#41790=CARTESIAN_POINT('Ctrl Pts',(-78.1648051892391,1.74092286861015,-6.75761227210323));
#41791=CARTESIAN_POINT('Ctrl Pts',(-78.0657174040224,4.75772945761006,-5.10491395252843));
#41792=CARTESIAN_POINT('Ctrl Pts',(-77.9666296188058,6.61846908008706,-2.2117873067864));
#41793=CARTESIAN_POINT('Ctrl Pts',(-77.867541833589,6.87100597884612,1.2187751610494));
#41794=CARTESIAN_POINT('Ctrl Pts',(-77.7684540483724,5.45397694080736,4.35319096567927));
#41795=CARTESIAN_POINT('Ctrl Pts',(-77.6693662631557,2.71170176727014,6.42983744583905));
#41796=CARTESIAN_POINT('Ctrl Pts',(-77.5702784779391,-0.689482002086527,
6.94411625934709));
#41797=CARTESIAN_POINT('Ctrl Pts',(-77.4711906927224,-3.9231305272209,5.77106427974229));
#41798=CARTESIAN_POINT('Ctrl Pts',(-77.3721029075058,-6.2035088741565,3.19571802617058));
#41799=CARTESIAN_POINT('Ctrl Pts',(-77.273015122289,-6.97651448167062,-0.15614653877089));
#41800=CARTESIAN_POINT('Ctrl Pts',(-77.1739273370724,-6.0543169454189,-3.47006950635624));
#41801=CARTESIAN_POINT('Ctrl Pts',(-77.0748395518556,-3.66099838645685,
-5.94081028723273));
#41802=CARTESIAN_POINT('Ctrl Pts',(-76.975751766639,-0.3781043825719,-6.96801070108319));
#41803=CARTESIAN_POINT('Ctrl Pts',(-76.8766639814224,2.99666411533033,-6.30207428030022));
#41804=CARTESIAN_POINT('Ctrl Pts',(-76.7775761962057,5.64328183787549,-4.10481499617639));
#41805=CARTESIAN_POINT('Ctrl Pts',(-76.678488410989,6.918654773664,-0.910138548456401));
#41806=CARTESIAN_POINT('Ctrl Pts',(-76.5794006257724,6.51288372935182,2.50568984163527));
#41807=CARTESIAN_POINT('Ctrl Pts',(-76.4803128405557,4.52456584134205,5.31266787987831));
#41808=CARTESIAN_POINT('Ctrl Pts',(-76.381225055339,1.4368367418211,6.82873606400796));
#41809=CARTESIAN_POINT('Ctrl Pts',(-76.2821372701224,-2.00002517584462,
6.68550935610128));
#41810=CARTESIAN_POINT('Ctrl Pts',(-76.1830494849056,-4.95090674119966,
4.91779000105471));
#41811=CARTESIAN_POINT('Ctrl Pts',(-76.083961699689,-6.6987817487351,1.9551110294158));
#41812=CARTESIAN_POINT('Ctrl Pts',(-75.9848739144723,-6.81893908870291,
-1.48263473556018));
#41813=CARTESIAN_POINT('Ctrl Pts',(-75.8857861292556,-5.2821820754235,-4.56011935990765));
#41814=CARTESIAN_POINT('Ctrl Pts',(-75.786698344039,-2.46192286577841,-6.52955372575242));
#41815=CARTESIAN_POINT('Ctrl Pts',(-75.6876105588223,0.956551884412262,
-6.91239065352628));
#41816=CARTESIAN_POINT('Ctrl Pts',(-75.5885227736057,4.14259684951599,-5.61560570169507));
#41817=CARTESIAN_POINT('Ctrl Pts',(-75.489434988389,6.32204414738856,-2.95430090765989));
#41818=CARTESIAN_POINT('Ctrl Pts',(-75.3903472031723,6.96531616148055,0.424860948014456));
#41819=CARTESIAN_POINT('Ctrl Pts',(-75.2912594179557,5.91610607935003,3.70078706661266));
#41820=CARTESIAN_POINT('Ctrl Pts',(-75.1921716327389,3.42935843445585,6.07746960358966));
#41821=CARTESIAN_POINT('Ctrl Pts',(-75.0930838475223,0.10932086886228,6.9774053201861));
#41822=CARTESIAN_POINT('Ctrl Pts',(-74.9939960623056,-3.23728025953358,
6.18192143073367));
#41823=CARTESIAN_POINT('Ctrl Pts',(-74.894908277089,-5.79726398927988,3.88431027251025));
#41824=CARTESIAN_POINT('Ctrl Pts',(-74.7958204918722,-6.94858725316066,
0.642861757878953));
#41825=CARTESIAN_POINT('Ctrl Pts',(-74.6967327066556,-6.41149333002965,
-2.7547938822197));
#41826=CARTESIAN_POINT('Ctrl Pts',(-74.597644921439,-4.3164891240697,-5.48307009770239));
#41827=CARTESIAN_POINT('Ctrl Pts',(-74.4985571362222,-1.17263366833754,
-6.87903091535509));
#41828=CARTESIAN_POINT('Ctrl Pts',(-74.3994693510056,2.25615666229153,-6.60347584001997));
#41829=CARTESIAN_POINT('Ctrl Pts',(-74.3003815657889,5.13672998902946,-4.72336120515205));
#41830=CARTESIAN_POINT('Ctrl Pts',(-74.2012937805723,6.76914410260199,-1.69553064635787));
#41831=CARTESIAN_POINT('Ctrl Pts',(-74.1022059953556,6.75674340306355,1.74429201674696));
#41832=CARTESIAN_POINT('Ctrl Pts',(-74.0031182101389,5.1025411006494,4.76027419070725));
#41833=CARTESIAN_POINT('Ctrl Pts',(-73.9040304249223,2.20848704450624,6.61957106078467));
#41834=CARTESIAN_POINT('Ctrl Pts',(-73.8049426397056,-1.22220091251239,
6.87039744003096));
#41835=CARTESIAN_POINT('Ctrl Pts',(-73.7058548544889,-4.35590979285198,
5.45180574957198));
#41836=CARTESIAN_POINT('Ctrl Pts',(-73.6067670692723,-6.43118870874393,
2.70849549511429));
#41837=CARTESIAN_POINT('Ctrl Pts',(-73.5076792840555,-6.94377161850602,
-0.692944272333947));
#41838=CARTESIAN_POINT('Ctrl Pts',(-73.408591498839,-5.76910747843973,-3.92600750849266));
#41839=CARTESIAN_POINT('Ctrl Pts',(-73.3095037136222,-3.19262454191448,
-6.20510149706638));
#41840=CARTESIAN_POINT('Ctrl Pts',(-73.2104159284056,0.159625029158248,
-6.97643575936854));
#41841=CARTESIAN_POINT('Ctrl Pts',(-73.1113281431889,3.47308777452254,-6.05258600641015));
#41842=CARTESIAN_POINT('Ctrl Pts',(-73.0122403579722,5.94263493289657,-3.65803582662163));
#41843=CARTESIAN_POINT('Ctrl Pts',(-72.9131525727555,6.96819835885431,-0.374630065784826));
#41844=CARTESIAN_POINT('Ctrl Pts',(-72.8140647875388,6.30057935175775,2.99980597484801));
#41845=CARTESIAN_POINT('Ctrl Pts',(-72.7149770023223,4.10200072969768,5.64532780873616));
#41846=CARTESIAN_POINT('Ctrl Pts',(-72.6158892171055,0.906688774540824,
6.91910771130582));
#41847=CARTESIAN_POINT('Ctrl Pts',(-72.5168014318889,-2.50893687236812,
6.51163357576282));
#41848=CARTESIAN_POINT('Ctrl Pts',(-72.4177136466722,-5.31492318079035,
4.52191636773916));
#41849=CARTESIAN_POINT('Ctrl Pts',(-72.3186258614555,-6.82945162603157,
1.4334317361579));
#41850=CARTESIAN_POINT('Ctrl Pts',(-72.2195380762388,-6.68451130688302,
-2.00335834105711));
#41851=CARTESIAN_POINT('Ctrl Pts',(-72.1204502910222,-4.9153208536972,-4.9533581497545));
#41852=CARTESIAN_POINT('Ctrl Pts',(-72.0213625058055,-1.95177075491801,
-6.69975573993386));
#41853=CARTESIAN_POINT('Ctrl Pts',(-71.9222747205888,1.48603449352654,-6.81819899523176));
#41854=CARTESIAN_POINT('Ctrl Pts',(-71.8231869353722,4.56275250395429,-5.27990773046166));
#41855=CARTESIAN_POINT('Ctrl Pts',(-71.7240991501555,6.53078043579762,-2.45866690585223));
#41856=CARTESIAN_POINT('Ctrl Pts',(-71.6250113649389,6.91191285483219,0.959998302985763));
#41857=CARTESIAN_POINT('Ctrl Pts',(-71.5259235797221,5.61353949318912,4.14539629142208));
#41858=CARTESIAN_POINT('Ctrl Pts',(-71.4268357945055,2.95114835139102,6.32351638430802));
#41859=CARTESIAN_POINT('Ctrl Pts',(-71.3277480092889,-0.428333821485886,
6.96510345880816));
#41860=CARTESIAN_POINT('Ctrl Pts',(-71.2286602240721,-3.70373639377261,
5.91426012109497));
#41861=CARTESIAN_POINT('Ctrl Pts',(-71.1295724388556,-6.0791787359331,3.42632776469341));
#41862=CARTESIAN_POINT('Ctrl Pts',(-71.0304846536388,-6.97745896057144,
0.105841901302007));
#41863=CARTESIAN_POINT('Ctrl Pts',(-70.9313968684222,-6.18030654523836,
-3.24036218059244));
#41864=CARTESIAN_POINT('Ctrl Pts',(-70.8323090832054,-3.88141925750582,
-5.79919999672307));
#41865=CARTESIAN_POINT('Ctrl Pts',(-70.7332212979888,-0.639397092767843,
-6.94890692212019));
#41866=CARTESIAN_POINT('Ctrl Pts',(-70.6341335127721,2.75799032844922,-6.41011898506654));
#41867=CARTESIAN_POINT('Ctrl Pts',(-70.5350457275555,5.4852216297949,-4.31375471330489));
#41868=CARTESIAN_POINT('Ctrl Pts',(-70.4359579423388,6.87961473872937,-1.16920361836068));
#41869=CARTESIAN_POINT('Ctrl Pts',(-70.3368701571221,6.60235009311713,2.25944889352386));
#41870=CARTESIAN_POINT('Ctrl Pts',(-70.2377823719054,4.720799429967,5.13908443174007));
#41871=CARTESIAN_POINT('Ctrl Pts',(-70.1386945866888,1.69215532125842,6.76998865754343));
#41872=CARTESIAN_POINT('Ctrl Pts',(-70.0396068014721,-1.74766073124442,
6.75587285426512));
#41873=CARTESIAN_POINT('Ctrl Pts',(-69.9405190162555,-4.76281774037749,
5.1001669802542));
#41874=CARTESIAN_POINT('Ctrl Pts',(-69.8414312310387,-6.62067139582524,
2.20518623318563));
#41875=CARTESIAN_POINT('Ctrl Pts',(-69.7423434458221,-6.86978719320209,
-1.22562636013042));
#41876=CARTESIAN_POINT('Ctrl Pts',(-69.6432556606054,-5.4496332029916,-4.35862753712465));
#41877=CARTESIAN_POINT('Ctrl Pts',(-69.5441678753888,-2.7052885496134,-6.43253837282463));
#41878=CARTESIAN_POINT('Ctrl Pts',(-69.4450800901721,0.696406370312047,
-6.94342525140987));
#41879=CARTESIAN_POINT('Ctrl Pts',(-69.3459923049554,3.92888351374035,-5.7671492429098));
#41880=CARTESIAN_POINT('Ctrl Pts',(-69.2469045197387,6.20669257735784,-3.18953026395594));
#41881=CARTESIAN_POINT('Ctrl Pts',(-69.1478167345221,6.97635530269203,0.163103479860511));
#41882=CARTESIAN_POINT('Ctrl Pts',(-69.0487289493054,6.05085356269778,3.47610517926561));
#41883=CARTESIAN_POINT('Ctrl Pts',(-68.9496411640888,3.65507235738477,5.94445810118679));
#41884=CARTESIAN_POINT('Ctrl Pts',(-68.850553378872,0.371155655855663,6.96838428431038));
#41885=CARTESIAN_POINT('Ctrl Pts',(-68.7514655936554,-3.00294708858478,
6.29908285683592));
#41886=CARTESIAN_POINT('Ctrl Pts',(-68.6523778084387,-5.64737237617125,
4.09918544349301));
#41887=CARTESIAN_POINT('Ctrl Pts',(-68.5532900232221,-6.91955892876356,
0.903238775114562));
#41888=CARTESIAN_POINT('Ctrl Pts',(-68.4542022380054,-6.51038180347379,
-2.51218327915711));
#41889=CARTESIAN_POINT('Ctrl Pts',(-68.3551144527887,-4.5192657697164,-5.31717716081293));
#41890=CARTESIAN_POINT('Ctrl Pts',(-68.2560266675721,-1.43002637464361,
-6.83016548935693));
#41891=CARTESIAN_POINT('Ctrl Pts',(-68.1569388823553,2.00669100925305,-6.68351159761526));
#41892=CARTESIAN_POINT('Ctrl Pts',(-68.0578510971388,4.95580832479609,-4.91285048081417));
#41893=CARTESIAN_POINT('Ctrl Pts',(-67.958763311922,6.70072806976919,-1.94843000240689));
#41894=CARTESIAN_POINT('Ctrl Pts',(-67.8596755267054,6.81745719814908,1.48943389667244));
#41895=CARTESIAN_POINT('Ctrl Pts',(-67.7605877414887,5.27763209027949,4.56538448403874));
#41896=CARTESIAN_POINT('Ctrl Pts',(-67.661499956272,2.45541029942128,6.53200558237203));
#41897=CARTESIAN_POINT('Ctrl Pts',(-67.5624121710554,-0.963444411371859,
6.91143321589037));
#41898=CARTESIAN_POINT('Ctrl Pts',(-67.4633243858387,-4.14819484782596,
5.61147213638018));
#41899=CARTESIAN_POINT('Ctrl Pts',(-67.364236600622,-6.3249867549711,2.94799456000949));
#41900=CARTESIAN_POINT('Ctrl Pts',(-67.2651488154053,-6.96488962123942,
-0.43180557150384));
#41901=CARTESIAN_POINT('Ctrl Pts',(-67.1660610301887,-5.91241148244737,
-3.70668686266028));
#41902=CARTESIAN_POINT('Ctrl Pts',(-67.0669732449719,-3.42329869727003,
-6.08088217405369));
#41903=CARTESIAN_POINT('Ctrl Pts',(-66.9678854597554,-0.102357930226421,
-6.97751934963469));
#41904=CARTESIAN_POINT('Ctrl Pts',(-66.8687976745387,3.24343320184657,-6.17867291813365));
#41905=CARTESIAN_POINT('Ctrl Pts',(-66.769709889322,5.8011550352234,-3.87856217633039));
#41906=CARTESIAN_POINT('Ctrl Pts',(-66.6706221041053,6.94918332915839,-0.635861427761624));
#41907=CARTESIAN_POINT('Ctrl Pts',(-66.5715343188886,6.40882745338248,2.76104101455297));
#41908=CARTESIAN_POINT('Ctrl Pts',(-66.472446533672,4.31084441180371,5.48767531358562));
#41909=CARTESIAN_POINT('Ctrl Pts',(-66.4063880101942,2.21438477785055,6.41530668525375));
#41910=CARTESIAN_POINT('Ctrl Pts',(-66.3733587484553,1.11846611686177,6.60099798407104));
#41911=CARTESIAN_POINT('Ctrl Pts',(-86.6480812515447,5.0676469145806,-4.00174413353138));
#41912=CARTESIAN_POINT('Ctrl Pts',(-86.6150519898058,5.73202919177904,-3.16039728955523));
#41913=CARTESIAN_POINT('Ctrl Pts',(-86.548993466328,6.63294942982275,-1.14121596771352));
#41914=CARTESIAN_POINT('Ctrl Pts',(-86.4499056811114,6.37202890052182,2.16661126111543));
#41915=CARTESIAN_POINT('Ctrl Pts',(-86.3508178958946,4.56293319760216,4.94729374239046));
#41916=CARTESIAN_POINT('Ctrl Pts',(-86.2517301106781,1.64503401228858,6.52618045802251));
#41917=CARTESIAN_POINT('Ctrl Pts',(-86.1526423254613,-1.67255339305395,
6.51912586002186));
#41918=CARTESIAN_POINT('Ctrl Pts',(-86.0535545402447,-4.58374854481224,
4.92808826616734));
#41919=CARTESIAN_POINT('Ctrl Pts',(-85.954466755028,-6.38114363043145,2.13954896780058));
#41920=CARTESIAN_POINT('Ctrl Pts',(-85.8553789698114,-6.62800707229765,
-1.16885357111151));
#41921=CARTESIAN_POINT('Ctrl Pts',(-85.7562911845946,-5.264348182752,-4.19324941227064));
#41922=CARTESIAN_POINT('Ctrl Pts',(-85.657203399378,-2.62152148840752,-6.19873490177144));
#41923=CARTESIAN_POINT('Ctrl Pts',(-85.5581156141612,0.658301641619111,
-6.69801001476086));
#41924=CARTESIAN_POINT('Ctrl Pts',(-85.4590278289447,3.77816571376116,-5.56975382329959));
#41925=CARTESIAN_POINT('Ctrl Pts',(-85.3599400437279,5.97998430798706,-3.08811977652457));
#41926=CARTESIAN_POINT('Ctrl Pts',(-85.2608522585114,6.72874369455863,0.14388787470623));
#41927=CARTESIAN_POINT('Ctrl Pts',(-85.1617644732945,5.84250507543342,3.34093248717029));
#41928=CARTESIAN_POINT('Ctrl Pts',(-85.0626766880781,3.53661297516676,5.7261736134403));
#41929=CARTESIAN_POINT('Ctrl Pts',(-84.9635889028612,0.371369489502175,
6.72002828558944));
#41930=CARTESIAN_POINT('Ctrl Pts',(-84.8645011176447,-2.88411200136919,
6.08100267207071));
#41931=CARTESIAN_POINT('Ctrl Pts',(-84.7654133324279,-5.43879142892048,
3.9643717398377));
#41932=CARTESIAN_POINT('Ctrl Pts',(-84.6663255472113,-6.67191460557079,
0.884449550078927));
#41933=CARTESIAN_POINT('Ctrl Pts',(-84.5672377619947,-6.28384848391239,
-2.41038248838107));
#41934=CARTESIAN_POINT('Ctrl Pts',(-84.4681499767779,-4.3688881328442,-5.11952263304775));
#41935=CARTESIAN_POINT('Ctrl Pts',(-84.3690621915613,-1.392344247804,-6.58468473086316));
#41936=CARTESIAN_POINT('Ctrl Pts',(-84.2699744063445,1.922521352462,-6.44985326635431));
#41937=CARTESIAN_POINT('Ctrl Pts',(-84.170886621128,4.77023903107702,-4.74779054878123));
#41938=CARTESIAN_POINT('Ctrl Pts',(-84.0717988359113,6.45885007795985,-1.89207589143408));
#41939=CARTESIAN_POINT('Ctrl Pts',(-83.9727110506945,6.57804376234814,1.4233888327451));
#41940=CARTESIAN_POINT('Ctrl Pts',(-83.873623265478,5.09885755444503,4.39298840745579));
#41941=CARTESIAN_POINT('Ctrl Pts',(-83.7745354802612,2.38071464708853,6.29514839203017));
#41942=CARTESIAN_POINT('Ctrl Pts',(-83.6754476950446,-0.915911249841352,
6.66766841489367));
#41943=CARTESIAN_POINT('Ctrl Pts',(-83.5763599098279,-3.98998251232974,
5.42003090949228));
#41944=CARTESIAN_POINT('Ctrl Pts',(-83.4772721246113,-6.09453942546194,
2.85539571689145));
#41945=CARTESIAN_POINT('Ctrl Pts',(-83.3781843393945,-6.71820177140126,
-0.403063850143066));
#41946=CARTESIAN_POINT('Ctrl Pts',(-83.2790965541779,-5.70942763444443,
-3.56358409408187));
#41947=CARTESIAN_POINT('Ctrl Pts',(-83.1800087689612,-3.31333613429106,
-5.85819931120072));
#41948=CARTESIAN_POINT('Ctrl Pts',(-83.0809209837446,-0.112146637715546,
-6.7293475642294));
#41949=CARTESIAN_POINT('Ctrl Pts',(-82.981833198528,3.11629304709045,-5.96535105029092));
#41950=CARTESIAN_POINT('Ctrl Pts',(-82.8827454133112,5.58751366724708,-3.75185108005079));
#41951=CARTESIAN_POINT('Ctrl Pts',(-82.7836576280946,6.70104044767366,-0.626699630758572));
#41952=CARTESIAN_POINT('Ctrl Pts',(-82.6845698428779,6.18630072578829,2.65073175532014));
#41953=CARTESIAN_POINT('Ctrl Pts',(-82.5854820576612,4.16836962285014,5.28406947303415));
#41954=CARTESIAN_POINT('Ctrl Pts',(-82.4863942724445,1.13757840077963,6.63344638107755));
#41955=CARTESIAN_POINT('Ctrl Pts',(-82.3873064872278,-2.16962971777241,
6.37098127420809));
#41956=CARTESIAN_POINT('Ctrl Pts',(-82.2882187020112,-4.94964576526393,
4.56044979217578));
#41957=CARTESIAN_POINT('Ctrl Pts',(-82.1891309167946,-6.52696165584364,
1.64178776085645));
#41958=CARTESIAN_POINT('Ctrl Pts',(-82.0900431315779,-6.5183099479478,-1.67580754594197));
#41959=CARTESIAN_POINT('Ctrl Pts',(-81.9909553463612,-4.92579289513902,
-4.58620320774704));
#41960=CARTESIAN_POINT('Ctrl Pts',(-81.8918675611445,-2.13637162557306,
-6.38221057205085));
#41961=CARTESIAN_POINT('Ctrl Pts',(-81.7927797759279,1.17216042709791,-6.62742298647799));
#41962=CARTESIAN_POINT('Ctrl Pts',(-81.6936919907112,4.19587259639663,-5.26225699328331));
#41963=CARTESIAN_POINT('Ctrl Pts',(-81.5946042054945,6.20004177829955,-2.61843034199716));
#41964=CARTESIAN_POINT('Ctrl Pts',(-81.4955164202779,6.69768068040923,0.661641150340698));
#41965=CARTESIAN_POINT('Ctrl Pts',(-81.3964286350611,5.56786946036987,3.7809423667694));
#41966=CARTESIAN_POINT('Ctrl Pts',(-81.2973408498445,3.08513768980417,5.98152329624329));
#41967=CARTESIAN_POINT('Ctrl Pts',(-81.1982530646279,-0.147242794950722,
6.72867112198883));
#41968=CARTESIAN_POINT('Ctrl Pts',(-81.0991652794111,-3.34384517739488,
5.84083854751732));
#41969=CARTESIAN_POINT('Ctrl Pts',(-81.0000774941945,-5.72793625897687,
3.53375745087992));
#41970=CARTESIAN_POINT('Ctrl Pts',(-80.9009897089778,-6.72021262003917,
0.368018817477388));
#41971=CARTESIAN_POINT('Ctrl Pts',(-80.8019019237612,-6.07956388789115,
-2.8871436475522));
#41972=CARTESIAN_POINT('Ctrl Pts',(-80.7028141385445,-3.96165945125696,
-5.44076739999217));
#41973=CARTESIAN_POINT('Ctrl Pts',(-80.6037263533278,-0.881122804233911,
-6.67235476517926));
#41974=CARTESIAN_POINT('Ctrl Pts',(-80.5046385681112,2.41351533311149,-6.28264587935584));
#41975=CARTESIAN_POINT('Ctrl Pts',(-80.4055507828944,5.12170033673702,-4.36633498133378));
#41976=CARTESIAN_POINT('Ctrl Pts',(-80.3064629976779,6.58537813908403,-1.38906093236599));
#41977=CARTESIAN_POINT('Ctrl Pts',(-80.2073752124611,6.44889389008117,1.92573702852313));
#41978=CARTESIAN_POINT('Ctrl Pts',(-80.1082874272445,4.7454115039713,4.77260569988011));
#41979=CARTESIAN_POINT('Ctrl Pts',(-80.0091996420278,1.88885525538614,6.45979266948648));
#41980=CARTESIAN_POINT('Ctrl Pts',(-79.9101118568112,-1.42666848699003,
6.57733323899442));
#41981=CARTESIAN_POINT('Ctrl Pts',(-79.8110240715944,-4.39553016615239,
5.09666656423546));
#41982=CARTESIAN_POINT('Ctrl Pts',(-79.7119362863778,-6.29633464056644,
2.37757557241705));
#41983=CARTESIAN_POINT('Ctrl Pts',(-79.612848501161,-6.66721091015377,-0.919235654268119));
#41984=CARTESIAN_POINT('Ctrl Pts',(-79.5137607159445,-5.41804081923588,
-3.99268445906324));
#41985=CARTESIAN_POINT('Ctrl Pts',(-79.4146729307277,-2.85235660741258,
-6.09596237625374));
#41986=CARTESIAN_POINT('Ctrl Pts',(-79.3155851455112,0.406413514392112,
-6.71799996754024));
#41987=CARTESIAN_POINT('Ctrl Pts',(-79.2164973602944,3.56643038784096,-5.70765011166905));
#41988=CARTESIAN_POINT('Ctrl Pts',(-79.1174095750778,5.85985062175381,-3.31041480773674));
#41989=CARTESIAN_POINT('Ctrl Pts',(-79.018321789861,6.72940264438526,-0.108791352100868));
#41990=CARTESIAN_POINT('Ctrl Pts',(-78.9192340046445,5.96379651628121,3.11926700058577));
#41991=CARTESIAN_POINT('Ctrl Pts',(-78.8201462194277,3.74906466361352,5.58938365623578));
#41992=CARTESIAN_POINT('Ctrl Pts',(-78.7210584342111,0.623358395191846,
6.7013520889217));
#41993=CARTESIAN_POINT('Ctrl Pts',(-78.6219706489944,-2.65381593281721,
6.18497829448711));
#41994=CARTESIAN_POINT('Ctrl Pts',(-78.5228828637778,-5.28614717706186,
4.16573445276967));
#41995=CARTESIAN_POINT('Ctrl Pts',(-78.423795078561,-6.63401275632328,1.1342708043017));
#41996=CARTESIAN_POINT('Ctrl Pts',(-78.3247072933444,-6.36989869878348,
-2.17280603731392));
#41997=CARTESIAN_POINT('Ctrl Pts',(-78.2256195081277,-4.55798131796269,
-4.95191900313952));
#41998=CARTESIAN_POINT('Ctrl Pts',(-78.126531722911,-1.63853319528842,-6.52777944453465));
#41999=CARTESIAN_POINT('Ctrl Pts',(-78.0274439376944,1.67905738535901,-6.51747357533751));
#42000=CARTESIAN_POINT('Ctrl Pts',(-77.9283561524777,4.58865865190096,-4.92350558899711));
#42001=CARTESIAN_POINT('Ctrl Pts',(-77.8292683672611,6.38327497964459,-2.1331891718257));
#42002=CARTESIAN_POINT('Ctrl Pts',(-77.7301805820443,6.62683772017861,1.17546473318823));
#42003=CARTESIAN_POINT('Ctrl Pts',(-77.6310927968278,5.26016426526179,4.19849585101786));
#42004=CARTESIAN_POINT('Ctrl Pts',(-77.532005011611,2.61533865820306,6.20134656437292));
#42005=CARTESIAN_POINT('Ctrl Pts',(-77.4329172263944,-0.664980550574156,
6.69734995172787));
#42006=CARTESIAN_POINT('Ctrl Pts',(-77.3338294411777,-3.78371805220548,
5.56598357974272));
#42007=CARTESIAN_POINT('Ctrl Pts',(-77.2347416559611,-5.98306081107892,
3.08215490192868));
#42008=CARTESIAN_POINT('Ctrl Pts',(-77.1356538707443,-6.72859686992606,
-0.150597711046703));
#42009=CARTESIAN_POINT('Ctrl Pts',(-77.0365660855277,-5.83917057085085,
-3.3467570203199));
#42010=CARTESIAN_POINT('Ctrl Pts',(-76.937478300311,-3.53090104645192,-5.7296974884121));
#42011=CARTESIAN_POINT('Ctrl Pts',(-76.8383905150944,-0.364668054766116,
-6.72039527992099));
#42012=CARTESIAN_POINT('Ctrl Pts',(-76.7393027298777,2.89017457637429,-6.07812359422141));
#42013=CARTESIAN_POINT('Ctrl Pts',(-76.640214944661,5.4427420182674,-3.95894617684274));
#42014=CARTESIAN_POINT('Ctrl Pts',(-76.5411271594444,6.67279326610485,-0.877795839803971));
#42015=CARTESIAN_POINT('Ctrl Pts',(-76.4420393742276,6.28144171285588,2.41664757806042));
#42016=CARTESIAN_POINT('Ctrl Pts',(-76.342951589011,4.36378074435504,5.12387676703367));
#42017=CARTESIAN_POINT('Ctrl Pts',(-76.2438638037943,1.3857772715892,6.58606991020427));
#42018=CARTESIAN_POINT('Ctrl Pts',(-76.1447760185777,-1.92895222583112,
6.44793291055455));
#42019=CARTESIAN_POINT('Ctrl Pts',(-76.0456882333609,-4.77497118219338,
4.74303127944292));
#42020=CARTESIAN_POINT('Ctrl Pts',(-75.9466004481443,-6.46073365507635,
1.88563414975306));
#42021=CARTESIAN_POINT('Ctrl Pts',(-75.8475126629276,-6.57662108048484,
-1.42994778655504));
#42022=CARTESIAN_POINT('Ctrl Pts',(-75.7484248777109,-5.09447430696985,
-4.39807083210074));
#42023=CARTESIAN_POINT('Ctrl Pts',(-75.6493370924943,-2.37443590666912,
-6.29751932380295));
#42024=CARTESIAN_POINT('Ctrl Pts',(-75.5502493072776,0.922559830168535,
-6.66675174791372));
#42025=CARTESIAN_POINT('Ctrl Pts',(-75.451161522061,3.99538541319622,-5.41604938202839));
#42026=CARTESIAN_POINT('Ctrl Pts',(-75.3520737368442,6.09738381156011,-2.84931678882429));
#42027=CARTESIAN_POINT('Ctrl Pts',(-75.2529859516277,6.71779649355226,0.409763077604835));
#42028=CARTESIAN_POINT('Ctrl Pts',(-75.1538981664109,5.70587116994455,3.56927579496832));
#42029=CARTESIAN_POINT('Ctrl Pts',(-75.0548103811943,3.30749265819749,5.86150047551997));
#42030=CARTESIAN_POINT('Ctrl Pts',(-74.9557225959776,0.105436039440141,
6.72945605157939));
#42031=CARTESIAN_POINT('Ctrl Pts',(-74.856634810761,-3.12224017861639,5.96224049964313));
#42032=CARTESIAN_POINT('Ctrl Pts',(-74.7575470255443,-5.59125225567696,
3.7462773151408));
#42033=CARTESIAN_POINT('Ctrl Pts',(-74.6584592403276,-6.7016620641815,0.620017004655243));
#42034=CARTESIAN_POINT('Ctrl Pts',(-74.5593714551108,-6.18365432557073,
-2.65689945056294));
#42035=CARTESIAN_POINT('Ctrl Pts',(-74.4602836698943,-4.16309824706767,
-5.28822356692807));
#42036=CARTESIAN_POINT('Ctrl Pts',(-74.3611958846775,-1.13096292583862,
-6.63457748232167));
#42037=CARTESIAN_POINT('Ctrl Pts',(-74.2621080994609,2.17598181668543,-6.36881453977156));
#42038=CARTESIAN_POINT('Ctrl Pts',(-74.1630203142442,4.95419100994433,-4.55551171061364));
#42039=CARTESIAN_POINT('Ctrl Pts',(-74.0639325290275,6.52859561038844,-1.63527822237319));
#42040=CARTESIAN_POINT('Ctrl Pts',(-73.9648447438109,6.51663558245208,1.68230680735436));
#42041=CARTESIAN_POINT('Ctrl Pts',(-73.8657569585942,4.92121705884814,4.59111295529236));
#42042=CARTESIAN_POINT('Ctrl Pts',(-73.7666691733775,2.13000618775729,6.38433780032563));
#42043=CARTESIAN_POINT('Ctrl Pts',(-73.6675813881609,-1.1787687470524,6.62625080641564));
#42044=CARTESIAN_POINT('Ctrl Pts',(-73.5684936029442,-4.20111806187289,
5.25807022953826));
#42045=CARTESIAN_POINT('Ctrl Pts',(-73.4694058177275,-6.20264980876182,
2.6122463242233));
#42046=CARTESIAN_POINT('Ctrl Pts',(-73.3703180325109,-6.69701755805326,
-0.668319785490224));
#42047=CARTESIAN_POINT('Ctrl Pts',(-73.2712302472942,-5.56409631538542,
-3.78649279699112));
#42048=CARTESIAN_POINT('Ctrl Pts',(-73.1721424620775,-3.07917134781474,
-5.98459683849698));
#42049=CARTESIAN_POINT('Ctrl Pts',(-73.0730546768609,0.153952589703362,
-6.7285209451019));
#42050=CARTESIAN_POINT('Ctrl Pts',(-72.9739668916442,3.34966803122509,-5.83750114253862));
#42051=CARTESIAN_POINT('Ctrl Pts',(-72.8748791064275,5.73145729341713,-3.52804376422502));
#42052=CARTESIAN_POINT('Ctrl Pts',(-72.7757913212109,6.72057626908036,-0.36131720139656));
#42053=CARTESIAN_POINT('Ctrl Pts',(-72.6767035359942,6.076681789501,2.89320478668518));
#42054=CARTESIAN_POINT('Ctrl Pts',(-72.5776157507775,3.95623191821552,5.44471528345093));
#42055=CARTESIAN_POINT('Ctrl Pts',(-72.4785279655609,0.874468657149755,
6.67323010814208));
#42056=CARTESIAN_POINT('Ctrl Pts',(-72.3794401803441,-2.41977922221927,
6.28023598475943));
#42057=CARTESIAN_POINT('Ctrl Pts',(-72.2803523951276,-5.12605192351007,
4.36122542251945));
#42058=CARTESIAN_POINT('Ctrl Pts',(-72.1812646099108,-6.586760043996,1.3824932663015));
#42059=CARTESIAN_POINT('Ctrl Pts',(-72.0821768246942,-6.44697032804094,
-1.93216694359235));
#42060=CARTESIAN_POINT('Ctrl Pts',(-71.9830890394775,-4.74064987577426,
-4.77733547742596));
#42061=CARTESIAN_POINT('Ctrl Pts',(-71.8840012542608,-1.88241257534229,
-6.4616730344969));
#42062=CARTESIAN_POINT('Ctrl Pts',(-71.7849134690441,1.43322673062819,-6.57590728699578));
#42063=CARTESIAN_POINT('Ctrl Pts',(-71.6858256838275,4.40061040466765,-5.09228078319352));
#42064=CARTESIAN_POINT('Ctrl Pts',(-71.5867378986108,6.29870244144603,-2.37129565062501));
#42065=CARTESIAN_POINT('Ctrl Pts',(-71.4876501133941,6.66629092828726,0.925883776716208));
#42066=CARTESIAN_POINT('Ctrl Pts',(-71.3885623281775,5.41405659836511,3.99808537405724));
#42067=CARTESIAN_POINT('Ctrl Pts',(-71.2894745429607,2.84627626188227,6.09880373102764));
#42068=CARTESIAN_POINT('Ctrl Pts',(-71.1903867577442,-0.413112538948448,
6.71759134948792));
#42069=CARTESIAN_POINT('Ctrl Pts',(-71.0912989725275,-3.57212031475667,
5.70409080971315));
#42070=CARTESIAN_POINT('Ctrl Pts',(-70.9922111873108,-5.86314887208913,
3.30456968639962));
#42071=CARTESIAN_POINT('Ctrl Pts',(-70.8931234020941,-6.72950778579852,
0.102080700567402));
#42072=CARTESIAN_POINT('Ctrl Pts',(-70.7940356168774,-5.96068300076348,
-3.1252125804432));
#42073=CARTESIAN_POINT('Ctrl Pts',(-70.6949478316608,-3.74348903532561,
-5.59311946510605));
#42074=CARTESIAN_POINT('Ctrl Pts',(-70.5958600464441,-0.616675459979426,
-6.70197037337605));
#42075=CARTESIAN_POINT('Ctrl Pts',(-70.4967722612274,2.65998230779076,-6.18232881936826));
#42076=CARTESIAN_POINT('Ctrl Pts',(-70.3976844760109,5.2902986421166,-4.16046100639949));
#42077=CARTESIAN_POINT('Ctrl Pts',(-70.298596690794,6.63514055893235,-1.1276547662127));
#42078=CARTESIAN_POINT('Ctrl Pts',(-70.1995089055775,6.36772879744182,2.17915705509754));
#42079=CARTESIAN_POINT('Ctrl Pts',(-70.1004211203607,4.55304097074248,4.95646178511361));
#42080=CARTESIAN_POINT('Ctrl Pts',(-70.0013333351441,1.63202284291991,6.52941015320211));
#42081=CARTESIAN_POINT('Ctrl Pts',(-69.9022455499274,-1.68555581112019,
6.51579596949983));
#42082=CARTESIAN_POINT('Ctrl Pts',(-69.8031577647107,-4.5935661173111,4.91892730526103));
#42083=CARTESIAN_POINT('Ctrl Pts',(-69.704069979494,-6.38539903382975,2.12682267415914));
#42084=CARTESIAN_POINT('Ctrl Pts',(-69.6049821942774,-6.62566224533496,
-1.18207246786906));
#42085=CARTESIAN_POINT('Ctrl Pts',(-69.5058944090607,-5.2559748866333,-4.20373922830985));
#42086=CARTESIAN_POINT('Ctrl Pts',(-69.4068066238441,-2.6091533408265,-6.20395151114239));
#42087=CARTESIAN_POINT('Ctrl Pts',(-69.3077188386274,0.671658854258736,
-6.69668349946783));
#42088=CARTESIAN_POINT('Ctrl Pts',(-69.2086310534107,3.78926660043672,-5.56220766776749));
#42089=CARTESIAN_POINT('Ctrl Pts',(-69.109543268194,5.98613137811518,-3.07618702820339));
#42090=CARTESIAN_POINT('Ctrl Pts',(-69.0104554829774,6.72844334753605,0.157307430085179));
#42091=CARTESIAN_POINT('Ctrl Pts',(-68.9113676977607,5.83583026299398,3.35257820938968));
#42092=CARTESIAN_POINT('Ctrl Pts',(-68.8122799125441,3.52518560491299,5.7332156735485));
#42093=CARTESIAN_POINT('Ctrl Pts',(-68.7131921273274,0.357966258194822,
6.72075558748428));
#42094=CARTESIAN_POINT('Ctrl Pts',(-68.6141043421107,-2.89623427771726,
6.07523847406414));
#42095=CARTESIAN_POINT('Ctrl Pts',(-68.5150165568941,-5.44668719508104,
3.95351667609934));
#42096=CARTESIAN_POINT('Ctrl Pts',(-68.4159287716773,-6.67366529112376,
0.87114125699861));
#42097=CARTESIAN_POINT('Ctrl Pts',(-68.3168409864607,-6.2790286954851,-2.42291026460674));
#42098=CARTESIAN_POINT('Ctrl Pts',(-68.217753201244,-4.3586690162214,-5.12822580603616));
#42099=CARTESIAN_POINT('Ctrl Pts',(-68.1186654160274,-1.37920891780825,
-6.58744853945448));
#42100=CARTESIAN_POINT('Ctrl Pts',(-68.0195776308107,1.93538118199903,-6.44600614446938));
#42101=CARTESIAN_POINT('Ctrl Pts',(-67.920489845594,4.77969858297944,-4.73826729013039));
#42102=CARTESIAN_POINT('Ctrl Pts',(-67.8214020603773,6.4626108115923,-1.87919053990488));
#42103=CARTESIAN_POINT('Ctrl Pts',(-67.7223142751607,6.57519185043476,1.43650533248979));
#42104=CARTESIAN_POINT('Ctrl Pts',(-67.623226489944,5.09008601022387,4.40314885463497));
#42105=CARTESIAN_POINT('Ctrl Pts',(-67.5241387047273,2.36815477105034,6.29988405117785));
#42106=CARTESIAN_POINT('Ctrl Pts',(-67.4250509195107,-0.929207424099301,
6.66582833380815));
#42107=CARTESIAN_POINT('Ctrl Pts',(-67.325963134294,-4.00078448088328,5.41206270720496));
#42108=CARTESIAN_POINT('Ctrl Pts',(-67.2268753490773,-6.10022185055814,
2.84323454371856));
#42109=CARTESIAN_POINT('Ctrl Pts',(-67.1277875638607,-6.71738511085694,
-0.416460916761654));
#42110=CARTESIAN_POINT('Ctrl Pts',(-67.0286997786439,-5.7023078643397,-3.57496593570028));
#42111=CARTESIAN_POINT('Ctrl Pts',(-66.9296119934273,-3.30164826000004,
-5.86479177678551));
#42112=CARTESIAN_POINT('Ctrl Pts',(-66.8305242082106,-0.098720535984401,
-6.72956602887435));
#42113=CARTESIAN_POINT('Ctrl Pts',(-66.731436422994,3.12817446980103,-5.95910742627677));
#42114=CARTESIAN_POINT('Ctrl Pts',(-66.6323486377773,5.59500502930411,-3.74073348346592));
#42115=CARTESIAN_POINT('Ctrl Pts',(-66.5332608525606,6.70223695800609,-0.613265438462746));
#42116=CARTESIAN_POINT('Ctrl Pts',(-66.4341730673439,6.18108318358988,2.66292458462869));
#42117=CARTESIAN_POINT('Ctrl Pts',(-66.3350852821273,4.15765412545302,5.29266513173219));
#42118=CARTESIAN_POINT('Ctrl Pts',(-66.2690267586495,2.13569433908622,6.18733216929803));
#42119=CARTESIAN_POINT('Ctrl Pts',(-66.2359974969106,1.07872027397156,6.36642473698023));
#42120=CARTESIAN_POINT('Ctrl Pts',(-86.51072,4.88092761120804,-3.85429840783599));
#42121=CARTESIAN_POINT('Ctrl Pts',(-86.4776907382611,5.52083048049534,-3.04395129593469));
#42122=CARTESIAN_POINT('Ctrl Pts',(-86.4116322147833,6.38855598297889,-1.09916744813806));
#42123=CARTESIAN_POINT('Ctrl Pts',(-86.3125444295668,6.13724916597635,2.08678167705531));
#42124=CARTESIAN_POINT('Ctrl Pts',(-86.2134566443499,4.39481025566226,4.7650088956501));
#42125=CARTESIAN_POINT('Ctrl Pts',(-86.1143688591334,1.5844221326576,6.28572095298091));
#42126=CARTESIAN_POINT('Ctrl Pts',(-86.0152810739166,-1.61092755177724,
6.27892628422283));
#42127=CARTESIAN_POINT('Ctrl Pts',(-85.9161932886999,-4.41485865379402,
4.7465110522202));
#42128=CARTESIAN_POINT('Ctrl Pts',(-85.8171055034833,-6.14602806032999,
2.06071650383196));
#42129=CARTESIAN_POINT('Ctrl Pts',(-85.7180177182666,-6.38379572842379,
-1.12578673393419));
#42130=CARTESIAN_POINT('Ctrl Pts',(-85.6189299330499,-5.07038134923681,
-4.03874760456303));
#42131=CARTESIAN_POINT('Ctrl Pts',(-85.5198421478334,-2.52493057070103,
-5.97034024796873));
#42132=CARTESIAN_POINT('Ctrl Pts',(-85.4207543626165,0.634046276949095,
-6.45121938687785));
#42133=CARTESIAN_POINT('Ctrl Pts',(-85.3216665774001,3.63895781668574,-5.36453420729772));
#42134=CARTESIAN_POINT('Ctrl Pts',(-85.2225787921832,5.75964959979071,-2.97433687429733));
#42135=CARTESIAN_POINT('Ctrl Pts',(-85.1234910069667,6.48082067300681,0.138586273355216));
#42136=CARTESIAN_POINT('Ctrl Pts',(-85.0244032217499,5.62723583982488,3.21783460818738));
#42137=CARTESIAN_POINT('Ctrl Pts',(-84.9253154365333,3.40630517705998,5.51519065308138));
#42138=CARTESIAN_POINT('Ctrl Pts',(-84.8262276513165,0.357686244883394,
6.47242638646756));
#42139=CARTESIAN_POINT('Ctrl Pts',(-84.7271398660999,-2.77784584020579,
5.85694590531591));
#42140=CARTESIAN_POINT('Ctrl Pts',(-84.6280520808834,-5.23839717022127,
3.81830301365183));
#42141=CARTESIAN_POINT('Ctrl Pts',(-84.5289642956664,-6.42608547258025,
0.851861683038723));
#42142=CARTESIAN_POINT('Ctrl Pts',(-84.4298765104501,-6.05231778905693,
-2.32157106432606));
#42143=CARTESIAN_POINT('Ctrl Pts',(-84.3307887252331,-4.20791485226097,
-4.93089194986176));
#42144=CARTESIAN_POINT('Ctrl Pts',(-84.2317009400167,-1.34104281493249,
-6.34206961449874));
#42145=CARTESIAN_POINT('Ctrl Pts',(-84.1326131547998,1.85168535032901,-6.21220606459603));
#42146=CARTESIAN_POINT('Ctrl Pts',(-84.0335253695833,4.59447782990876,-4.57285647015062));
#42147=CARTESIAN_POINT('Ctrl Pts',(-83.9344375843666,6.22087138538862,-1.82236166344391));
#42148=CARTESIAN_POINT('Ctrl Pts',(-83.8353497991498,6.33567333489668,1.37094355079113));
#42149=CARTESIAN_POINT('Ctrl Pts',(-83.7362620139334,4.91098828363557,4.23112714344313));
#42150=CARTESIAN_POINT('Ctrl Pts',(-83.6371742287164,2.29299634549289,6.06320134792872));
#42151=CARTESIAN_POINT('Ctrl Pts',(-83.5380864435,-0.8821641649706,6.4219957343511));
#42152=CARTESIAN_POINT('Ctrl Pts',(-83.4389986582831,-3.84297014786777,
5.22032788899049));
#42153=CARTESIAN_POINT('Ctrl Pts',(-83.3399108730665,-5.86998389207923,
2.75018761772868));
#42154=CARTESIAN_POINT('Ctrl Pts',(-83.2408230878499,-6.47066717086244,
-0.388212815218607));
#42155=CARTESIAN_POINT('Ctrl Pts',(-83.1417353026332,-5.49906168580417,
-3.43228253523767));
#42156=CARTESIAN_POINT('Ctrl Pts',(-83.0426475174165,-3.19125505301957,
-5.64235181573731));
#42157=CARTESIAN_POINT('Ctrl Pts',(-82.9435597321999,-0.108014553846464,
-6.48140229287878));
#42158=CARTESIAN_POINT('Ctrl Pts',(-82.8444719469832,3.0014720904087,-5.7455555098245));
#42159=CARTESIAN_POINT('Ctrl Pts',(-82.7453841617665,5.38163968330173,-3.61361275527539));
#42160=CARTESIAN_POINT('Ctrl Pts',(-82.6462963765498,6.45413816238201,-0.603608653732817));
#42161=CARTESIAN_POINT('Ctrl Pts',(-82.5472085913332,5.95836421374577,2.5530645746496));
#42162=CARTESIAN_POINT('Ctrl Pts',(-82.4481208061165,4.01478452008011,5.08937600136816));
#42163=CARTESIAN_POINT('Ctrl Pts',(-82.3490330208998,1.0956639086878,6.38903462388301));
#42164=CARTESIAN_POINT('Ctrl Pts',(-82.2499452356833,-2.08968891757316,
6.13624013983718));
#42165=CARTESIAN_POINT('Ctrl Pts',(-82.1508574504665,-4.76727425738086,
4.39241835221678));
#42166=CARTESIAN_POINT('Ctrl Pts',(-82.0517696652499,-6.2864733672827,1.58129549054636));
#42167=CARTESIAN_POINT('Ctrl Pts',(-81.9526818800331,-6.27814043472745,
-1.61406180421233));
#42168=CARTESIAN_POINT('Ctrl Pts',(-81.8535940948165,-4.74430025497663,
-4.41722287377553));
#42169=CARTESIAN_POINT('Ctrl Pts',(-81.7545063095999,-2.0576562319405,-6.14705569009534));
#42170=CARTESIAN_POINT('Ctrl Pts',(-81.6554185243831,1.12897174760274,-6.3832331634597));
#42171=CARTESIAN_POINT('Ctrl Pts',(-81.5563307391665,4.04127413651083,-5.06836721040866));
#42172=CARTESIAN_POINT('Ctrl Pts',(-81.4572429539498,5.97159897215335,-2.52195331871032));
#42173=CARTESIAN_POINT('Ctrl Pts',(-81.3581551687331,6.45090218697082,0.637262740250864));
#42174=CARTESIAN_POINT('Ctrl Pts',(-81.2590673835165,5.36271927440909,3.64163216289869));
#42175=CARTESIAN_POINT('Ctrl Pts',(-81.1599795982997,2.97146466365244,5.76113188346196));
#42176=CARTESIAN_POINT('Ctrl Pts',(-81.0608918130833,-0.141817580336693,
6.48075077439986));
#42177=CARTESIAN_POINT('Ctrl Pts',(-80.9618040278663,-3.22063997927572,
5.62563071573915));
#42178=CARTESIAN_POINT('Ctrl Pts',(-80.8627162426499,-5.5168883532987,3.4035548656095));
#42179=CARTESIAN_POINT('Ctrl Pts',(-80.7636284574331,-6.47260392904711,
0.354459029594419));
#42180=CARTESIAN_POINT('Ctrl Pts',(-80.6645406722165,-5.85556013366548,
-2.78076578427677));
#42181=CARTESIAN_POINT('Ctrl Pts',(-80.5654528869998,-3.81569066033551,
-5.24030033591639));
#42182=CARTESIAN_POINT('Ctrl Pts',(-80.4663651017831,-0.84865751236067,
-6.42650941434701));
#42183=CARTESIAN_POINT('Ctrl Pts',(-80.3672773165665,2.32458847824698,-6.05115949490496));
#42184=CARTESIAN_POINT('Ctrl Pts',(-80.2681895313497,4.9329894152624,-4.20545577255142));
#42185=CARTESIAN_POINT('Ctrl Pts',(-80.1691017461332,6.34273747384018,-1.33788047445222));
#42186=CARTESIAN_POINT('Ctrl Pts',(-80.0700139609164,6.21128203689244,1.85478254362996));
#42187=CARTESIAN_POINT('Ctrl Pts',(-79.9709261756998,4.57056508211651,4.59675729793451));
#42188=CARTESIAN_POINT('Ctrl Pts',(-79.871838390483,1.81925969290868,6.22177924678583));
#42189=CARTESIAN_POINT('Ctrl Pts',(-79.7727506052665,-1.37410236497632,
6.3349889910357));
#42190=CARTESIAN_POINT('Ctrl Pts',(-79.6736628200496,-4.23357525011125,
4.90887802126133));
#42191=CARTESIAN_POINT('Ctrl Pts',(-79.5745750348332,-6.06434388870396,
2.28997293117537));
#42192=CARTESIAN_POINT('Ctrl Pts',(-79.4754872496163,-6.42155508654061,
-0.885366080500809));
#42193=CARTESIAN_POINT('Ctrl Pts',(-79.3763994643998,-5.21841112433719,
-3.84557254038601));
#42194=CARTESIAN_POINT('Ctrl Pts',(-79.2773116791831,-2.7472604853497,-5.87135441372885));
#42195=CARTESIAN_POINT('Ctrl Pts',(-79.1782238939664,0.391439059863712,
-6.47047280253847));
#42196=CARTESIAN_POINT('Ctrl Pts',(-79.0791361087498,3.43502395626256,-5.49734965650533));
#42197=CARTESIAN_POINT('Ctrl Pts',(-78.980048323533,5.64394228314933,-3.18844136381023));
#42198=CARTESIAN_POINT('Ctrl Pts',(-78.8809605383164,6.48145534358615,-0.104782894956996));
#42199=CARTESIAN_POINT('Ctrl Pts',(-78.7818727530997,5.74405825318873,3.00433646750017));
#42200=CARTESIAN_POINT('Ctrl Pts',(-78.682784967883,3.61092900537051,5.38344077186245));
#42201=CARTESIAN_POINT('Ctrl Pts',(-78.5836971826664,0.600390527212153,
6.45443832109432));
#42202=CARTESIAN_POINT('Ctrl Pts',(-78.4846093974497,-2.55603511449917,
5.9570905079094));
#42203=CARTESIAN_POINT('Ctrl Pts',(-78.3855216122331,-5.09137715163132,
4.01224644380471));
#42204=CARTESIAN_POINT('Ctrl Pts',(-78.2864338270163,-6.38958013082574,
1.0924781818114));
#42205=CARTESIAN_POINT('Ctrl Pts',(-78.1873460417997,-6.13519745229988,
-2.09274820445987));
#42206=CARTESIAN_POINT('Ctrl Pts',(-78.088258256583,-4.39004082983858,-4.76946373697579));
#42207=CARTESIAN_POINT('Ctrl Pts',(-77.9891704713664,-1.57816084063661,
-6.2872610242504));
#42208=CARTESIAN_POINT('Ctrl Pts',(-77.8900826861497,1.61719190210787,-6.27733487857178));
#42209=CARTESIAN_POINT('Ctrl Pts',(-77.790994900933,4.41958784619184,-4.74209722546579));
#42210=CARTESIAN_POINT('Ctrl Pts',(-77.6919071157163,6.14808087920214,-2.05459103686501));
#42211=CARTESIAN_POINT('Ctrl Pts',(-77.5928193304997,6.3826694615111,1.13215430532706));
#42212=CARTESIAN_POINT('Ctrl Pts',(-77.493731545283,5.06635158971623,4.04380073635643));
#42213=CARTESIAN_POINT('Ctrl Pts',(-77.3946437600663,2.51897554913599,5.97285568290681));
#42214=CARTESIAN_POINT('Ctrl Pts',(-77.2955559748497,-0.640479099061789,
6.45058364410864));
#42215=CARTESIAN_POINT('Ctrl Pts',(-77.196468189633,-3.64430557719005,5.36090287974316));
#42216=CARTESIAN_POINT('Ctrl Pts',(-77.0973804044164,-5.76261274800134,
2.96859177768677));
#42217=CARTESIAN_POINT('Ctrl Pts',(-76.9982926191996,-6.4806792581815,-0.145048883322511));
#42218=CARTESIAN_POINT('Ctrl Pts',(-76.899204833983,-5.6240241962828,-3.22344453428357));
#42219=CARTESIAN_POINT('Ctrl Pts',(-76.8001170487663,-3.40080370644699,
-5.51858468959146));
#42220=CARTESIAN_POINT('Ctrl Pts',(-76.7010292635497,-0.351231726960331,
-6.47277985875879));
#42221=CARTESIAN_POINT('Ctrl Pts',(-76.6019414783329,2.78368503741827,-5.85417290814259));
#42222=CARTESIAN_POINT('Ctrl Pts',(-76.5028536931163,5.24220219865931,-3.81307735750908));
#42223=CARTESIAN_POINT('Ctrl Pts',(-76.4037659078996,6.42693175854569,-0.845453131151542));
#42224=CARTESIAN_POINT('Ctrl Pts',(-76.304678122683,6.04999969635994,2.32760531448557));
#42225=CARTESIAN_POINT('Ctrl Pts',(-76.2055903374662,4.20299564736804,4.93508565418903));
#42226=CARTESIAN_POINT('Ctrl Pts',(-76.1065025522496,1.3347178013573,6.34340375640058));
#42227=CARTESIAN_POINT('Ctrl Pts',(-76.0074147670329,-1.85787927581762,
6.21035646500782));
#42228=CARTESIAN_POINT('Ctrl Pts',(-75.9083269818163,-4.59903562318709,
4.56827255783114));
#42229=CARTESIAN_POINT('Ctrl Pts',(-75.8092391965996,-6.2226855614176,1.81615727009033));
#42230=CARTESIAN_POINT('Ctrl Pts',(-75.710151411383,-6.33430307226678,-1.37726083754989));
#42231=CARTESIAN_POINT('Ctrl Pts',(-75.6110636261662,-4.90676653851619,
-4.23602230429382));
#42232=CARTESIAN_POINT('Ctrl Pts',(-75.5119758409496,-2.28694894755983,
-6.06548492185348));
#42233=CARTESIAN_POINT('Ctrl Pts',(-75.4128880557329,0.888567775924808,
-6.42111284230117));
#42234=CARTESIAN_POINT('Ctrl Pts',(-75.3138002705162,3.84817397687645,-5.21649306236172));
#42235=CARTESIAN_POINT('Ctrl Pts',(-75.2147124852996,5.87272347573166,-2.7443326699887));
#42236=CARTESIAN_POINT('Ctrl Pts',(-75.1156247000829,6.47027682562396,0.394665207195212));
#42237=CARTESIAN_POINT('Ctrl Pts',(-75.0165369148663,5.49563626053907,3.43776452332399));
#42238=CARTESIAN_POINT('Ctrl Pts',(-74.9174491296495,3.18562688193913,5.64553134745027));
#42239=CARTESIAN_POINT('Ctrl Pts',(-74.8183613444329,0.101551210018007,
6.48150678297269));
#42240=CARTESIAN_POINT('Ctrl Pts',(-74.7192735592163,-3.00720009769922,
5.74255956855258));
#42241=CARTESIAN_POINT('Ctrl Pts',(-74.6201857739996,-5.38524052207403,
3.60824435777137));
#42242=CARTESIAN_POINT('Ctrl Pts',(-74.5210979887829,-6.45473687520237,
0.59717225143153));
#42243=CARTESIAN_POINT('Ctrl Pts',(-74.4220102035662,-5.95581532111178,
-2.55900501890618));
#42244=CARTESIAN_POINT('Ctrl Pts',(-74.3229224183495,-4.00970737006563,
-5.09337703615375));
#42245=CARTESIAN_POINT('Ctrl Pts',(-74.2238346331329,-1.08929218333971,
-6.39012404928824));
#42246=CARTESIAN_POINT('Ctrl Pts',(-74.1247468479162,2.09580697107931,-6.13415323952314));
#42247=CARTESIAN_POINT('Ctrl Pts',(-74.0256590626996,4.77165203085921,-4.38766221607524));
#42248=CARTESIAN_POINT('Ctrl Pts',(-73.9265712774829,6.2880471181749,-1.5750257983885));
#42249=CARTESIAN_POINT('Ctrl Pts',(-73.8274834922662,6.27652776184059,1.62032159796177));
#42250=CARTESIAN_POINT('Ctrl Pts',(-73.7283957070496,4.73989301704688,4.42195171987746));
#42251=CARTESIAN_POINT('Ctrl Pts',(-73.6293079218328,2.05152533100835,6.1491045398666));
#42252=CARTESIAN_POINT('Ctrl Pts',(-73.5302201366162,-1.13533658159241,
6.38210417280031));
#42253=CARTESIAN_POINT('Ctrl Pts',(-73.4311323513995,-4.04632633089381,
5.06433470950454));
#42254=CARTESIAN_POINT('Ctrl Pts',(-73.3320445661828,-5.9741109087797,2.51599715333231));
#42255=CARTESIAN_POINT('Ctrl Pts',(-73.2329567809662,-6.45026349760051,
-0.643695298646502));
#42256=CARTESIAN_POINT('Ctrl Pts',(-73.1338689957495,-5.3590851523311,-3.64697808548958));
#42257=CARTESIAN_POINT('Ctrl Pts',(-73.0347812105328,-2.96571815371499,
-5.7640921799276));
#42258=CARTESIAN_POINT('Ctrl Pts',(-72.9356934253162,0.148280150248475,
-6.48060613083523));
#42259=CARTESIAN_POINT('Ctrl Pts',(-72.8366056400995,3.22624828792765,-5.62241627866711));
#42260=CARTESIAN_POINT('Ctrl Pts',(-72.7375178548829,5.52027965393766,-3.3980517018284));
#42261=CARTESIAN_POINT('Ctrl Pts',(-72.6384300696661,6.47295417930641,-0.348004337008301));
#42262=CARTESIAN_POINT('Ctrl Pts',(-72.5393422844495,5.85278422724426,2.78660359852236));
#42263=CARTESIAN_POINT('Ctrl Pts',(-72.4402544992328,3.81046310673336,5.24410275816569));
#42264=CARTESIAN_POINT('Ctrl Pts',(-72.3411667140162,0.842248539758685,
6.42735250497835));
#42265=CARTESIAN_POINT('Ctrl Pts',(-72.2420789287994,-2.33062157207041,
6.04883839375603));
#42266=CARTESIAN_POINT('Ctrl Pts',(-72.1429911435828,-4.93718066622978,
4.20053447729974));
#42267=CARTESIAN_POINT('Ctrl Pts',(-72.0439033583661,-6.34406846196043,
1.33155479644511));
#42268=CARTESIAN_POINT('Ctrl Pts',(-71.9448155731495,-6.20942934919886,
-1.86097554612759));
#42269=CARTESIAN_POINT('Ctrl Pts',(-71.8457277879328,-4.56597889785132,
-4.60131280509741));
#42270=CARTESIAN_POINT('Ctrl Pts',(-71.7466400027161,-1.81305439576657,
-6.22359032905994));
#42271=CARTESIAN_POINT('Ctrl Pts',(-71.6475522174995,1.38041896772984,-6.33361557875979));
#42272=CARTESIAN_POINT('Ctrl Pts',(-71.5484644322828,4.238468305381,-4.90465383592539));
#42273=CARTESIAN_POINT('Ctrl Pts',(-71.4493766470661,6.06662444709443,-2.28392439539779));
#42274=CARTESIAN_POINT('Ctrl Pts',(-71.3502888618495,6.42066900174233,0.89176925044665));
#42275=CARTESIAN_POINT('Ctrl Pts',(-71.2512010766327,5.2145737035411,3.8507744566924));
#42276=CARTESIAN_POINT('Ctrl Pts',(-71.1521132914161,2.7414041723735,5.87409107774727));
#42277=CARTESIAN_POINT('Ctrl Pts',(-71.0530255061994,-0.397891256411005,
6.47007924016768));
#42278=CARTESIAN_POINT('Ctrl Pts',(-70.9539377209828,-3.44050423574074,
5.49392149833132));
#42279=CARTESIAN_POINT('Ctrl Pts',(-70.854849935766,-5.64711900824516,3.18281160810583));
#42280=CARTESIAN_POINT('Ctrl Pts',(-70.7557621505494,-6.4815566110256,0.0983194998327943));
#42281=CARTESIAN_POINT('Ctrl Pts',(-70.6566743653327,-5.74105945628859,
-3.01006298029397));
#42282=CARTESIAN_POINT('Ctrl Pts',(-70.5575865801161,-3.6055588131454,-5.38703893348903));
#42283=CARTESIAN_POINT('Ctrl Pts',(-70.4584987948994,-0.593953827191011,
-6.45503382463191));
#42284=CARTESIAN_POINT('Ctrl Pts',(-70.3594110096827,2.56197428713231,-5.95453865366998));
#42285=CARTESIAN_POINT('Ctrl Pts',(-70.2603232244661,5.09537565443828,-4.00716729949408));
#42286=CARTESIAN_POINT('Ctrl Pts',(-70.1612354392494,6.39066637913534,-1.08610591406471));
#42287=CARTESIAN_POINT('Ctrl Pts',(-70.0621476540327,6.13310750176651,2.09886521667122));
#42288=CARTESIAN_POINT('Ctrl Pts',(-69.9630598688161,4.38528251151797,4.77383913848715));
#42289=CARTESIAN_POINT('Ctrl Pts',(-69.8639720835993,1.57189036458139,6.28883164886079));
#42290=CARTESIAN_POINT('Ctrl Pts',(-69.7648842983828,-1.62345089099596,
6.27571908473456));
#42291=CARTESIAN_POINT('Ctrl Pts',(-69.665796513166,-4.42431449424472,4.73768763026785));
#42292=CARTESIAN_POINT('Ctrl Pts',(-69.5667087279494,-6.15012667183424,
2.04845911513266));
#42293=CARTESIAN_POINT('Ctrl Pts',(-69.4676209427327,-6.38153729746785,
-1.13851857560769));
#42294=CARTESIAN_POINT('Ctrl Pts',(-69.368533157516,-5.062316570275,-4.04885091949506));
#42295=CARTESIAN_POINT('Ctrl Pts',(-69.2694453722994,-2.5130181320396,-5.97536464946014));
#42296=CARTESIAN_POINT('Ctrl Pts',(-69.1703575870826,0.646911338205425,
-6.44994174752579));
#42297=CARTESIAN_POINT('Ctrl Pts',(-69.0712698018661,3.64964968713308,-5.35726609262518));
#42298=CARTESIAN_POINT('Ctrl Pts',(-68.9721820166493,5.76557017887249,-2.96284379245084));
#42299=CARTESIAN_POINT('Ctrl Pts',(-68.8730942314327,6.48053139238009,0.151511380309847));
#42300=CARTESIAN_POINT('Ctrl Pts',(-68.774006446216,5.62080696329017,3.22905123951376));
#42301=CARTESIAN_POINT('Ctrl Pts',(-68.6749186609993,3.39529885244121,5.52197324591022));
#42302=CARTESIAN_POINT('Ctrl Pts',(-68.5758308757827,0.344776860533978,
6.47312689065817));
#42303=CARTESIAN_POINT('Ctrl Pts',(-68.476743090566,-2.78952146684973,5.85139409129237));
#42304=CARTESIAN_POINT('Ctrl Pts',(-68.3776553053494,-5.24600201399085,
3.80784790870568));
#42305=CARTESIAN_POINT('Ctrl Pts',(-68.2785675201326,-6.42777165348394,
0.839043738882656));
#42306=CARTESIAN_POINT('Ctrl Pts',(-68.179479734916,-6.04767558749643,-2.33363725005636));
#42307=CARTESIAN_POINT('Ctrl Pts',(-68.0803919496993,-4.1980722627264,-4.9392744512594));
#42308=CARTESIAN_POINT('Ctrl Pts',(-67.9813041644827,-1.3283914609729,-6.34473158955201));
#42309=CARTESIAN_POINT('Ctrl Pts',(-67.882216379266,1.864071354745,-6.20850069132352));
#42310=CARTESIAN_POINT('Ctrl Pts',(-67.7831285940493,4.60358884116279,-4.5636840994466));
#42311=CARTESIAN_POINT('Ctrl Pts',(-67.6840408088326,6.22449355341539,-1.80995107740288));
#42312=CARTESIAN_POINT('Ctrl Pts',(-67.584953023616,6.33292650272045,1.38357676830714));
#42313=CARTESIAN_POINT('Ctrl Pts',(-67.4858652383993,4.90253993016824,4.24091322523118));
#42314=CARTESIAN_POINT('Ctrl Pts',(-67.3867774531826,2.2808992426794,6.06776251998367));
#42315=CARTESIAN_POINT('Ctrl Pts',(-67.287689667966,-0.894970436826739,
6.42022345172595));
#42316=CARTESIAN_POINT('Ctrl Pts',(-67.1886018827492,-3.8533741139406,5.21265327802973));
#42317=CARTESIAN_POINT('Ctrl Pts',(-67.0895140975326,-5.87545694614519,
2.73847452742765));
#42318=CARTESIAN_POINT('Ctrl Pts',(-66.990426312316,-6.46988060047446,-0.401116262019477));
#42319=CARTESIAN_POINT('Ctrl Pts',(-66.8913385270993,-5.49220424623203,
-3.44324500874027));
#42320=CARTESIAN_POINT('Ctrl Pts',(-66.7922507418826,-3.17999782273006,
-5.64870137951734));
#42321=CARTESIAN_POINT('Ctrl Pts',(-66.693162956666,-0.0950831417423778,
-6.481612708114));
#42322=CARTESIAN_POINT('Ctrl Pts',(-66.5940751714492,3.01291573775549,-5.73954193441991));
#42323=CARTESIAN_POINT('Ctrl Pts',(-66.4949873862326,5.38885502338481,-3.60290479060144));
#42324=CARTESIAN_POINT('Ctrl Pts',(-66.3958996010159,6.45529058685379,-0.590669449163867));
#42325=CARTESIAN_POINT('Ctrl Pts',(-66.2968118157992,5.95333891379727,2.5648081547044));
#42326=CARTESIAN_POINT('Ctrl Pts',(-66.1977240305826,4.00446383910233,5.09765494987877));
#42327=CARTESIAN_POINT('Ctrl Pts',(-66.1316655071048,2.05700390032189,5.9593576533423));
#42328=CARTESIAN_POINT('Ctrl Pts',(-66.0986362453659,1.03897443108136,6.13185148988943));
#42329=CARTESIAN_POINT('Ctrl Pts',(-66.51072,1.15821195975198,6.83557123116185));
#42330=CARTESIAN_POINT('Ctrl Pts',(-66.5437492617389,2.29307521661488,6.64328120120947));
#42331=CARTESIAN_POINT('Ctrl Pts',(-66.5767785234778,3.37855495738465,6.16298334832425));
#42332=CARTESIAN_POINT('Ctrl Pts',(-66.6098077852167,4.28338433193964,5.45224641338801));
#42333=CARTESIAN_POINT('Ctrl Pts',(-66.6428370469556,5.18821370649464,4.74150947845177));
#42334=CARTESIAN_POINT('Ctrl Pts',(-66.6758663086944,5.91239271483488,3.8003334614645));
#42335=CARTESIAN_POINT('Ctrl Pts',(-66.7088955704333,6.36774188186092,2.74347630938123));
#42336=CARTESIAN_POINT('Ctrl Pts',(-66.7419248321722,6.82309104888695,1.686619157298));
#42337=CARTESIAN_POINT('Ctrl Pts',(-66.7749540939112,7.00961037459882,0.514080870118756));
#42338=CARTESIAN_POINT('Ctrl Pts',(-66.80798335565,6.90473259426009,-0.631843848826572));
#42339=CARTESIAN_POINT('Ctrl Pts',(-66.8410126173889,6.79985481392136,-1.77776856777197));
#42340=CARTESIAN_POINT('Ctrl Pts',(-66.8740418791278,6.403579927532,-2.89707971848347));
#42341=CARTESIAN_POINT('Ctrl Pts',(-66.9070711408667,5.7640069664622,-3.85370988397183));
#42342=CARTESIAN_POINT('Ctrl Pts',(-66.9401004026056,5.12443400539243,-4.81034004946015));
#42343=CARTESIAN_POINT('Ctrl Pts',(-66.9731296643445,4.24156296964229,-5.6042892297253));
#42344=CARTESIAN_POINT('Ctrl Pts',(-67.0061589260834,3.22267957537377,-6.13913619659199));
#42345=CARTESIAN_POINT('Ctrl Pts',(-67.0391881878223,2.20379618110529,-6.67398316345867));
#42346=CARTESIAN_POINT('Ctrl Pts',(-67.0722174495611,1.04890042831847,-6.94972791692685));
#42347=CARTESIAN_POINT('Ctrl Pts',(-67.1052467113,-0.101706416420187,-6.93285027714876));
#42348=CARTESIAN_POINT('Ctrl Pts',(-67.1382759730389,-1.2523132611589,-6.91597263737066));
#42349=CARTESIAN_POINT('Ctrl Pts',(-67.1713052347778,-2.39863119784948,
-6.60647260434626));
#42350=CARTESIAN_POINT('Ctrl Pts',(-67.2043344965167,-3.40138449386395,
-6.04196179088377));
#42351=CARTESIAN_POINT('Ctrl Pts',(-67.2373637582556,-4.40413778987836,
-5.47745097742132));
#42352=CARTESIAN_POINT('Ctrl Pts',(-67.2703930199945,-5.26332644521669,
-4.65792938352081));
#42353=CARTESIAN_POINT('Ctrl Pts',(-67.3034222817334,-5.87456727806366,
-3.68295899267487));
#42354=CARTESIAN_POINT('Ctrl Pts',(-67.3364515434723,-6.48580811091063,
-2.70798860182892));
#42355=CARTESIAN_POINT('Ctrl Pts',(-67.3694808052112,-6.84910112126625,
-1.57756941403751));
#42356=CARTESIAN_POINT('Ctrl Pts',(-67.4025100669501,-6.92030721440444,
-0.429042353050756));
#42357=CARTESIAN_POINT('Ctrl Pts',(-67.4066161567646,-6.92915932306131,
-0.286261224482349));
#42358=CARTESIAN_POINT('Ctrl Pts',(-67.4107222465792,-6.93349733082867,
-0.143200245082971));
#42359=CARTESIAN_POINT('Ctrl Pts',(-67.4148283363937,-6.93337279743796,
-0.000131731084783704));
#42360=CARTESIAN_POINT('Origin',(-87.75,0.,0.));
#42361=CARTESIAN_POINT('Origin',(-66.51072,0.,0.));
#42362=CARTESIAN_POINT('Origin',(-66.,9.38757796099391,-1.49533175231994));
#42363=CARTESIAN_POINT('',(-66.,9.50531436582601,-3.4877820755921));
#42364=CARTESIAN_POINT('',(-66.,10.1030411093822,-0.666472311603392));
#42365=CARTESIAN_POINT('Origin',(-66.,0.,0.));
#42366=CARTESIAN_POINT('',(-66.,7.75912709216827,-0.91164851646916));
#42367=CARTESIAN_POINT('Ctrl Pts',(-66.,7.75912709216827,-0.911648516469152));
#42368=CARTESIAN_POINT('Ctrl Pts',(-66.,7.77914589672304,-0.913085729118069));
#42369=CARTESIAN_POINT('Ctrl Pts',(-66.,7.81916111326106,-0.916160028010783));
#42370=CARTESIAN_POINT('Ctrl Pts',(-66.,7.87911675845826,-0.921371110962998));
#42371=CARTESIAN_POINT('Ctrl Pts',(-66.,7.95892309714082,-0.92951996674881));
#42372=CARTESIAN_POINT('Ctrl Pts',(-66.,8.05846479644172,-0.94163789416019));
#42373=CARTESIAN_POINT('Ctrl Pts',(-66.,8.15781635562219,-0.955460858076408));
#42374=CARTESIAN_POINT('Ctrl Pts',(-66.,8.25703088282646,-0.970525968901249));
#42375=CARTESIAN_POINT('Ctrl Pts',(-66.,8.35619956862638,-0.986039820385861));
#42376=CARTESIAN_POINT('Ctrl Pts',(-66.,8.45545727626546,-1.00082385038912));
#42377=CARTESIAN_POINT('Ctrl Pts',(-66.,8.5549523562227,-1.01352414725572));
#42378=CARTESIAN_POINT('Ctrl Pts',(-66.,8.65481931169516,-1.0227982069947));
#42379=CARTESIAN_POINT('Ctrl Pts',(-66.,8.75515237563664,-1.02749863562185));
#42380=CARTESIAN_POINT('Ctrl Pts',(-66.,8.85597360323765,-1.02688738551608));
#42381=CARTESIAN_POINT('Ctrl Pts',(-66.,8.95721840904376,-1.02074993441888));
#42382=CARTESIAN_POINT('Ctrl Pts',(-66.,9.05876930477337,-1.00922949007046));
#42383=CARTESIAN_POINT('Ctrl Pts',(-66.,9.16048129971873,-0.992712229606096));
#42384=CARTESIAN_POINT('Ctrl Pts',(-66.,9.26220852393388,-0.971700897727075));
#42385=CARTESIAN_POINT('Ctrl Pts',(-66.,9.36383468209953,-0.946679483797828));
#42386=CARTESIAN_POINT('Ctrl Pts',(-66.,9.46528658437238,-0.9180359267008));
#42387=CARTESIAN_POINT('Ctrl Pts',(-66.,9.56651871386955,-0.886087649174329));
#42388=CARTESIAN_POINT('Ctrl Pts',(-66.,9.66750440467984,-0.851083007004113));
#42389=CARTESIAN_POINT('Ctrl Pts',(-66.,9.76822511794956,-0.813212594962941));
#42390=CARTESIAN_POINT('Ctrl Pts',(-66.,9.8686591303367,-0.772616048562836));
#42391=CARTESIAN_POINT('Ctrl Pts',(-66.,9.95571582676883,-0.735030406117664));
#42392=CARTESIAN_POINT('Ctrl Pts',(-66.,10.022551212884,-0.704655396487718));
#42393=CARTESIAN_POINT('Ctrl Pts',(-66.,10.0693164096301,-0.682658849179938));
#42394=CARTESIAN_POINT('Ctrl Pts',(-66.,10.0961259401211,-0.669804263759911));
#42395=CARTESIAN_POINT('Ctrl Pts',(-66.,10.1030411093822,-0.666472311603392));
#42396=CARTESIAN_POINT('',(-66.,7.45911616757565,-2.32308894548002));
#42397=CARTESIAN_POINT('Origin',(-66.,0.,0.));
#42398=CARTESIAN_POINT('Ctrl Pts',(-66.,9.50531436582601,-3.4877820755921));
#42399=CARTESIAN_POINT('Ctrl Pts',(-66.,9.49314968148027,-3.47204626414704));
#42400=CARTESIAN_POINT('Ctrl Pts',(-66.,9.46406244582505,-3.43569488186565));
#42401=CARTESIAN_POINT('Ctrl Pts',(-66.,9.41732601303256,-3.38194356049215));
#42402=CARTESIAN_POINT('Ctrl Pts',(-66.,9.35182499787114,-3.31534545781812));
#42403=CARTESIAN_POINT('Ctrl Pts',(-66.,9.2665602360089,-3.23781625057574));
#42404=CARTESIAN_POINT('Ctrl Pts',(-66.,9.17473495202629,-3.15707031802335));
#42405=CARTESIAN_POINT('Ctrl Pts',(-66.,9.08161987720375,-3.07429102783389));
#42406=CARTESIAN_POINT('Ctrl Pts',(-66.,8.98705347372786,-2.99024137111801));
#42407=CARTESIAN_POINT('Ctrl Pts',(-66.,8.89061125688695,-2.90769272800839));
#42408=CARTESIAN_POINT('Ctrl Pts',(-66.,8.79176831392536,-2.8302457596494));
#42409=CARTESIAN_POINT('Ctrl Pts',(-66.,8.69012855448696,-2.76062472778166));
#42410=CARTESIAN_POINT('Ctrl Pts',(-66.,8.58555140837535,-2.69981100640618));
#42411=CARTESIAN_POINT('Ctrl Pts',(-66.,8.47810818661977,-2.64761048501369));
#42412=CARTESIAN_POINT('Ctrl Pts',(-66.,8.36807155833748,-2.6029226992256));
#42413=CARTESIAN_POINT('Ctrl Pts',(-66.,8.25589807840597,-2.56413168225005));
#42414=CARTESIAN_POINT('Ctrl Pts',(-66.,8.14220082613772,-2.52941102084457));
#42415=CARTESIAN_POINT('Ctrl Pts',(-66.,8.02764802899043,-2.49691117466945));
#42416=CARTESIAN_POINT('Ctrl Pts',(-66.,7.91287572547377,-2.46495249663592));
#42417=CARTESIAN_POINT('Ctrl Pts',(-66.,7.79839054163423,-2.43222686627939));
#42418=CARTESIAN_POINT('Ctrl Pts',(-66.,7.68448877252354,-2.39796845787595));
#42419=CARTESIAN_POINT('Ctrl Pts',(-66.,7.5939515764785,-2.36903210935654));
#42420=CARTESIAN_POINT('Ctrl Pts',(-66.,7.52639813136866,-2.34641563722107));
#42421=CARTESIAN_POINT('Ctrl Pts',(-66.,7.48151763438731,-2.3309321471704));
#42422=CARTESIAN_POINT('Ctrl Pts',(-66.,7.45911616757565,-2.32308894548002));
#42423=CARTESIAN_POINT('Ctrl Pts',(-66.,7.45911616757565,-2.32308894548002));
#42424=CARTESIAN_POINT('Ctrl Pts',(-50.,7.45911616757565,-2.32308894548002));
#42425=CARTESIAN_POINT('Ctrl Pts',(-66.,7.48151763438731,-2.3309321471704));
#42426=CARTESIAN_POINT('Ctrl Pts',(-50.,7.48151763438731,-2.3309321471704));
#42427=CARTESIAN_POINT('Ctrl Pts',(-66.,7.52639813136866,-2.34641563722107));
#42428=CARTESIAN_POINT('Ctrl Pts',(-50.,7.52639813136866,-2.34641563722107));
#42429=CARTESIAN_POINT('Ctrl Pts',(-66.,7.5939515764785,-2.36903210935654));
#42430=CARTESIAN_POINT('Ctrl Pts',(-50.,7.5939515764785,-2.36903210935654));
#42431=CARTESIAN_POINT('Ctrl Pts',(-66.,7.68448877252354,-2.39796845787595));
#42432=CARTESIAN_POINT('Ctrl Pts',(-50.,7.68448877252354,-2.39796845787595));
#42433=CARTESIAN_POINT('Ctrl Pts',(-66.,7.79839054163423,-2.43222686627939));
#42434=CARTESIAN_POINT('Ctrl Pts',(-50.,7.79839054163423,-2.43222686627939));
#42435=CARTESIAN_POINT('Ctrl Pts',(-66.,7.91287572547377,-2.46495249663592));
#42436=CARTESIAN_POINT('Ctrl Pts',(-50.,7.91287572547377,-2.46495249663592));
#42437=CARTESIAN_POINT('Ctrl Pts',(-66.,8.02764802899043,-2.49691117466945));
#42438=CARTESIAN_POINT('Ctrl Pts',(-50.,8.02764802899043,-2.49691117466945));
#42439=CARTESIAN_POINT('Ctrl Pts',(-66.,8.14220082613772,-2.52941102084457));
#42440=CARTESIAN_POINT('Ctrl Pts',(-50.,8.14220082613772,-2.52941102084457));
#42441=CARTESIAN_POINT('Ctrl Pts',(-66.,8.25589807840597,-2.56413168225005));
#42442=CARTESIAN_POINT('Ctrl Pts',(-50.,8.25589807840597,-2.56413168225005));
#42443=CARTESIAN_POINT('Ctrl Pts',(-66.,8.36807155833748,-2.6029226992256));
#42444=CARTESIAN_POINT('Ctrl Pts',(-50.,8.36807155833748,-2.6029226992256));
#42445=CARTESIAN_POINT('Ctrl Pts',(-66.,8.47810818661977,-2.64761048501369));
#42446=CARTESIAN_POINT('Ctrl Pts',(-50.,8.47810818661977,-2.64761048501369));
#42447=CARTESIAN_POINT('Ctrl Pts',(-66.,8.58555140837535,-2.69981100640618));
#42448=CARTESIAN_POINT('Ctrl Pts',(-50.,8.58555140837535,-2.69981100640618));
#42449=CARTESIAN_POINT('Ctrl Pts',(-66.,8.69012855448696,-2.76062472778166));
#42450=CARTESIAN_POINT('Ctrl Pts',(-50.,8.69012855448696,-2.76062472778166));
#42451=CARTESIAN_POINT('Ctrl Pts',(-66.,8.79176831392536,-2.8302457596494));
#42452=CARTESIAN_POINT('Ctrl Pts',(-50.,8.79176831392536,-2.8302457596494));
#42453=CARTESIAN_POINT('Ctrl Pts',(-66.,8.89061125688695,-2.90769272800839));
#42454=CARTESIAN_POINT('Ctrl Pts',(-50.,8.89061125688695,-2.90769272800839));
#42455=CARTESIAN_POINT('Ctrl Pts',(-66.,8.98705347372786,-2.99024137111801));
#42456=CARTESIAN_POINT('Ctrl Pts',(-50.,8.98705347372786,-2.99024137111801));
#42457=CARTESIAN_POINT('Ctrl Pts',(-66.,9.08161987720375,-3.07429102783389));
#42458=CARTESIAN_POINT('Ctrl Pts',(-50.,9.08161987720375,-3.07429102783389));
#42459=CARTESIAN_POINT('Ctrl Pts',(-66.,9.17473495202629,-3.15707031802335));
#42460=CARTESIAN_POINT('Ctrl Pts',(-50.,9.17473495202629,-3.15707031802335));
#42461=CARTESIAN_POINT('Ctrl Pts',(-66.,9.2665602360089,-3.23781625057574));
#42462=CARTESIAN_POINT('Ctrl Pts',(-50.,9.2665602360089,-3.23781625057574));
#42463=CARTESIAN_POINT('Ctrl Pts',(-66.,9.3567226928151,-3.31979881460968));
#42464=CARTESIAN_POINT('Ctrl Pts',(-50.,9.3567226928151,-3.31979881460968));
#42465=CARTESIAN_POINT('Ctrl Pts',(-66.,9.44439430274083,-3.40964474504027));
#42466=CARTESIAN_POINT('Ctrl Pts',(-50.,9.44439430274083,-3.40964474504027));
#42467=CARTESIAN_POINT('Ctrl Pts',(-66.,9.52877945206957,-3.51352466905028));
#42468=CARTESIAN_POINT('Ctrl Pts',(-50.,9.52877945206957,-3.51352466905028));
#42469=CARTESIAN_POINT('Ctrl Pts',(-66.,9.60947298443164,-3.63434129183301));
#42470=CARTESIAN_POINT('Ctrl Pts',(-50.,9.60947298443164,-3.63434129183301));
#42471=CARTESIAN_POINT('Ctrl Pts',(-66.,9.6869239989324,-3.76808784102041));
#42472=CARTESIAN_POINT('Ctrl Pts',(-50.,9.6869239989324,-3.76808784102041));
#42473=CARTESIAN_POINT('Ctrl Pts',(-66.,9.7627049188411,-3.90175231914239));
#42474=CARTESIAN_POINT('Ctrl Pts',(-50.,9.7627049188411,-3.90175231914239));
#42475=CARTESIAN_POINT('Ctrl Pts',(-66.,9.83905157879557,-4.01702660556759));
#42476=CARTESIAN_POINT('Ctrl Pts',(-50.,9.83905157879557,-4.01702660556759));
#42477=CARTESIAN_POINT('Ctrl Pts',(-66.,9.91850412115979,-4.09321456481936));
#42478=CARTESIAN_POINT('Ctrl Pts',(-50.,9.91850412115979,-4.09321456481936));
#42479=CARTESIAN_POINT('Ctrl Pts',(-66.,10.003524961334,-4.11032134692824));
#42480=CARTESIAN_POINT('Ctrl Pts',(-50.,10.003524961334,-4.11032134692824));
#42481=CARTESIAN_POINT('Ctrl Pts',(-66.,10.0960897853042,-4.05236656747314));
#42482=CARTESIAN_POINT('Ctrl Pts',(-50.,10.0960897853042,-4.05236656747314));
#42483=CARTESIAN_POINT('Ctrl Pts',(-66.,10.1977063391542,-3.90721566927367));
#42484=CARTESIAN_POINT('Ctrl Pts',(-50.,10.1977063391542,-3.90721566927367));
#42485=CARTESIAN_POINT('Ctrl Pts',(-66.,10.3094940348316,-3.6659181197565));
#42486=CARTESIAN_POINT('Ctrl Pts',(-50.,10.3094940348316,-3.6659181197565));
#42487=CARTESIAN_POINT('Ctrl Pts',(-66.,10.4322386329331,-3.32224944575216));
#42488=CARTESIAN_POINT('Ctrl Pts',(-50.,10.4322386329331,-3.32224944575216));
#42489=CARTESIAN_POINT('Ctrl Pts',(-66.,10.5664542961036,-2.87219453321856));
#42490=CARTESIAN_POINT('Ctrl Pts',(-50.,10.5664542961036,-2.87219453321856));
#42491=CARTESIAN_POINT('Ctrl Pts',(-66.,10.7124395485472,-2.31348157729569));
#42492=CARTESIAN_POINT('Ctrl Pts',(-50.,10.7124395485472,-2.31348157729569));
#42493=CARTESIAN_POINT('Ctrl Pts',(-66.,10.8703331900164,-1.64511745895776));
#42494=CARTESIAN_POINT('Ctrl Pts',(-50.,10.8703331900164,-1.64511745895776));
#42495=CARTESIAN_POINT('Ctrl Pts',(-66.,11.0062009025174,-1.02257826517791));
#42496=CARTESIAN_POINT('Ctrl Pts',(-50.,11.0062009025174,-1.02257826517791));
#42497=CARTESIAN_POINT('Ctrl Pts',(-66.,11.1134656310101,-0.506367938989212));
#42498=CARTESIAN_POINT('Ctrl Pts',(-50.,11.1134656310101,-0.506367938989212));
#42499=CARTESIAN_POINT('Ctrl Pts',(-66.,11.1873562558614,-0.140343105909661));
#42500=CARTESIAN_POINT('Ctrl Pts',(-50.,11.1873562558614,-0.140343105909661));
#42501=CARTESIAN_POINT('Ctrl Pts',(-66.,11.2248967699273,0.048140466098866));
#42502=CARTESIAN_POINT('Ctrl Pts',(-50.,11.2248967699273,0.048140466098866));
#42503=CARTESIAN_POINT('',(-65.5,9.84017809125458,-4.00768263868202));
#42504=CARTESIAN_POINT('Ctrl Pts',(-66.,9.50531436582601,-3.4877820755921));
#42505=CARTESIAN_POINT('Ctrl Pts',(-65.7982417703064,9.65105196151285,-3.67630314699894));
#42506=CARTESIAN_POINT('Ctrl Pts',(-65.6331946192804,9.7436125308195,-3.89166284380022));
#42507=CARTESIAN_POINT('Ctrl Pts',(-65.5,9.84017809125458,-4.00768263868202));
#42508=CARTESIAN_POINT('',(-50.,7.45911616757565,-2.32308894548002));
#42509=CARTESIAN_POINT('',(-66.,7.45911616757565,-2.32308894548002));
#42510=CARTESIAN_POINT('',(-50.,9.50531436582603,-3.48778207559212));
#42511=CARTESIAN_POINT('Ctrl Pts',(-50.,7.45911616757565,-2.32308894548002));
#42512=CARTESIAN_POINT('Ctrl Pts',(-50.,7.48151763438731,-2.3309321471704));
#42513=CARTESIAN_POINT('Ctrl Pts',(-50.,7.52639813136866,-2.34641563722107));
#42514=CARTESIAN_POINT('Ctrl Pts',(-50.,7.5939515764785,-2.36903210935654));
#42515=CARTESIAN_POINT('Ctrl Pts',(-50.,7.68448877252354,-2.39796845787595));
#42516=CARTESIAN_POINT('Ctrl Pts',(-50.,7.79839054163423,-2.43222686627939));
#42517=CARTESIAN_POINT('Ctrl Pts',(-50.,7.91287572547377,-2.46495249663592));
#42518=CARTESIAN_POINT('Ctrl Pts',(-50.,8.02764802899043,-2.49691117466945));
#42519=CARTESIAN_POINT('Ctrl Pts',(-50.,8.14220082613772,-2.52941102084457));
#42520=CARTESIAN_POINT('Ctrl Pts',(-50.,8.25589807840597,-2.56413168225005));
#42521=CARTESIAN_POINT('Ctrl Pts',(-50.,8.36807155833748,-2.6029226992256));
#42522=CARTESIAN_POINT('Ctrl Pts',(-50.,8.47810818661977,-2.64761048501369));
#42523=CARTESIAN_POINT('Ctrl Pts',(-50.,8.58555140837535,-2.69981100640618));
#42524=CARTESIAN_POINT('Ctrl Pts',(-50.,8.69012855448696,-2.76062472778166));
#42525=CARTESIAN_POINT('Ctrl Pts',(-50.,8.79176831392536,-2.8302457596494));
#42526=CARTESIAN_POINT('Ctrl Pts',(-50.,8.89061125688695,-2.90769272800839));
#42527=CARTESIAN_POINT('Ctrl Pts',(-50.,8.98705347372786,-2.99024137111801));
#42528=CARTESIAN_POINT('Ctrl Pts',(-50.,9.08161987720375,-3.07429102783389));
#42529=CARTESIAN_POINT('Ctrl Pts',(-50.,9.17473495202629,-3.15707031802335));
#42530=CARTESIAN_POINT('Ctrl Pts',(-50.,9.2665602360089,-3.23781625057574));
#42531=CARTESIAN_POINT('Ctrl Pts',(-50.,9.35182499787114,-3.31534545781812));
#42532=CARTESIAN_POINT('Ctrl Pts',(-50.,9.41732601303256,-3.38194356049215));
#42533=CARTESIAN_POINT('Ctrl Pts',(-50.,9.46406244582506,-3.43569488186566));
#42534=CARTESIAN_POINT('Ctrl Pts',(-50.,9.49314968148028,-3.47204626414705));
#42535=CARTESIAN_POINT('Ctrl Pts',(-50.,9.50531436582603,-3.48778207559212));
#42536=CARTESIAN_POINT('',(-50.5,9.84017809125458,-4.00768263868202));
#42537=CARTESIAN_POINT('Ctrl Pts',(-50.5,9.84017809125459,-4.00768263868203));
#42538=CARTESIAN_POINT('Ctrl Pts',(-50.4982567069803,9.83891421086397,-4.00616413515951));
#42539=CARTESIAN_POINT('Ctrl Pts',(-50.4965113438768,9.8376533352101,-4.00463244240549));
#42540=CARTESIAN_POINT('Ctrl Pts',(-50.3581212730785,9.73802153669804,-3.88231384117201));
#42541=CARTESIAN_POINT('Ctrl Pts',(-50.2022201285465,9.65138560851398,-3.67673474112415));
#42542=CARTESIAN_POINT('Ctrl Pts',(-50.,9.50531436582603,-3.48778207559212));
#42543=CARTESIAN_POINT('Ctrl Pts',(-65.5,9.84017809125458,-4.00768263868202));
#42544=CARTESIAN_POINT('Ctrl Pts',(-60.5,9.84017809125458,-4.00768263868202));
#42545=CARTESIAN_POINT('Ctrl Pts',(-55.5,9.84017809125458,-4.00768263868202));
#42546=CARTESIAN_POINT('Ctrl Pts',(-50.5,9.84017809125458,-4.00768263868202));
#42547=CARTESIAN_POINT('Origin',(-66.,0.,0.));
#42548=CARTESIAN_POINT('',(-50.,7.75912709216827,-0.91164851646916));
#42549=CARTESIAN_POINT('',(-66.,7.75912709216827,-0.91164851646916));
#42550=CARTESIAN_POINT('Origin',(-50.,0.,0.));
#42551=CARTESIAN_POINT('Ctrl Pts',(-66.,11.2248967699273,0.048140466098866));
#42552=CARTESIAN_POINT('Ctrl Pts',(-50.,11.2248967699273,0.048140466098866));
#42553=CARTESIAN_POINT('Ctrl Pts',(-66.,11.2063599613097,0.0333893783018618));
#42554=CARTESIAN_POINT('Ctrl Pts',(-50.,11.2063599613097,0.0333893783018618));
#42555=CARTESIAN_POINT('Ctrl Pts',(-66.,11.1692224341001,0.00409091359342473));
#42556=CARTESIAN_POINT('Ctrl Pts',(-50.,11.1692224341001,0.00409091359342473));
#42557=CARTESIAN_POINT('Ctrl Pts',(-66.,11.1133244136114,-0.0392456507517008));
#42558=CARTESIAN_POINT('Ctrl Pts',(-50.,11.1133244136114,-0.0392456507517008));
#42559=CARTESIAN_POINT('Ctrl Pts',(-66.,11.0384097481576,-0.0958038462574695));
#42560=CARTESIAN_POINT('Ctrl Pts',(-50.,11.0384097481576,-0.0958038462574695));
#42561=CARTESIAN_POINT('Ctrl Pts',(-66.,10.9441246976668,-0.164449053510359));
#42562=CARTESIAN_POINT('Ctrl Pts',(-50.,10.9441246976668,-0.164449053510359));
#42563=CARTESIAN_POINT('Ctrl Pts',(-66.,10.8491977491253,-0.231019991472708));
#42564=CARTESIAN_POINT('Ctrl Pts',(-50.,10.8491977491253,-0.231019991472708));
#42565=CARTESIAN_POINT('Ctrl Pts',(-66.,10.7536325411685,-0.295485610415231));
#42566=CARTESIAN_POINT('Ctrl Pts',(-50.,10.7536325411685,-0.295485610415231));
#42567=CARTESIAN_POINT('Ctrl Pts',(-66.,10.6574386110001,-0.357805568812489));
#42568=CARTESIAN_POINT('Ctrl Pts',(-50.,10.6574386110001,-0.357805568812489));
#42569=CARTESIAN_POINT('Ctrl Pts',(-66.,10.5606341069048,-0.417929905154785));
#42570=CARTESIAN_POINT('Ctrl Pts',(-50.,10.5606341069048,-0.417929905154785));
#42571=CARTESIAN_POINT('Ctrl Pts',(-66.,10.4632449048126,-0.475801947946924));
#42572=CARTESIAN_POINT('Ctrl Pts',(-50.,10.4632449048126,-0.475801947946924));
#42573=CARTESIAN_POINT('Ctrl Pts',(-66.,10.3653028555026,-0.531361945998192));
#42574=CARTESIAN_POINT('Ctrl Pts',(-50.,10.3653028555026,-0.531361945998192));
#42575=CARTESIAN_POINT('Ctrl Pts',(-66.,10.2668444511909,-0.584551084436177));
#42576=CARTESIAN_POINT('Ctrl Pts',(-50.,10.2668444511909,-0.584551084436177));
#42577=CARTESIAN_POINT('Ctrl Pts',(-66.,10.1679093574848,-0.635314704999891));
#42578=CARTESIAN_POINT('Ctrl Pts',(-50.,10.1679093574848,-0.635314704999891));
#42579=CARTESIAN_POINT('Ctrl Pts',(-66.,10.0685392194901,-0.683608443201678));
#42580=CARTESIAN_POINT('Ctrl Pts',(-50.,10.0685392194901,-0.683608443201678));
#42581=CARTESIAN_POINT('Ctrl Pts',(-66.,9.96877581793761,-0.729391917885004));
#42582=CARTESIAN_POINT('Ctrl Pts',(-50.,9.96877581793761,-0.729391917885004));
#42583=CARTESIAN_POINT('Ctrl Pts',(-66.,9.8686591303367,-0.772616048562836));
#42584=CARTESIAN_POINT('Ctrl Pts',(-50.,9.8686591303367,-0.772616048562836));
#42585=CARTESIAN_POINT('Ctrl Pts',(-66.,9.76822511794956,-0.813212594962941));
#42586=CARTESIAN_POINT('Ctrl Pts',(-50.,9.76822511794956,-0.813212594962941));
#42587=CARTESIAN_POINT('Ctrl Pts',(-66.,9.66750440467984,-0.851083007004113));
#42588=CARTESIAN_POINT('Ctrl Pts',(-50.,9.66750440467984,-0.851083007004113));
#42589=CARTESIAN_POINT('Ctrl Pts',(-66.,9.56651871386955,-0.886087649174329));
#42590=CARTESIAN_POINT('Ctrl Pts',(-50.,9.56651871386955,-0.886087649174329));
#42591=CARTESIAN_POINT('Ctrl Pts',(-66.,9.46528658437238,-0.9180359267008));
#42592=CARTESIAN_POINT('Ctrl Pts',(-50.,9.46528658437238,-0.9180359267008));
#42593=CARTESIAN_POINT('Ctrl Pts',(-66.,9.36383468209953,-0.946679483797828));
#42594=CARTESIAN_POINT('Ctrl Pts',(-50.,9.36383468209953,-0.946679483797828));
#42595=CARTESIAN_POINT('Ctrl Pts',(-66.,9.26220852393388,-0.971700897727075));
#42596=CARTESIAN_POINT('Ctrl Pts',(-50.,9.26220852393388,-0.971700897727075));
#42597=CARTESIAN_POINT('Ctrl Pts',(-66.,9.16048129971873,-0.992712229606096));
#42598=CARTESIAN_POINT('Ctrl Pts',(-50.,9.16048129971873,-0.992712229606096));
#42599=CARTESIAN_POINT('Ctrl Pts',(-66.,9.05876930477337,-1.00922949007046));
#42600=CARTESIAN_POINT('Ctrl Pts',(-50.,9.05876930477337,-1.00922949007046));
#42601=CARTESIAN_POINT('Ctrl Pts',(-66.,8.95721840904376,-1.02074993441888));
#42602=CARTESIAN_POINT('Ctrl Pts',(-50.,8.95721840904376,-1.02074993441888));
#42603=CARTESIAN_POINT('Ctrl Pts',(-66.,8.85597360323765,-1.02688738551608));
#42604=CARTESIAN_POINT('Ctrl Pts',(-50.,8.85597360323765,-1.02688738551608));
#42605=CARTESIAN_POINT('Ctrl Pts',(-66.,8.75515237563664,-1.02749863562185));
#42606=CARTESIAN_POINT('Ctrl Pts',(-50.,8.75515237563664,-1.02749863562185));
#42607=CARTESIAN_POINT('Ctrl Pts',(-66.,8.65481931169516,-1.0227982069947));
#42608=CARTESIAN_POINT('Ctrl Pts',(-50.,8.65481931169516,-1.0227982069947));
#42609=CARTESIAN_POINT('Ctrl Pts',(-66.,8.5549523562227,-1.01352414725572));
#42610=CARTESIAN_POINT('Ctrl Pts',(-50.,8.5549523562227,-1.01352414725572));
#42611=CARTESIAN_POINT('Ctrl Pts',(-66.,8.45545727626546,-1.00082385038912));
#42612=CARTESIAN_POINT('Ctrl Pts',(-50.,8.45545727626546,-1.00082385038912));
#42613=CARTESIAN_POINT('Ctrl Pts',(-66.,8.35619956862638,-0.986039820385861));
#42614=CARTESIAN_POINT('Ctrl Pts',(-50.,8.35619956862638,-0.986039820385861));
#42615=CARTESIAN_POINT('Ctrl Pts',(-66.,8.25703088282646,-0.970525968901249));
#42616=CARTESIAN_POINT('Ctrl Pts',(-50.,8.25703088282646,-0.970525968901249));
#42617=CARTESIAN_POINT('Ctrl Pts',(-66.,8.15781635562219,-0.955460858076408));
#42618=CARTESIAN_POINT('Ctrl Pts',(-50.,8.15781635562219,-0.955460858076408));
#42619=CARTESIAN_POINT('Ctrl Pts',(-66.,8.05846479644172,-0.94163789416019));
#42620=CARTESIAN_POINT('Ctrl Pts',(-50.,8.05846479644172,-0.94163789416019));
#42621=CARTESIAN_POINT('Ctrl Pts',(-66.,7.95892309714082,-0.92951996674881));
#42622=CARTESIAN_POINT('Ctrl Pts',(-50.,7.95892309714082,-0.92951996674881));
#42623=CARTESIAN_POINT('Ctrl Pts',(-66.,7.87911675845826,-0.921371110962998));
#42624=CARTESIAN_POINT('Ctrl Pts',(-50.,7.87911675845826,-0.921371110962998));
#42625=CARTESIAN_POINT('Ctrl Pts',(-66.,7.81916111326106,-0.916160028010783));
#42626=CARTESIAN_POINT('Ctrl Pts',(-50.,7.81916111326106,-0.916160028010783));
#42627=CARTESIAN_POINT('Ctrl Pts',(-66.,7.77914589672304,-0.913085729118069));
#42628=CARTESIAN_POINT('Ctrl Pts',(-50.,7.77914589672304,-0.913085729118069));
#42629=CARTESIAN_POINT('Ctrl Pts',(-66.,7.75912709216827,-0.911648516469152));
#42630=CARTESIAN_POINT('Ctrl Pts',(-50.,7.75912709216827,-0.911648516469152));
#42631=CARTESIAN_POINT('',(-65.5,10.6181350341134,-0.381881391708805));
#42632=CARTESIAN_POINT('Ctrl Pts',(-65.5,10.6181350341134,-0.381881391708781));
#42633=CARTESIAN_POINT('Ctrl Pts',(-65.5867229745674,10.529368555399,-0.437231194499219));
#42634=CARTESIAN_POINT('Ctrl Pts',(-65.6740389226617,10.4396220830013,-0.489919095176194));
#42635=CARTESIAN_POINT('Ctrl Pts',(-65.762054813772,10.3488859652185,-0.539750997576187));
#42636=CARTESIAN_POINT('Ctrl Pts',(-65.8407843210749,10.2677232370167,-0.584325233824076));
#42637=CARTESIAN_POINT('Ctrl Pts',(-65.9200738638956,10.1857705419182,-0.626610595896924));
#42638=CARTESIAN_POINT('Ctrl Pts',(-66.,10.1030411093822,-0.666472311603393));
#42639=CARTESIAN_POINT('',(-50.5,10.6181350341134,-0.381881391708805));
#42640=CARTESIAN_POINT('Ctrl Pts',(-50.5,10.6181350341134,-0.381881391708804));
#42641=CARTESIAN_POINT('Ctrl Pts',(-55.5,10.6181350341134,-0.381881391708804));
#42642=CARTESIAN_POINT('Ctrl Pts',(-60.5,10.6181350341134,-0.381881391708804));
#42643=CARTESIAN_POINT('Ctrl Pts',(-65.5,10.6181350341134,-0.381881391708804));
#42644=CARTESIAN_POINT('',(-50.,10.1030411093822,-0.666472311603383));
#42645=CARTESIAN_POINT('Ctrl Pts',(-50.,10.1030411093822,-0.666472311603383));
#42646=CARTESIAN_POINT('Ctrl Pts',(-50.1024673395144,10.2091023462276,-0.615368578131412));
#42647=CARTESIAN_POINT('Ctrl Pts',(-50.2038883811707,10.3138858386924,-0.560279576022463));
#42648=CARTESIAN_POINT('Ctrl Pts',(-50.3044244416113,10.4173674225829,-0.501495352008985));
#42649=CARTESIAN_POINT('Ctrl Pts',(-50.369977639336,10.4848412095995,-0.463165882533405));
#42650=CARTESIAN_POINT('Ctrl Pts',(-50.4351545856909,10.5517616293991,-0.423268128173657));
#42651=CARTESIAN_POINT('Ctrl Pts',(-50.5,10.6181350341134,-0.381881391708782));
#42652=CARTESIAN_POINT('Ctrl Pts',(-50.,10.1030411093822,-0.666472311603383));
#42653=CARTESIAN_POINT('Ctrl Pts',(-50.,10.0961259401211,-0.669804263759903));
#42654=CARTESIAN_POINT('Ctrl Pts',(-50.,10.0693164096302,-0.682658849179933));
#42655=CARTESIAN_POINT('Ctrl Pts',(-50.,10.022551212884,-0.704655396487715));
#42656=CARTESIAN_POINT('Ctrl Pts',(-50.,9.95571582676884,-0.735030406117662));
#42657=CARTESIAN_POINT('Ctrl Pts',(-50.,9.8686591303367,-0.772616048562836));
#42658=CARTESIAN_POINT('Ctrl Pts',(-50.,9.76822511794956,-0.813212594962941));
#42659=CARTESIAN_POINT('Ctrl Pts',(-50.,9.66750440467984,-0.851083007004113));
#42660=CARTESIAN_POINT('Ctrl Pts',(-50.,9.56651871386955,-0.886087649174329));
#42661=CARTESIAN_POINT('Ctrl Pts',(-50.,9.46528658437238,-0.9180359267008));
#42662=CARTESIAN_POINT('Ctrl Pts',(-50.,9.36383468209953,-0.946679483797828));
#42663=CARTESIAN_POINT('Ctrl Pts',(-50.,9.26220852393388,-0.971700897727075));
#42664=CARTESIAN_POINT('Ctrl Pts',(-50.,9.16048129971873,-0.992712229606096));
#42665=CARTESIAN_POINT('Ctrl Pts',(-50.,9.05876930477337,-1.00922949007046));
#42666=CARTESIAN_POINT('Ctrl Pts',(-50.,8.95721840904376,-1.02074993441888));
#42667=CARTESIAN_POINT('Ctrl Pts',(-50.,8.85597360323765,-1.02688738551608));
#42668=CARTESIAN_POINT('Ctrl Pts',(-50.,8.75515237563664,-1.02749863562185));
#42669=CARTESIAN_POINT('Ctrl Pts',(-50.,8.65481931169516,-1.0227982069947));
#42670=CARTESIAN_POINT('Ctrl Pts',(-50.,8.5549523562227,-1.01352414725572));
#42671=CARTESIAN_POINT('Ctrl Pts',(-50.,8.45545727626546,-1.00082385038912));
#42672=CARTESIAN_POINT('Ctrl Pts',(-50.,8.35619956862638,-0.986039820385861));
#42673=CARTESIAN_POINT('Ctrl Pts',(-50.,8.25703088282646,-0.970525968901249));
#42674=CARTESIAN_POINT('Ctrl Pts',(-50.,8.15781635562219,-0.955460858076408));
#42675=CARTESIAN_POINT('Ctrl Pts',(-50.,8.05846479644172,-0.94163789416019));
#42676=CARTESIAN_POINT('Ctrl Pts',(-50.,7.95892309714082,-0.92951996674881));
#42677=CARTESIAN_POINT('Ctrl Pts',(-50.,7.87911675845826,-0.921371110962998));
#42678=CARTESIAN_POINT('Ctrl Pts',(-50.,7.81916111326106,-0.916160028010783));
#42679=CARTESIAN_POINT('Ctrl Pts',(-50.,7.77914589672304,-0.913085729118069));
#42680=CARTESIAN_POINT('Ctrl Pts',(-50.,7.75912709216827,-0.911648516469152));
#42681=CARTESIAN_POINT('Origin',(-50.,9.38757796099391,-1.49533175231994));
#42682=CARTESIAN_POINT('Origin',(-50.,0.,0.));
#42683=CARTESIAN_POINT('Origin',(-65.75,0.,0.));
#42684=CARTESIAN_POINT('',(-65.5,9.54482387373331,-4.66765061025465));
#42685=CARTESIAN_POINT('Origin',(-65.5,0.,0.));
#42686=CARTESIAN_POINT('',(-66.,8.95850860312801,-4.71812977859675));
#42687=CARTESIAN_POINT('Ctrl Pts',(-65.5,9.54482387373331,-4.66765061025465));
#42688=CARTESIAN_POINT('Ctrl Pts',(-65.6642917360004,9.34854280324816,-4.69504523834513));
#42689=CARTESIAN_POINT('Ctrl Pts',(-65.8311182354841,9.15245906265275,-4.71228445517344));
#42690=CARTESIAN_POINT('Ctrl Pts',(-66.,8.95850860312801,-4.71812977859675));
#42691=CARTESIAN_POINT('Origin',(-66.,0.,0.));
#42692=CARTESIAN_POINT('Origin',(-65.75,0.,0.));
#42693=CARTESIAN_POINT('',(-66.,10.1021455355716,0.67991218413181));
#42694=CARTESIAN_POINT('Origin',(-66.,0.,0.));
#42695=CARTESIAN_POINT('',(-65.5,10.6195213806306,0.341160733863857));
#42696=CARTESIAN_POINT('Ctrl Pts',(-66.,10.1021455355716,0.679912184131811));
#42697=CARTESIAN_POINT('Ctrl Pts',(-65.798241770306,10.3119618818526,0.566966436117564));
#42698=CARTESIAN_POINT('Ctrl Pts',(-65.6331946192801,10.4841148496301,0.407873338586525));
#42699=CARTESIAN_POINT('Ctrl Pts',(-65.5,10.6195213806305,0.34116073386386));
#42700=CARTESIAN_POINT('Origin',(-65.5,0.,0.));
#42701=CARTESIAN_POINT('Origin',(-58.,0.,0.));
#42702=CARTESIAN_POINT('',(-50.5,9.54482387373331,-4.66765061025465));
#42703=CARTESIAN_POINT('Origin',(-50.5,0.,0.));
#42704=CARTESIAN_POINT('Ctrl Pts',(-50.5,9.54482387373331,-4.66765061025465));
#42705=CARTESIAN_POINT('Ctrl Pts',(-55.5,9.54482387373331,-4.66765061025465));
#42706=CARTESIAN_POINT('Ctrl Pts',(-60.5,9.54482387373331,-4.66765061025465));
#42707=CARTESIAN_POINT('Ctrl Pts',(-65.5,9.54482387373331,-4.66765061025465));
#42708=CARTESIAN_POINT('Origin',(-50.25,0.,0.));
#42709=CARTESIAN_POINT('',(-50.,8.95850860312803,-4.71812977859675));
#42710=CARTESIAN_POINT('Origin',(-50.,0.,0.));
#42711=CARTESIAN_POINT('Ctrl Pts',(-50.,8.95850860312803,-4.71812977859675));
#42712=CARTESIAN_POINT('Ctrl Pts',(-50.1688817645162,9.15245906265309,-4.71228445517342));
#42713=CARTESIAN_POINT('Ctrl Pts',(-50.3357082639999,9.34854280324851,-4.69504523834508));
#42714=CARTESIAN_POINT('Ctrl Pts',(-50.5,9.54482387373333,-4.66765061025465));
#42715=CARTESIAN_POINT('Origin',(-66.,7.96777298730851,-5.18432547646766));
#42716=CARTESIAN_POINT('',(-66.,7.26492798915904,-7.0524071289407));
#42717=CARTESIAN_POINT('Origin',(-66.,0.,0.));
#42718=CARTESIAN_POINT('',(-66.,6.71751445306826,-3.98875366785403));
#42719=CARTESIAN_POINT('Ctrl Pts',(-66.,6.71751445306827,-3.98875366785402));
#42720=CARTESIAN_POINT('Ctrl Pts',(-66.,6.73521797398851,-3.99820900830411));
#42721=CARTESIAN_POINT('Ctrl Pts',(-66.,6.77052326328196,-4.01729317493961));
#42722=CARTESIAN_POINT('Ctrl Pts',(-66.,6.82317593222513,-4.04643989396096));
#42723=CARTESIAN_POINT('Ctrl Pts',(-66.,6.89276821217244,-4.08634440644098));
#42724=CARTESIAN_POINT('Ctrl Pts',(-66.,6.97877527429846,-4.1379019406034));
#42725=CARTESIAN_POINT('Ctrl Pts',(-66.,7.06391513395684,-4.19093976616563));
#42726=CARTESIAN_POINT('Ctrl Pts',(-66.,7.148424582012,-4.24505661346796));
#42727=CARTESIAN_POINT('Ctrl Pts',(-66.,7.23270963259088,-4.29956476038277));
#42728=CARTESIAN_POINT('Ctrl Pts',(-66.,7.31737285380592,-4.35344239064242));
#42729=CARTESIAN_POINT('Ctrl Pts',(-66.,7.40310045604506,-4.40551298397998));
#42730=CARTESIAN_POINT('Ctrl Pts',(-66.,7.4905613596596,-4.4546048093515));
#42731=CARTESIAN_POINT('Ctrl Pts',(-66.,7.58030833791389,-4.49970799818987));
#42732=CARTESIAN_POINT('Ctrl Pts',(-66.,7.67266173023884,-4.54015728109748));
#42733=CARTESIAN_POINT('Ctrl Pts',(-66.,7.76764978894924,-4.57573041296856));
#42734=CARTESIAN_POINT('Ctrl Pts',(-66.,7.86510693532357,-4.60651043379445));
#42735=CARTESIAN_POINT('Ctrl Pts',(-66.,7.96474364136776,-4.63279116090914));
#42736=CARTESIAN_POINT('Ctrl Pts',(-66.,8.06622216356313,-4.65497254379874));
#42737=CARTESIAN_POINT('Ctrl Pts',(-66.,8.16923940463961,-4.67344942718086));
#42738=CARTESIAN_POINT('Ctrl Pts',(-66.,8.27357071338958,-4.68854644186826));
#42739=CARTESIAN_POINT('Ctrl Pts',(-66.,8.37904540061237,-4.70053505457754));
#42740=CARTESIAN_POINT('Ctrl Pts',(-66.,8.48553809038739,-4.7096313036054));
#42741=CARTESIAN_POINT('Ctrl Pts',(-66.,8.59295432475099,-4.71600176550966));
#42742=CARTESIAN_POINT('Ctrl Pts',(-66.,8.70121746356333,-4.71976516799885));
#42743=CARTESIAN_POINT('Ctrl Pts',(-66.,8.79603517118228,-4.72083812353456));
#42744=CARTESIAN_POINT('Ctrl Pts',(-66.,8.86944696402783,-4.72027357204841));
#42745=CARTESIAN_POINT('Ctrl Pts',(-66.,8.92111589890229,-4.71919984530889));
#42746=CARTESIAN_POINT('Ctrl Pts',(-66.,8.95083605462571,-4.71836101562288));
#42747=CARTESIAN_POINT('Ctrl Pts',(-66.,8.95850860312801,-4.71812977859675));
#42748=CARTESIAN_POINT('',(-66.,5.86935629366618,-5.15614322415516));
#42749=CARTESIAN_POINT('Origin',(-66.,0.,0.));
#42750=CARTESIAN_POINT('Ctrl Pts',(-66.,7.26492798915904,-7.0524071289407));
#42751=CARTESIAN_POINT('Ctrl Pts',(-66.,7.26021532815457,-7.03308392699787));
#42752=CARTESIAN_POINT('Ctrl Pts',(-66.,7.24842825534665,-6.98804444224892));
#42753=CARTESIAN_POINT('Ctrl Pts',(-66.,7.227595031479,-6.91993074698252));
#42754=CARTESIAN_POINT('Ctrl Pts',(-66.,7.19484476532416,-6.83244868977223));
#42755=CARTESIAN_POINT('Ctrl Pts',(-66.,7.14848549892204,-6.72694193164882));
#42756=CARTESIAN_POINT('Ctrl Pts',(-66.,7.09744125739136,-6.6158281439859));
#42757=CARTESIAN_POINT('Ctrl Pts',(-66.,7.04604577435704,-6.50233218649336));
#42758=CARTESIAN_POINT('Ctrl Pts',(-66.,6.99384114124033,-6.38708538288662));
#42759=CARTESIAN_POINT('Ctrl Pts',(-66.,6.93931235010921,-6.27244686141061));
#42760=CARTESIAN_POINT('Ctrl Pts',(-66.,6.88051534847335,-6.16149248844613));
#42761=CARTESIAN_POINT('Ctrl Pts',(-66.,6.81598023271187,-6.05654989646995));
#42762=CARTESIAN_POINT('Ctrl Pts',(-66.,6.74517942479359,-5.95845844019316));
#42763=CARTESIAN_POINT('Ctrl Pts',(-66.,6.66825702244228,-5.86706979565036));
#42764=CARTESIAN_POINT('Ctrl Pts',(-66.,6.58590972047863,-5.78148954312863));
#42765=CARTESIAN_POINT('Ctrl Pts',(-66.,6.49921187544537,-5.70042712110381));
#42766=CARTESIAN_POINT('Ctrl Pts',(-66.,6.40946643235469,-5.62246337987595));
#42767=CARTESIAN_POINT('Ctrl Pts',(-66.,6.31803612319428,-5.54618047286195));
#42768=CARTESIAN_POINT('Ctrl Pts',(-66.,6.22618517207396,-5.47030266626172));
#42769=CARTESIAN_POINT('Ctrl Pts',(-66.,6.13490846544372,-5.39384099594422));
#42770=CARTESIAN_POINT('Ctrl Pts',(-66.,6.04478817168633,-5.31621635935271));
#42771=CARTESIAN_POINT('Ctrl Pts',(-66.,5.97384780075134,-5.25295689440918));
#42772=CARTESIAN_POINT('Ctrl Pts',(-66.,5.92133360577774,-5.20481925752974));
#42773=CARTESIAN_POINT('Ctrl Pts',(-66.,5.88663093438999,-5.17241984284373));
#42774=CARTESIAN_POINT('Ctrl Pts',(-66.,5.86935629366618,-5.15614322415516));
#42775=CARTESIAN_POINT('Ctrl Pts',(-66.,5.86935629366618,-5.15614322415516));
#42776=CARTESIAN_POINT('Ctrl Pts',(-50.,5.86935629366618,-5.15614322415516));
#42777=CARTESIAN_POINT('Ctrl Pts',(-66.,5.88663093438999,-5.17241984284373));
#42778=CARTESIAN_POINT('Ctrl Pts',(-50.,5.88663093438999,-5.17241984284373));
#42779=CARTESIAN_POINT('Ctrl Pts',(-66.,5.92133360577774,-5.20481925752974));
#42780=CARTESIAN_POINT('Ctrl Pts',(-50.,5.92133360577774,-5.20481925752974));
#42781=CARTESIAN_POINT('Ctrl Pts',(-66.,5.97384780075134,-5.25295689440918));
#42782=CARTESIAN_POINT('Ctrl Pts',(-50.,5.97384780075134,-5.25295689440918));
#42783=CARTESIAN_POINT('Ctrl Pts',(-66.,6.04478817168633,-5.31621635935271));
#42784=CARTESIAN_POINT('Ctrl Pts',(-50.,6.04478817168633,-5.31621635935271));
#42785=CARTESIAN_POINT('Ctrl Pts',(-66.,6.13490846544372,-5.39384099594422));
#42786=CARTESIAN_POINT('Ctrl Pts',(-50.,6.13490846544372,-5.39384099594422));
#42787=CARTESIAN_POINT('Ctrl Pts',(-66.,6.22618517207396,-5.47030266626172));
#42788=CARTESIAN_POINT('Ctrl Pts',(-50.,6.22618517207396,-5.47030266626172));
#42789=CARTESIAN_POINT('Ctrl Pts',(-66.,6.31803612319428,-5.54618047286195));
#42790=CARTESIAN_POINT('Ctrl Pts',(-50.,6.31803612319428,-5.54618047286195));
#42791=CARTESIAN_POINT('Ctrl Pts',(-66.,6.40946643235469,-5.62246337987595));
#42792=CARTESIAN_POINT('Ctrl Pts',(-50.,6.40946643235469,-5.62246337987595));
#42793=CARTESIAN_POINT('Ctrl Pts',(-66.,6.49921187544537,-5.70042712110381));
#42794=CARTESIAN_POINT('Ctrl Pts',(-50.,6.49921187544537,-5.70042712110381));
#42795=CARTESIAN_POINT('Ctrl Pts',(-66.,6.58590972047863,-5.78148954312863));
#42796=CARTESIAN_POINT('Ctrl Pts',(-50.,6.58590972047863,-5.78148954312863));
#42797=CARTESIAN_POINT('Ctrl Pts',(-66.,6.66825702244228,-5.86706979565036));
#42798=CARTESIAN_POINT('Ctrl Pts',(-50.,6.66825702244228,-5.86706979565036));
#42799=CARTESIAN_POINT('Ctrl Pts',(-66.,6.74517942479359,-5.95845844019316));
#42800=CARTESIAN_POINT('Ctrl Pts',(-50.,6.74517942479359,-5.95845844019316));
#42801=CARTESIAN_POINT('Ctrl Pts',(-66.,6.81598023271187,-6.05654989646995));
#42802=CARTESIAN_POINT('Ctrl Pts',(-50.,6.81598023271187,-6.05654989646995));
#42803=CARTESIAN_POINT('Ctrl Pts',(-66.,6.88051534847335,-6.16149248844613));
#42804=CARTESIAN_POINT('Ctrl Pts',(-50.,6.88051534847335,-6.16149248844613));
#42805=CARTESIAN_POINT('Ctrl Pts',(-66.,6.93931235010921,-6.27244686141061));
#42806=CARTESIAN_POINT('Ctrl Pts',(-50.,6.93931235010921,-6.27244686141061));
#42807=CARTESIAN_POINT('Ctrl Pts',(-66.,6.99384114124033,-6.38708538288662));
#42808=CARTESIAN_POINT('Ctrl Pts',(-50.,6.99384114124033,-6.38708538288662));
#42809=CARTESIAN_POINT('Ctrl Pts',(-66.,7.04604577435704,-6.50233218649336));
#42810=CARTESIAN_POINT('Ctrl Pts',(-50.,7.04604577435704,-6.50233218649336));
#42811=CARTESIAN_POINT('Ctrl Pts',(-66.,7.09744125739136,-6.6158281439859));
#42812=CARTESIAN_POINT('Ctrl Pts',(-50.,7.09744125739136,-6.6158281439859));
#42813=CARTESIAN_POINT('Ctrl Pts',(-66.,7.14848549892204,-6.72694193164882));
#42814=CARTESIAN_POINT('Ctrl Pts',(-50.,7.14848549892204,-6.72694193164882));
#42815=CARTESIAN_POINT('Ctrl Pts',(-66.,7.19750768890132,-6.83850910564074));
#42816=CARTESIAN_POINT('Ctrl Pts',(-50.,7.19750768890132,-6.83850910564074));
#42817=CARTESIAN_POINT('Ctrl Pts',(-66.,7.24105605777582,-6.95624670358752));
#42818=CARTESIAN_POINT('Ctrl Pts',(-50.,7.24105605777582,-6.95624670358752));
#42819=CARTESIAN_POINT('Ctrl Pts',(-66.,7.27589395606278,-7.08546826867055));
#42820=CARTESIAN_POINT('Ctrl Pts',(-50.,7.27589395606278,-7.08546826867055));
#42821=CARTESIAN_POINT('Ctrl Pts',(-66.,7.30047061843489,-7.22866076209231));
#42822=CARTESIAN_POINT('Ctrl Pts',(-50.,7.30047061843489,-7.22866076209231));
#42823=CARTESIAN_POINT('Ctrl Pts',(-66.,7.31682601848242,-7.38234648021868));
#42824=CARTESIAN_POINT('Ctrl Pts',(-50.,7.31682601848242,-7.38234648021868));
#42825=CARTESIAN_POINT('Ctrl Pts',(-66.,7.33168909251117,-7.53527793402804));
#42826=CARTESIAN_POINT('Ctrl Pts',(-50.,7.33168909251117,-7.53527793402804));
#42827=CARTESIAN_POINT('Ctrl Pts',(-66.,7.35454896062522,-7.67163921895471));
#42828=CARTESIAN_POINT('Ctrl Pts',(-50.,7.35454896062522,-7.67163921895471));
#42829=CARTESIAN_POINT('Ctrl Pts',(-66.,7.39614403501135,-7.77355664342129));
#42830=CARTESIAN_POINT('Ctrl Pts',(-50.,7.39614403501135,-7.77355664342129));
#42831=CARTESIAN_POINT('Ctrl Pts',(-66.,7.46685648222862,-7.82376555763565));
#42832=CARTESIAN_POINT('Ctrl Pts',(-50.,7.46685648222862,-7.82376555763565));
#42833=CARTESIAN_POINT('Ctrl Pts',(-66.,7.57499098914986,-7.80847073788432));
#42834=CARTESIAN_POINT('Ctrl Pts',(-50.,7.57499098914986,-7.80847073788432));
#42835=CARTESIAN_POINT('Ctrl Pts',(-66.,7.72686051941396,-7.71719997015535));
#42836=CARTESIAN_POINT('Ctrl Pts',(-50.,7.72686051941396,-7.71719997015535));
#42837=CARTESIAN_POINT('Ctrl Pts',(-66.,7.9271282162934,-7.54223184193065));
#42838=CARTESIAN_POINT('Ctrl Pts',(-50.,7.9271282162934,-7.54223184193065));
#42839=CARTESIAN_POINT('Ctrl Pts',(-66.,8.17904362913404,-7.27819961164743));
#42840=CARTESIAN_POINT('Ctrl Pts',(-50.,8.17904362913404,-7.27819961164743));
#42841=CARTESIAN_POINT('Ctrl Pts',(-66.,8.48470956289165,-6.92164441889879));
#42842=CARTESIAN_POINT('Ctrl Pts',(-50.,8.48470956289165,-6.92164441889879));
#42843=CARTESIAN_POINT('Ctrl Pts',(-66.,8.84532275927927,-6.47061228740683));
#42844=CARTESIAN_POINT('Ctrl Pts',(-50.,8.84532275927927,-6.47061228740683));
#42845=CARTESIAN_POINT('Ctrl Pts',(-66.,9.26141395607925,-5.92425241274213));
#42846=CARTESIAN_POINT('Ctrl Pts',(-50.,9.26141395607925,-5.92425241274213));
#42847=CARTESIAN_POINT('Ctrl Pts',(-66.,9.63874478953592,-5.41079693734509));
#42848=CARTESIAN_POINT('Ctrl Pts',(-50.,9.63874478953592,-5.41079693734509));
#42849=CARTESIAN_POINT('Ctrl Pts',(-66.,9.94669765021079,-4.98284383425478));
#42850=CARTESIAN_POINT('Ctrl Pts',(-50.,9.94669765021079,-4.98284383425478));
#42851=CARTESIAN_POINT('Ctrl Pts',(-66.,10.1630758067952,-4.67851753531735));
#42852=CARTESIAN_POINT('Ctrl Pts',(-50.,10.1630758067952,-4.67851753531735));
#42853=CARTESIAN_POINT('Ctrl Pts',(-66.,10.2740339482513,-4.52159832693919));
#42854=CARTESIAN_POINT('Ctrl Pts',(-50.,10.2740339482513,-4.52159832693919));
#42855=CARTESIAN_POINT('',(-65.5,7.35937861468917,-7.663561274346));
#42856=CARTESIAN_POINT('Ctrl Pts',(-66.,7.26492798915904,-7.0524071289407));
#42857=CARTESIAN_POINT('Ctrl Pts',(-65.7982417703062,7.32138747997352,-7.28390651783422));
#42858=CARTESIAN_POINT('Ctrl Pts',(-65.6331946192802,7.31835108748961,-7.51829516584718));
#42859=CARTESIAN_POINT('Ctrl Pts',(-65.5,7.35937861468917,-7.66356127434599));
#42860=CARTESIAN_POINT('',(-50.,5.86935629366618,-5.15614322415516));
#42861=CARTESIAN_POINT('',(-66.,5.86935629366618,-5.15614322415516));
#42862=CARTESIAN_POINT('',(-50.,7.26492798915904,-7.05240712894072));
#42863=CARTESIAN_POINT('Ctrl Pts',(-50.,5.86935629366618,-5.15614322415516));
#42864=CARTESIAN_POINT('Ctrl Pts',(-50.,5.88663093438999,-5.17241984284373));
#42865=CARTESIAN_POINT('Ctrl Pts',(-50.,5.92133360577774,-5.20481925752974));
#42866=CARTESIAN_POINT('Ctrl Pts',(-50.,5.97384780075134,-5.25295689440918));
#42867=CARTESIAN_POINT('Ctrl Pts',(-50.,6.04478817168633,-5.31621635935271));
#42868=CARTESIAN_POINT('Ctrl Pts',(-50.,6.13490846544372,-5.39384099594422));
#42869=CARTESIAN_POINT('Ctrl Pts',(-50.,6.22618517207396,-5.47030266626172));
#42870=CARTESIAN_POINT('Ctrl Pts',(-50.,6.31803612319428,-5.54618047286195));
#42871=CARTESIAN_POINT('Ctrl Pts',(-50.,6.40946643235469,-5.62246337987595));
#42872=CARTESIAN_POINT('Ctrl Pts',(-50.,6.49921187544537,-5.70042712110381));
#42873=CARTESIAN_POINT('Ctrl Pts',(-50.,6.58590972047863,-5.78148954312863));
#42874=CARTESIAN_POINT('Ctrl Pts',(-50.,6.66825702244228,-5.86706979565036));
#42875=CARTESIAN_POINT('Ctrl Pts',(-50.,6.74517942479359,-5.95845844019316));
#42876=CARTESIAN_POINT('Ctrl Pts',(-50.,6.81598023271187,-6.05654989646995));
#42877=CARTESIAN_POINT('Ctrl Pts',(-50.,6.88051534847335,-6.16149248844613));
#42878=CARTESIAN_POINT('Ctrl Pts',(-50.,6.93931235010921,-6.27244686141061));
#42879=CARTESIAN_POINT('Ctrl Pts',(-50.,6.99384114124033,-6.38708538288662));
#42880=CARTESIAN_POINT('Ctrl Pts',(-50.,7.04604577435704,-6.50233218649336));
#42881=CARTESIAN_POINT('Ctrl Pts',(-50.,7.09744125739136,-6.6158281439859));
#42882=CARTESIAN_POINT('Ctrl Pts',(-50.,7.14848549892204,-6.72694193164882));
#42883=CARTESIAN_POINT('Ctrl Pts',(-50.,7.19484476532416,-6.83244868977223));
#42884=CARTESIAN_POINT('Ctrl Pts',(-50.,7.227595031479,-6.91993074698252));
#42885=CARTESIAN_POINT('Ctrl Pts',(-50.,7.24842825534666,-6.98804444224893));
#42886=CARTESIAN_POINT('Ctrl Pts',(-50.,7.26021532815457,-7.03308392699788));
#42887=CARTESIAN_POINT('Ctrl Pts',(-50.,7.26492798915904,-7.05240712894072));
#42888=CARTESIAN_POINT('',(-50.5,7.35937861468917,-7.663561274346));
#42889=CARTESIAN_POINT('Ctrl Pts',(-50.5,7.35937861468918,-7.66356127434601));
#42890=CARTESIAN_POINT('Ctrl Pts',(-50.4982567069799,7.35884163352443,-7.66165998588276));
#42891=CARTESIAN_POINT('Ctrl Pts',(-50.4965113438759,7.35831276186704,-7.65974787059353));
#42892=CARTESIAN_POINT('Ctrl Pts',(-50.3581212730773,7.31704604215131,-7.50748036478051));
#42893=CARTESIAN_POINT('Ctrl Pts',(-50.2022201285457,7.32151673652989,-7.28443650514684));
#42894=CARTESIAN_POINT('Ctrl Pts',(-50.,7.26492798915904,-7.05240712894072));
#42895=CARTESIAN_POINT('Ctrl Pts',(-65.5,7.35937861468917,-7.663561274346));
#42896=CARTESIAN_POINT('Ctrl Pts',(-60.5,7.35937861468917,-7.663561274346));
#42897=CARTESIAN_POINT('Ctrl Pts',(-55.5,7.35937861468917,-7.663561274346));
#42898=CARTESIAN_POINT('Ctrl Pts',(-50.5,7.35937861468917,-7.663561274346));
#42899=CARTESIAN_POINT('Origin',(-66.,0.,0.));
#42900=CARTESIAN_POINT('',(-50.,6.71751445306826,-3.98875366785403));
#42901=CARTESIAN_POINT('',(-66.,6.71751445306826,-3.98875366785403));
#42902=CARTESIAN_POINT('Origin',(-50.,0.,0.));
#42903=CARTESIAN_POINT('Ctrl Pts',(-66.,10.2740339482513,-4.52159832693919));
#42904=CARTESIAN_POINT('Ctrl Pts',(-50.,10.2740339482513,-4.52159832693919));
#42905=CARTESIAN_POINT('Ctrl Pts',(-66.,10.2510999230073,-4.527534516881));
#42906=CARTESIAN_POINT('Ctrl Pts',(-50.,10.2510999230073,-4.527534516881));
#42907=CARTESIAN_POINT('Ctrl Pts',(-66.,10.2052563445341,-4.53919480308192));
#42908=CARTESIAN_POINT('Ctrl Pts',(-50.,10.2052563445341,-4.53919480308192));
#42909=CARTESIAN_POINT('Ctrl Pts',(-66.,10.1365643931213,-4.55604895138109));
#42910=CARTESIAN_POINT('Ctrl Pts',(-50.,10.1365643931213,-4.55604895138109));
#42911=CARTESIAN_POINT('Ctrl Pts',(-66.,10.0451221502067,-4.57724689443403));
#42912=CARTESIAN_POINT('Ctrl Pts',(-50.,10.0451221502067,-4.57724689443403));
#42913=CARTESIAN_POINT('Ctrl Pts',(-66.,9.93106794944591,-4.60160822677996));
#42914=CARTESIAN_POINT('Ctrl Pts',(-50.,9.93106794944591,-4.60160822677996));
#42915=CARTESIAN_POINT('Ctrl Pts',(-66.,9.81727102696474,-4.62381353637928));
#42916=CARTESIAN_POINT('Ctrl Pts',(-50.,9.81727102696474,-4.62381353637928));
#42917=CARTESIAN_POINT('Ctrl Pts',(-66.,9.70374733588469,-4.64383593785917));
#42918=CARTESIAN_POINT('Ctrl Pts',(-50.,9.70374733588469,-4.64383593785917));
#42919=CARTESIAN_POINT('Ctrl Pts',(-66.,9.59052199725138,-4.66164245653247));
#42920=CARTESIAN_POINT('Ctrl Pts',(-50.,9.59052199725138,-4.66164245653247));
#42921=CARTESIAN_POINT('Ctrl Pts',(-66.,9.47763191152479,-4.67719483186143));
#42922=CARTESIAN_POINT('Ctrl Pts',(-50.,9.47763191152479,-4.67719483186143));
#42923=CARTESIAN_POINT('Ctrl Pts',(-66.,9.36512376791676,-4.69045181654785));
#42924=CARTESIAN_POINT('Ctrl Pts',(-50.,9.36512376791676,-4.69045181654785));
#42925=CARTESIAN_POINT('Ctrl Pts',(-66.,9.25305096656076,-4.70137178004192));
#42926=CARTESIAN_POINT('Ctrl Pts',(-50.,9.25305096656076,-4.70137178004192));
#42927=CARTESIAN_POINT('Ctrl Pts',(-66.,9.14147076691866,-4.7099158350055));
#42928=CARTESIAN_POINT('Ctrl Pts',(-50.,9.14147076691866,-4.7099158350055));
#42929=CARTESIAN_POINT('Ctrl Pts',(-66.,9.03044163684364,-4.7160501820886));
#42930=CARTESIAN_POINT('Ctrl Pts',(-50.,9.03044163684364,-4.7160501820886));
#42931=CARTESIAN_POINT('Ctrl Pts',(-66.,8.92001966569546,-4.71975123090547));
#42932=CARTESIAN_POINT('Ctrl Pts',(-50.,8.92001966569546,-4.71975123090547));
#42933=CARTESIAN_POINT('Ctrl Pts',(-66.,8.81025944656715,-4.72099908518823));
#42934=CARTESIAN_POINT('Ctrl Pts',(-50.,8.81025944656715,-4.72099908518823));
#42935=CARTESIAN_POINT('Ctrl Pts',(-66.,8.70121746356333,-4.71976516799885));
#42936=CARTESIAN_POINT('Ctrl Pts',(-50.,8.70121746356333,-4.71976516799885));
#42937=CARTESIAN_POINT('Ctrl Pts',(-66.,8.59295432475099,-4.71600176550966));
#42938=CARTESIAN_POINT('Ctrl Pts',(-50.,8.59295432475099,-4.71600176550966));
#42939=CARTESIAN_POINT('Ctrl Pts',(-66.,8.48553809038739,-4.7096313036054));
#42940=CARTESIAN_POINT('Ctrl Pts',(-50.,8.48553809038739,-4.7096313036054));
#42941=CARTESIAN_POINT('Ctrl Pts',(-66.,8.37904540061237,-4.70053505457754));
#42942=CARTESIAN_POINT('Ctrl Pts',(-50.,8.37904540061237,-4.70053505457754));
#42943=CARTESIAN_POINT('Ctrl Pts',(-66.,8.27357071338958,-4.68854644186826));
#42944=CARTESIAN_POINT('Ctrl Pts',(-50.,8.27357071338958,-4.68854644186826));
#42945=CARTESIAN_POINT('Ctrl Pts',(-66.,8.16923940463961,-4.67344942718086));
#42946=CARTESIAN_POINT('Ctrl Pts',(-50.,8.16923940463961,-4.67344942718086));
#42947=CARTESIAN_POINT('Ctrl Pts',(-66.,8.06622216356313,-4.65497254379874));
#42948=CARTESIAN_POINT('Ctrl Pts',(-50.,8.06622216356313,-4.65497254379874));
#42949=CARTESIAN_POINT('Ctrl Pts',(-66.,7.96474364136776,-4.63279116090914));
#42950=CARTESIAN_POINT('Ctrl Pts',(-50.,7.96474364136776,-4.63279116090914));
#42951=CARTESIAN_POINT('Ctrl Pts',(-66.,7.86510693532357,-4.60651043379445));
#42952=CARTESIAN_POINT('Ctrl Pts',(-50.,7.86510693532357,-4.60651043379445));
#42953=CARTESIAN_POINT('Ctrl Pts',(-66.,7.76764978894924,-4.57573041296856));
#42954=CARTESIAN_POINT('Ctrl Pts',(-50.,7.76764978894924,-4.57573041296856));
#42955=CARTESIAN_POINT('Ctrl Pts',(-66.,7.67266173023884,-4.54015728109748));
#42956=CARTESIAN_POINT('Ctrl Pts',(-50.,7.67266173023884,-4.54015728109748));
#42957=CARTESIAN_POINT('Ctrl Pts',(-66.,7.58030833791389,-4.49970799818987));
#42958=CARTESIAN_POINT('Ctrl Pts',(-50.,7.58030833791389,-4.49970799818987));
#42959=CARTESIAN_POINT('Ctrl Pts',(-66.,7.4905613596596,-4.4546048093515));
#42960=CARTESIAN_POINT('Ctrl Pts',(-50.,7.4905613596596,-4.4546048093515));
#42961=CARTESIAN_POINT('Ctrl Pts',(-66.,7.40310045604506,-4.40551298397998));
#42962=CARTESIAN_POINT('Ctrl Pts',(-50.,7.40310045604506,-4.40551298397998));
#42963=CARTESIAN_POINT('Ctrl Pts',(-66.,7.31737285380592,-4.35344239064242));
#42964=CARTESIAN_POINT('Ctrl Pts',(-50.,7.31737285380592,-4.35344239064242));
#42965=CARTESIAN_POINT('Ctrl Pts',(-66.,7.23270963259088,-4.29956476038277));
#42966=CARTESIAN_POINT('Ctrl Pts',(-50.,7.23270963259088,-4.29956476038277));
#42967=CARTESIAN_POINT('Ctrl Pts',(-66.,7.148424582012,-4.24505661346796));
#42968=CARTESIAN_POINT('Ctrl Pts',(-50.,7.148424582012,-4.24505661346796));
#42969=CARTESIAN_POINT('Ctrl Pts',(-66.,7.06391513395684,-4.19093976616563));
#42970=CARTESIAN_POINT('Ctrl Pts',(-50.,7.06391513395684,-4.19093976616563));
#42971=CARTESIAN_POINT('Ctrl Pts',(-66.,6.97877527429846,-4.1379019406034));
#42972=CARTESIAN_POINT('Ctrl Pts',(-50.,6.97877527429846,-4.1379019406034));
#42973=CARTESIAN_POINT('Ctrl Pts',(-66.,6.89276821217244,-4.08634440644098));
#42974=CARTESIAN_POINT('Ctrl Pts',(-50.,6.89276821217244,-4.08634440644098));
#42975=CARTESIAN_POINT('Ctrl Pts',(-66.,6.82317593222513,-4.04643989396096));
#42976=CARTESIAN_POINT('Ctrl Pts',(-50.,6.82317593222513,-4.04643989396096));
#42977=CARTESIAN_POINT('Ctrl Pts',(-66.,6.77052326328196,-4.01729317493961));
#42978=CARTESIAN_POINT('Ctrl Pts',(-50.,6.77052326328196,-4.01729317493961));
#42979=CARTESIAN_POINT('Ctrl Pts',(-66.,6.73521797398851,-3.99820900830411));
#42980=CARTESIAN_POINT('Ctrl Pts',(-50.,6.73521797398851,-3.99820900830411));
#42981=CARTESIAN_POINT('Ctrl Pts',(-66.,6.71751445306827,-3.98875366785402));
#42982=CARTESIAN_POINT('Ctrl Pts',(-50.,6.71751445306827,-3.98875366785402));
#42983=CARTESIAN_POINT('Ctrl Pts',(-50.,8.95850860312803,-4.71812977859675));
#42984=CARTESIAN_POINT('Ctrl Pts',(-50.,8.95083605462573,-4.71836101562288));
#42985=CARTESIAN_POINT('Ctrl Pts',(-50.,8.9211158989023,-4.71919984530889));
#42986=CARTESIAN_POINT('Ctrl Pts',(-50.,8.86944696402783,-4.72027357204841));
#42987=CARTESIAN_POINT('Ctrl Pts',(-50.,8.79603517118229,-4.72083812353456));
#42988=CARTESIAN_POINT('Ctrl Pts',(-50.,8.70121746356333,-4.71976516799885));
#42989=CARTESIAN_POINT('Ctrl Pts',(-50.,8.59295432475099,-4.71600176550966));
#42990=CARTESIAN_POINT('Ctrl Pts',(-50.,8.48553809038739,-4.7096313036054));
#42991=CARTESIAN_POINT('Ctrl Pts',(-50.,8.37904540061237,-4.70053505457754));
#42992=CARTESIAN_POINT('Ctrl Pts',(-50.,8.27357071338958,-4.68854644186826));
#42993=CARTESIAN_POINT('Ctrl Pts',(-50.,8.16923940463961,-4.67344942718086));
#42994=CARTESIAN_POINT('Ctrl Pts',(-50.,8.06622216356313,-4.65497254379874));
#42995=CARTESIAN_POINT('Ctrl Pts',(-50.,7.96474364136776,-4.63279116090914));
#42996=CARTESIAN_POINT('Ctrl Pts',(-50.,7.86510693532357,-4.60651043379445));
#42997=CARTESIAN_POINT('Ctrl Pts',(-50.,7.76764978894924,-4.57573041296856));
#42998=CARTESIAN_POINT('Ctrl Pts',(-50.,7.67266173023884,-4.54015728109748));
#42999=CARTESIAN_POINT('Ctrl Pts',(-50.,7.58030833791389,-4.49970799818987));
#43000=CARTESIAN_POINT('Ctrl Pts',(-50.,7.4905613596596,-4.4546048093515));
#43001=CARTESIAN_POINT('Ctrl Pts',(-50.,7.40310045604506,-4.40551298397998));
#43002=CARTESIAN_POINT('Ctrl Pts',(-50.,7.31737285380592,-4.35344239064242));
#43003=CARTESIAN_POINT('Ctrl Pts',(-50.,7.23270963259088,-4.29956476038277));
#43004=CARTESIAN_POINT('Ctrl Pts',(-50.,7.148424582012,-4.24505661346796));
#43005=CARTESIAN_POINT('Ctrl Pts',(-50.,7.06391513395684,-4.19093976616563));
#43006=CARTESIAN_POINT('Ctrl Pts',(-50.,6.97877527429846,-4.1379019406034));
#43007=CARTESIAN_POINT('Ctrl Pts',(-50.,6.89276821217244,-4.08634440644098));
#43008=CARTESIAN_POINT('Ctrl Pts',(-50.,6.82317593222513,-4.04643989396096));
#43009=CARTESIAN_POINT('Ctrl Pts',(-50.,6.77052326328196,-4.01729317493961));
#43010=CARTESIAN_POINT('Ctrl Pts',(-50.,6.73521797398851,-3.99820900830411));
#43011=CARTESIAN_POINT('Ctrl Pts',(-50.,6.71751445306827,-3.98875366785402));
#43012=CARTESIAN_POINT('Origin',(-50.,7.96777298730851,-5.18432547646766));
#43013=CARTESIAN_POINT('Origin',(-50.,0.,0.));
#43014=CARTESIAN_POINT('Origin',(-65.75,0.,0.));
#43015=CARTESIAN_POINT('',(-65.5,6.82112595358204,-8.14634063401289));
#43016=CARTESIAN_POINT('Origin',(-65.5,0.,0.));
#43017=CARTESIAN_POINT('',(-66.,6.26496857389735,-7.95397974400731));
#43018=CARTESIAN_POINT('Ctrl Pts',(-65.5,6.82112595358203,-8.14634063401289));
#43019=CARTESIAN_POINT('Ctrl Pts',(-65.6642917360004,6.6306718741513,-8.09153216836031));
#43020=CARTESIAN_POINT('Ctrl Pts',(-65.831118235484,6.44452864243079,-8.02752653417561));
#43021=CARTESIAN_POINT('Ctrl Pts',(-66.,6.26496857389735,-7.95397974400731));
#43022=CARTESIAN_POINT('Origin',(-66.,0.,0.));
#43023=CARTESIAN_POINT('Origin',(-58.,0.,0.));
#43024=CARTESIAN_POINT('',(-50.5,6.82112595358204,-8.14634063401289));
#43025=CARTESIAN_POINT('Origin',(-50.5,0.,0.));
#43026=CARTESIAN_POINT('Ctrl Pts',(-50.5,6.82112595358204,-8.14634063401289));
#43027=CARTESIAN_POINT('Ctrl Pts',(-55.5,6.82112595358204,-8.14634063401289));
#43028=CARTESIAN_POINT('Ctrl Pts',(-60.5,6.82112595358204,-8.14634063401289));
#43029=CARTESIAN_POINT('Ctrl Pts',(-65.5,6.82112595358204,-8.14634063401289));
#43030=CARTESIAN_POINT('Origin',(-50.25,0.,0.));
#43031=CARTESIAN_POINT('',(-50.,6.26496857389736,-7.95397974400732));
#43032=CARTESIAN_POINT('Origin',(-50.,0.,0.));
#43033=CARTESIAN_POINT('Ctrl Pts',(-50.,6.26496857389736,-7.95397974400732));
#43034=CARTESIAN_POINT('Ctrl Pts',(-50.168881764515,6.44452864242976,-8.02752653417518));
#43035=CARTESIAN_POINT('Ctrl Pts',(-50.3357082639993,6.63067187415095,-8.09153216836019));
#43036=CARTESIAN_POINT('Ctrl Pts',(-50.5,6.82112595358205,-8.14634063401289));
#43037=CARTESIAN_POINT('Origin',(-66.,5.1702676791723,-7.97690222761574));
#43038=CARTESIAN_POINT('',(-66.,3.76836956336765,-9.39760692058804));
#43039=CARTESIAN_POINT('Origin',(-66.,0.,0.));
#43040=CARTESIAN_POINT('',(-66.,4.5143825383298,-6.37616707337747));
#43041=CARTESIAN_POINT('Ctrl Pts',(-66.,4.51438253832981,-6.37616707337746));
#43042=CARTESIAN_POINT('Ctrl Pts',(-66.,4.52670967601697,-6.39200562736583));
#43043=CARTESIAN_POINT('Ctrl Pts',(-66.,4.55120043280854,-6.42379983595862));
#43044=CARTESIAN_POINT('Ctrl Pts',(-66.,4.58744600070291,-6.47184245854068));
#43045=CARTESIAN_POINT('Ctrl Pts',(-66.,4.63479108448607,-6.53660277498602));
#43046=CARTESIAN_POINT('Ctrl Pts',(-66.,4.69239210704599,-6.61868514985729));
#43047=CARTESIAN_POINT('Ctrl Pts',(-66.,4.74859881197601,-6.7017671151923));
#43048=CARTESIAN_POINT('Ctrl Pts',(-66.,4.80379072956909,-6.78557840443743));
#43049=CARTESIAN_POINT('Ctrl Pts',(-66.,4.85861849397619,-6.86965589298989));
#43050=CARTESIAN_POINT('Ctrl Pts',(-66.,4.91404818867789,-6.95331119177114));
#43051=CARTESIAN_POINT('Ctrl Pts',(-66.,4.97118523196097,-7.03574860294511));
#43052=CARTESIAN_POINT('Ctrl Pts',(-66.,5.03111729892527,-7.1161697713572));
#43053=CARTESIAN_POINT('Ctrl Pts',(-66.,5.09476012362649,-7.19387696930703));
#43054=CARTESIAN_POINT('Ctrl Pts',(-66.,5.16267694013817,-7.26839273674309));
#43055=CARTESIAN_POINT('Ctrl Pts',(-66.,5.23498395346241,-7.33952553391019));
#43056=CARTESIAN_POINT('Ctrl Pts',(-66.,5.31149612450297,-7.40728387468187));
#43057=CARTESIAN_POINT('Ctrl Pts',(-66.,5.39182944999988,-7.47181841290458));
#43058=CARTESIAN_POINT('Ctrl Pts',(-66.,5.47551271178446,-7.53335714794964));
#43059=CARTESIAN_POINT('Ctrl Pts',(-66.,5.5621084189074,-7.59213750764915));
#43060=CARTESIAN_POINT('Ctrl Pts',(-66.,5.65127930303142,-7.64836468312946));
#43061=CARTESIAN_POINT('Ctrl Pts',(-66.,5.74275901635157,-7.70221724602392));
#43062=CARTESIAN_POINT('Ctrl Pts',(-66.,5.83634515157351,-7.75384156215611));
#43063=CARTESIAN_POINT('Ctrl Pts',(-66.,5.93188366426367,-7.80335138726874));
#43064=CARTESIAN_POINT('Ctrl Pts',(-66.,6.02925624926082,-7.85082401216739));
#43065=CARTESIAN_POINT('Ctrl Pts',(-66.,6.11544012502743,-7.89037004192436));
#43066=CARTESIAN_POINT('Ctrl Pts',(-66.,6.18273475869519,-7.91971356466277));
#43067=CARTESIAN_POINT('Ctrl Pts',(-66.,6.2303734034606,-7.93974831559927));
#43068=CARTESIAN_POINT('Ctrl Pts',(-66.,6.25786529949277,-7.95107028292051));
#43069=CARTESIAN_POINT('Ctrl Pts',(-66.,6.26496857389735,-7.95397974400731));
#43070=CARTESIAN_POINT('',(-66.,3.26473139515385,-7.09765349728322));
#43071=CARTESIAN_POINT('Origin',(-66.,0.,0.));
#43072=CARTESIAN_POINT('Ctrl Pts',(-66.,3.76836956336765,-9.39760692058804));
#43073=CARTESIAN_POINT('Ctrl Pts',(-66.,3.77192378760531,-9.37803748530914));
#43074=CARTESIAN_POINT('Ctrl Pts',(-66.,3.77947496961539,-9.33209763417661));
#43075=CARTESIAN_POINT('Ctrl Pts',(-66.,3.78814720834319,-9.26139904172235));
#43076=CARTESIAN_POINT('Ctrl Pts',(-66.,3.79381050973993,-9.168159472417));
#43077=CARTESIAN_POINT('Ctrl Pts',(-66.,3.79437267711955,-9.05291824039091));
#43078=CARTESIAN_POINT('Ctrl Pts',(-66.,3.79293549112385,-8.93064918094144));
#43079=CARTESIAN_POINT('Ctrl Pts',(-66.,3.79214634580768,-8.8060610382747));
#43080=CARTESIAN_POINT('Ctrl Pts',(-66.,3.79133013838023,-8.67954430710504));
#43081=CARTESIAN_POINT('Ctrl Pts',(-66.,3.78814329632398,-8.5526379490841));
#43082=CARTESIAN_POINT('Ctrl Pts',(-66.,3.77955877175069,-8.42736119058854));
#43083=CARTESIAN_POINT('Ctrl Pts',(-66.,3.76328700746442,-8.30524256603013));
#43084=CARTESIAN_POINT('Ctrl Pts',(-66.,3.73850464063369,-8.18683427877518));
#43085=CARTESIAN_POINT('Ctrl Pts',(-66.,3.70540363987127,-8.07205943796329));
#43086=CARTESIAN_POINT('Ctrl Pts',(-66.,3.66498426083752,-7.96038432184111));
#43087=CARTESIAN_POINT('Ctrl Pts',(-66.,3.61875289573396,-7.85106692396409));
#43088=CARTESIAN_POINT('Ctrl Pts',(-66.,3.56847706424299,-7.74334074205051));
#43089=CARTESIAN_POINT('Ctrl Pts',(-66.,3.51597837414158,-7.63646478182881));
#43090=CARTESIAN_POINT('Ctrl Pts',(-66.,3.46293063930599,-7.52978780875129));
#43091=CARTESIAN_POINT('Ctrl Pts',(-66.,3.41064498168427,-7.42281101590317));
#43092=CARTESIAN_POINT('Ctrl Pts',(-66.,3.359888780788,-7.31524215598795));
#43093=CARTESIAN_POINT('Ctrl Pts',(-66.,3.32081146957076,-7.22859771080324));
#43094=CARTESIAN_POINT('Ctrl Pts',(-66.,3.29241670612082,-7.16326234391299));
#43095=CARTESIAN_POINT('Ctrl Pts',(-66.,3.27389226747348,-7.11954915773029));
#43096=CARTESIAN_POINT('Ctrl Pts',(-66.,3.26473139515385,-7.09765349728322));
#43097=CARTESIAN_POINT('Ctrl Pts',(-66.,3.26473139515385,-7.09765349728322));
#43098=CARTESIAN_POINT('Ctrl Pts',(-50.,3.26473139515385,-7.09765349728322));
#43099=CARTESIAN_POINT('Ctrl Pts',(-66.,3.27389226747348,-7.11954915773029));
#43100=CARTESIAN_POINT('Ctrl Pts',(-50.,3.27389226747348,-7.11954915773029));
#43101=CARTESIAN_POINT('Ctrl Pts',(-66.,3.29241670612082,-7.16326234391299));
#43102=CARTESIAN_POINT('Ctrl Pts',(-50.,3.29241670612082,-7.16326234391299));
#43103=CARTESIAN_POINT('Ctrl Pts',(-66.,3.32081146957076,-7.22859771080324));
#43104=CARTESIAN_POINT('Ctrl Pts',(-50.,3.32081146957076,-7.22859771080324));
#43105=CARTESIAN_POINT('Ctrl Pts',(-66.,3.359888780788,-7.31524215598795));
#43106=CARTESIAN_POINT('Ctrl Pts',(-50.,3.359888780788,-7.31524215598795));
#43107=CARTESIAN_POINT('Ctrl Pts',(-66.,3.41064498168427,-7.42281101590317));
#43108=CARTESIAN_POINT('Ctrl Pts',(-50.,3.41064498168427,-7.42281101590317));
#43109=CARTESIAN_POINT('Ctrl Pts',(-66.,3.46293063930599,-7.52978780875129));
#43110=CARTESIAN_POINT('Ctrl Pts',(-50.,3.46293063930599,-7.52978780875129));
#43111=CARTESIAN_POINT('Ctrl Pts',(-66.,3.51597837414158,-7.63646478182881));
#43112=CARTESIAN_POINT('Ctrl Pts',(-50.,3.51597837414158,-7.63646478182881));
#43113=CARTESIAN_POINT('Ctrl Pts',(-66.,3.56847706424299,-7.74334074205051));
#43114=CARTESIAN_POINT('Ctrl Pts',(-50.,3.56847706424299,-7.74334074205051));
#43115=CARTESIAN_POINT('Ctrl Pts',(-66.,3.61875289573396,-7.85106692396409));
#43116=CARTESIAN_POINT('Ctrl Pts',(-50.,3.61875289573396,-7.85106692396409));
#43117=CARTESIAN_POINT('Ctrl Pts',(-66.,3.66498426083752,-7.96038432184111));
#43118=CARTESIAN_POINT('Ctrl Pts',(-50.,3.66498426083752,-7.96038432184111));
#43119=CARTESIAN_POINT('Ctrl Pts',(-66.,3.70540363987127,-8.07205943796329));
#43120=CARTESIAN_POINT('Ctrl Pts',(-50.,3.70540363987127,-8.07205943796329));
#43121=CARTESIAN_POINT('Ctrl Pts',(-66.,3.73850464063369,-8.18683427877518));
#43122=CARTESIAN_POINT('Ctrl Pts',(-50.,3.73850464063369,-8.18683427877518));
#43123=CARTESIAN_POINT('Ctrl Pts',(-66.,3.76328700746442,-8.30524256603013));
#43124=CARTESIAN_POINT('Ctrl Pts',(-50.,3.76328700746442,-8.30524256603013));
#43125=CARTESIAN_POINT('Ctrl Pts',(-66.,3.77955877175069,-8.42736119058854));
#43126=CARTESIAN_POINT('Ctrl Pts',(-50.,3.77955877175069,-8.42736119058854));
#43127=CARTESIAN_POINT('Ctrl Pts',(-66.,3.78814329632398,-8.5526379490841));
#43128=CARTESIAN_POINT('Ctrl Pts',(-50.,3.78814329632398,-8.5526379490841));
#43129=CARTESIAN_POINT('Ctrl Pts',(-66.,3.79133013838023,-8.67954430710504));
#43130=CARTESIAN_POINT('Ctrl Pts',(-50.,3.79133013838023,-8.67954430710504));
#43131=CARTESIAN_POINT('Ctrl Pts',(-66.,3.79214634580768,-8.8060610382747));
#43132=CARTESIAN_POINT('Ctrl Pts',(-50.,3.79214634580768,-8.8060610382747));
#43133=CARTESIAN_POINT('Ctrl Pts',(-66.,3.79293549112385,-8.93064918094144));
#43134=CARTESIAN_POINT('Ctrl Pts',(-50.,3.79293549112385,-8.93064918094144));
#43135=CARTESIAN_POINT('Ctrl Pts',(-66.,3.79437267711955,-9.05291824039091));
#43136=CARTESIAN_POINT('Ctrl Pts',(-50.,3.79437267711955,-9.05291824039091));
#43137=CARTESIAN_POINT('Ctrl Pts',(-66.,3.79377821827189,-9.17477904640165));
#43138=CARTESIAN_POINT('Ctrl Pts',(-50.,3.79377821827189,-9.17477904640165));
#43139=CARTESIAN_POINT('Ctrl Pts',(-66.,3.78567343749225,-9.30005041156712));
#43140=CARTESIAN_POINT('Ctrl Pts',(-50.,3.78567343749225,-9.30005041156712));
#43141=CARTESIAN_POINT('Ctrl Pts',(-66.,3.76494029563125,-9.43227003517924));
#43142=CARTESIAN_POINT('Ctrl Pts',(-50.,3.76494029563125,-9.43227003517924));
#43143=CARTESIAN_POINT('Ctrl Pts',(-66.,3.72915055981728,-9.57307911626445));
#43144=CARTESIAN_POINT('Ctrl Pts',(-50.,3.72915055981728,-9.57307911626445));
#43145=CARTESIAN_POINT('Ctrl Pts',(-66.,3.68158234815922,-9.72013034647482));
#43146=CARTESIAN_POINT('Ctrl Pts',(-50.,3.68158234815922,-9.72013034647482));
#43147=CARTESIAN_POINT('Ctrl Pts',(-66.,3.63295761578166,-9.86588553826929));
#43148=CARTESIAN_POINT('Ctrl Pts',(-50.,3.63295761578166,-9.86588553826929));
#43149=CARTESIAN_POINT('Ctrl Pts',(-66.,3.59837801318299,-9.99975571673022));
#43150=CARTESIAN_POINT('Ctrl Pts',(-50.,3.59837801318299,-9.99975571673022));
#43151=CARTESIAN_POINT('Ctrl Pts',(-66.,3.59492345335028,-10.1097801578306));
#43152=CARTESIAN_POINT('Ctrl Pts',(-50.,3.59492345335028,-10.1097801578306));
#43153=CARTESIAN_POINT('Ctrl Pts',(-66.,3.63910068308438,-10.1844096267491));
#43154=CARTESIAN_POINT('Ctrl Pts',(-50.,3.63910068308438,-10.1844096267491));
#43155=CARTESIAN_POINT('Ctrl Pts',(-66.,3.74410743433881,-10.2144193799856));
#43156=CARTESIAN_POINT('Ctrl Pts',(-50.,3.74410743433881,-10.2144193799856));
#43157=CARTESIAN_POINT('Ctrl Pts',(-66.,3.91997031954292,-10.1928102876364));
#43158=CARTESIAN_POINT('Ctrl Pts',(-50.,3.91997031954292,-10.1928102876364));
#43159=CARTESIAN_POINT('Ctrl Pts',(-66.,4.17408991345905,-10.1144251596098));
#43160=CARTESIAN_POINT('Ctrl Pts',(-50.,4.17408991345905,-10.1144251596098));
#43161=CARTESIAN_POINT('Ctrl Pts',(-66.,4.51161767757899,-9.97568294432114));
#43162=CARTESIAN_POINT('Ctrl Pts',(-50.,4.51161767757899,-9.97568294432114));
#43163=CARTESIAN_POINT('Ctrl Pts',(-66.,4.93588146508917,-9.77427910338594));
#43164=CARTESIAN_POINT('Ctrl Pts',(-50.,4.93588146508917,-9.77427910338594));
#43165=CARTESIAN_POINT('Ctrl Pts',(-66.,5.44876930769742,-9.50891534935813));
#43166=CARTESIAN_POINT('Ctrl Pts',(-50.,5.44876930769742,-9.50891534935813));
#43167=CARTESIAN_POINT('Ctrl Pts',(-66.,6.05111211183155,-9.17903030421983));
#43168=CARTESIAN_POINT('Ctrl Pts',(-50.,6.05111211183155,-9.17903030421983));
#43169=CARTESIAN_POINT('Ctrl Pts',(-66.,6.60466213719626,-8.8634396634983));
#43170=CARTESIAN_POINT('Ctrl Pts',(-50.,6.60466213719626,-8.8634396634983));
#43171=CARTESIAN_POINT('Ctrl Pts',(-66.,7.06005528277866,-8.59774076286258));
#43172=CARTESIAN_POINT('Ctrl Pts',(-50.,7.06005528277866,-8.59774076286258));
#43173=CARTESIAN_POINT('Ctrl Pts',(-66.,7.38150722208893,-8.40773377987118));
#43174=CARTESIAN_POINT('Ctrl Pts',(-50.,7.38150722208893,-8.40773377987118));
#43175=CARTESIAN_POINT('Ctrl Pts',(-66.,7.54669732025447,-8.30951169181823));
#43176=CARTESIAN_POINT('Ctrl Pts',(-50.,7.54669732025447,-8.30951169181823));
#43177=CARTESIAN_POINT('',(-65.5,3.6060757177882,-9.99434054440704));
#43178=CARTESIAN_POINT('Ctrl Pts',(-66.,3.76836956336765,-9.39760692058804));
#43179=CARTESIAN_POINT('Ctrl Pts',(-65.7982417703062,3.7257885904294,-9.63205627952235));
#43180=CARTESIAN_POINT('Ctrl Pts',(-65.6331946192803,3.62768025600023,-9.84494595215163));
#43181=CARTESIAN_POINT('Ctrl Pts',(-65.5,3.6060757177882,-9.99434054440703));
#43182=CARTESIAN_POINT('',(-50.,3.26473139515385,-7.09765349728322));
#43183=CARTESIAN_POINT('',(-66.,3.26473139515385,-7.09765349728322));
#43184=CARTESIAN_POINT('',(-50.,3.76836956336765,-9.39760692058806));
#43185=CARTESIAN_POINT('Ctrl Pts',(-50.,3.26473139515385,-7.09765349728322));
#43186=CARTESIAN_POINT('Ctrl Pts',(-50.,3.27389226747348,-7.11954915773029));
#43187=CARTESIAN_POINT('Ctrl Pts',(-50.,3.29241670612082,-7.16326234391299));
#43188=CARTESIAN_POINT('Ctrl Pts',(-50.,3.32081146957076,-7.22859771080324));
#43189=CARTESIAN_POINT('Ctrl Pts',(-50.,3.359888780788,-7.31524215598795));
#43190=CARTESIAN_POINT('Ctrl Pts',(-50.,3.41064498168427,-7.42281101590317));
#43191=CARTESIAN_POINT('Ctrl Pts',(-50.,3.46293063930599,-7.52978780875129));
#43192=CARTESIAN_POINT('Ctrl Pts',(-50.,3.51597837414158,-7.63646478182881));
#43193=CARTESIAN_POINT('Ctrl Pts',(-50.,3.56847706424299,-7.74334074205051));
#43194=CARTESIAN_POINT('Ctrl Pts',(-50.,3.61875289573396,-7.85106692396409));
#43195=CARTESIAN_POINT('Ctrl Pts',(-50.,3.66498426083752,-7.96038432184111));
#43196=CARTESIAN_POINT('Ctrl Pts',(-50.,3.70540363987127,-8.07205943796329));
#43197=CARTESIAN_POINT('Ctrl Pts',(-50.,3.73850464063369,-8.18683427877518));
#43198=CARTESIAN_POINT('Ctrl Pts',(-50.,3.76328700746442,-8.30524256603013));
#43199=CARTESIAN_POINT('Ctrl Pts',(-50.,3.77955877175069,-8.42736119058854));
#43200=CARTESIAN_POINT('Ctrl Pts',(-50.,3.78814329632398,-8.5526379490841));
#43201=CARTESIAN_POINT('Ctrl Pts',(-50.,3.79133013838023,-8.67954430710504));
#43202=CARTESIAN_POINT('Ctrl Pts',(-50.,3.79214634580768,-8.8060610382747));
#43203=CARTESIAN_POINT('Ctrl Pts',(-50.,3.79293549112385,-8.93064918094144));
#43204=CARTESIAN_POINT('Ctrl Pts',(-50.,3.79437267711955,-9.05291824039091));
#43205=CARTESIAN_POINT('Ctrl Pts',(-50.,3.79381050973993,-9.168159472417));
#43206=CARTESIAN_POINT('Ctrl Pts',(-50.,3.78814720834319,-9.26139904172235));
#43207=CARTESIAN_POINT('Ctrl Pts',(-50.,3.77947496961539,-9.33209763417662));
#43208=CARTESIAN_POINT('Ctrl Pts',(-50.,3.77192378760531,-9.37803748530916));
#43209=CARTESIAN_POINT('Ctrl Pts',(-50.,3.76836956336765,-9.39760692058806));
#43210=CARTESIAN_POINT('',(-50.5,3.6060757177882,-9.99434054440704));
#43211=CARTESIAN_POINT('Ctrl Pts',(-50.5,3.6060757177882,-9.99434054440705));
#43212=CARTESIAN_POINT('Ctrl Pts',(-50.4982567069814,3.60635848477112,-9.99238522105314));
#43213=CARTESIAN_POINT('Ctrl Pts',(-50.496511343879,3.60665306382448,-9.99042330533535));
#43214=CARTESIAN_POINT('Ctrl Pts',(-50.3581212730812,3.63088681363861,-9.83453533000683));
#43215=CARTESIAN_POINT('Ctrl Pts',(-50.2022201285476,3.72569110690851,-9.63259302040446));
#43216=CARTESIAN_POINT('Ctrl Pts',(-50.,3.76836956336765,-9.39760692058806));
#43217=CARTESIAN_POINT('Ctrl Pts',(-65.5,3.6060757177882,-9.99434054440703));
#43218=CARTESIAN_POINT('Ctrl Pts',(-60.5,3.6060757177882,-9.99434054440703));
#43219=CARTESIAN_POINT('Ctrl Pts',(-55.5,3.6060757177882,-9.99434054440704));
#43220=CARTESIAN_POINT('Ctrl Pts',(-50.5,3.6060757177882,-9.99434054440704));
#43221=CARTESIAN_POINT('Origin',(-66.,0.,0.));
#43222=CARTESIAN_POINT('',(-50.,4.5143825383298,-6.37616707337747));
#43223=CARTESIAN_POINT('',(-66.,4.5143825383298,-6.37616707337747));
#43224=CARTESIAN_POINT('Origin',(-50.,0.,0.));
#43225=CARTESIAN_POINT('Ctrl Pts',(-66.,7.54669732025447,-8.30951169181823));
#43226=CARTESIAN_POINT('Ctrl Pts',(-50.,7.54669732025447,-8.30951169181823));
#43227=CARTESIAN_POINT('Ctrl Pts',(-66.,7.52333157969776,-8.30560656273532));
#43228=CARTESIAN_POINT('Ctrl Pts',(-50.,7.52333157969776,-8.30560656273532));
#43229=CARTESIAN_POINT('Ctrl Pts',(-66.,7.47670872115481,-8.29761250101419));
#43230=CARTESIAN_POINT('Ctrl Pts',(-50.,7.47670872115481,-8.29761250101419));
#43231=CARTESIAN_POINT('Ctrl Pts',(-66.,7.4071003012639,-8.28506999791136));
#43232=CARTESIAN_POINT('Ctrl Pts',(-50.,7.4071003012639,-8.28506999791136));
#43233=CARTESIAN_POINT('Ctrl Pts',(-66.,7.31494167541519,-8.26724237158035));
#43234=CARTESIAN_POINT('Ctrl Pts',(-50.,7.31494167541519,-8.26724237158035));
#43235=CARTESIAN_POINT('Ctrl Pts',(-66.,7.20083933184586,-8.24310753334095));
#43236=CARTESIAN_POINT('Ctrl Pts',(-50.,7.20083933184586,-8.24310753334095));
#43237=CARTESIAN_POINT('Ctrl Pts',(-66.,7.0878489571346,-8.21710771481861));
#43238=CARTESIAN_POINT('Ctrl Pts',(-50.,7.0878489571346,-8.21710771481861));
#43239=CARTESIAN_POINT('Ctrl Pts',(-66.,6.97599606044936,-8.18922484372218));
#43240=CARTESIAN_POINT('Ctrl Pts',(-50.,6.97599606044936,-8.18922484372218));
#43241=CARTESIAN_POINT('Ctrl Pts',(-66.,6.8653170030208,-8.15943901382578));
#43242=CARTESIAN_POINT('Ctrl Pts',(-50.,6.8653170030208,-8.15943901382578));
#43243=CARTESIAN_POINT('Ctrl Pts',(-66.,6.75586105705924,-8.12773028115812));
#43244=CARTESIAN_POINT('Ctrl Pts',(-50.,6.75586105705924,-8.12773028115812));
#43245=CARTESIAN_POINT('Ctrl Pts',(-66.,6.64768765206965,-8.09407995465062));
#43246=CARTESIAN_POINT('Ctrl Pts',(-50.,6.64768765206965,-8.09407995465062));
#43247=CARTESIAN_POINT('Ctrl Pts',(-66.,6.54086250417151,-8.05847172269461));
#43248=CARTESIAN_POINT('Ctrl Pts',(-50.,6.54086250417151,-8.05847172269461));
#43249=CARTESIAN_POINT('Ctrl Pts',(-66.,6.43545373939148,-8.02089334946028));
#43250=CARTESIAN_POINT('Ctrl Pts',(-50.,6.43545373939148,-8.02089334946028));
#43251=CARTESIAN_POINT('Ctrl Pts',(-66.,6.33152851820538,-7.98133773872331));
#43252=CARTESIAN_POINT('Ctrl Pts',(-50.,6.33152851820538,-7.98133773872331));
#43253=CARTESIAN_POINT('Ctrl Pts',(-66.,6.22914767586739,-7.93980615319185));
#43254=CARTESIAN_POINT('Ctrl Pts',(-50.,6.22914767586739,-7.93980615319185));
#43255=CARTESIAN_POINT('Ctrl Pts',(-66.,6.12836917819085,-7.89630262173216));
#43256=CARTESIAN_POINT('Ctrl Pts',(-50.,6.12836917819085,-7.89630262173216));
#43257=CARTESIAN_POINT('Ctrl Pts',(-66.,6.02925624926082,-7.85082401216739));
#43258=CARTESIAN_POINT('Ctrl Pts',(-50.,6.02925624926082,-7.85082401216739));
#43259=CARTESIAN_POINT('Ctrl Pts',(-66.,5.93188366426367,-7.80335138726874));
#43260=CARTESIAN_POINT('Ctrl Pts',(-50.,5.93188366426367,-7.80335138726874));
#43261=CARTESIAN_POINT('Ctrl Pts',(-66.,5.83634515157351,-7.75384156215611));
#43262=CARTESIAN_POINT('Ctrl Pts',(-50.,5.83634515157351,-7.75384156215611));
#43263=CARTESIAN_POINT('Ctrl Pts',(-66.,5.74275901635157,-7.70221724602392));
#43264=CARTESIAN_POINT('Ctrl Pts',(-50.,5.74275901635157,-7.70221724602392));
#43265=CARTESIAN_POINT('Ctrl Pts',(-66.,5.65127930303142,-7.64836468312946));
#43266=CARTESIAN_POINT('Ctrl Pts',(-50.,5.65127930303142,-7.64836468312946));
#43267=CARTESIAN_POINT('Ctrl Pts',(-66.,5.5621084189074,-7.59213750764915));
#43268=CARTESIAN_POINT('Ctrl Pts',(-50.,5.5621084189074,-7.59213750764915));
#43269=CARTESIAN_POINT('Ctrl Pts',(-66.,5.47551271178446,-7.53335714794964));
#43270=CARTESIAN_POINT('Ctrl Pts',(-50.,5.47551271178446,-7.53335714794964));
#43271=CARTESIAN_POINT('Ctrl Pts',(-66.,5.39182944999988,-7.47181841290458));
#43272=CARTESIAN_POINT('Ctrl Pts',(-50.,5.39182944999988,-7.47181841290458));
#43273=CARTESIAN_POINT('Ctrl Pts',(-66.,5.31149612450297,-7.40728387468187));
#43274=CARTESIAN_POINT('Ctrl Pts',(-50.,5.31149612450297,-7.40728387468187));
#43275=CARTESIAN_POINT('Ctrl Pts',(-66.,5.23498395346241,-7.33952553391019));
#43276=CARTESIAN_POINT('Ctrl Pts',(-50.,5.23498395346241,-7.33952553391019));
#43277=CARTESIAN_POINT('Ctrl Pts',(-66.,5.16267694013817,-7.26839273674309));
#43278=CARTESIAN_POINT('Ctrl Pts',(-50.,5.16267694013817,-7.26839273674309));
#43279=CARTESIAN_POINT('Ctrl Pts',(-66.,5.09476012362649,-7.19387696930703));
#43280=CARTESIAN_POINT('Ctrl Pts',(-50.,5.09476012362649,-7.19387696930703));
#43281=CARTESIAN_POINT('Ctrl Pts',(-66.,5.03111729892527,-7.1161697713572));
#43282=CARTESIAN_POINT('Ctrl Pts',(-50.,5.03111729892527,-7.1161697713572));
#43283=CARTESIAN_POINT('Ctrl Pts',(-66.,4.97118523196097,-7.03574860294511));
#43284=CARTESIAN_POINT('Ctrl Pts',(-50.,4.97118523196097,-7.03574860294511));
#43285=CARTESIAN_POINT('Ctrl Pts',(-66.,4.91404818867789,-6.95331119177114));
#43286=CARTESIAN_POINT('Ctrl Pts',(-50.,4.91404818867789,-6.95331119177114));
#43287=CARTESIAN_POINT('Ctrl Pts',(-66.,4.85861849397619,-6.86965589298989));
#43288=CARTESIAN_POINT('Ctrl Pts',(-50.,4.85861849397619,-6.86965589298989));
#43289=CARTESIAN_POINT('Ctrl Pts',(-66.,4.80379072956909,-6.78557840443743));
#43290=CARTESIAN_POINT('Ctrl Pts',(-50.,4.80379072956909,-6.78557840443743));
#43291=CARTESIAN_POINT('Ctrl Pts',(-66.,4.74859881197601,-6.7017671151923));
#43292=CARTESIAN_POINT('Ctrl Pts',(-50.,4.74859881197601,-6.7017671151923));
#43293=CARTESIAN_POINT('Ctrl Pts',(-66.,4.69239210704599,-6.61868514985729));
#43294=CARTESIAN_POINT('Ctrl Pts',(-50.,4.69239210704599,-6.61868514985729));
#43295=CARTESIAN_POINT('Ctrl Pts',(-66.,4.63479108448607,-6.53660277498602));
#43296=CARTESIAN_POINT('Ctrl Pts',(-50.,4.63479108448607,-6.53660277498602));
#43297=CARTESIAN_POINT('Ctrl Pts',(-66.,4.58744600070291,-6.47184245854068));
#43298=CARTESIAN_POINT('Ctrl Pts',(-50.,4.58744600070291,-6.47184245854068));
#43299=CARTESIAN_POINT('Ctrl Pts',(-66.,4.55120043280854,-6.42379983595862));
#43300=CARTESIAN_POINT('Ctrl Pts',(-50.,4.55120043280854,-6.42379983595862));
#43301=CARTESIAN_POINT('Ctrl Pts',(-66.,4.52670967601697,-6.39200562736583));
#43302=CARTESIAN_POINT('Ctrl Pts',(-50.,4.52670967601697,-6.39200562736583));
#43303=CARTESIAN_POINT('Ctrl Pts',(-66.,4.51438253832981,-6.37616707337746));
#43304=CARTESIAN_POINT('Ctrl Pts',(-50.,4.51438253832981,-6.37616707337746));
#43305=CARTESIAN_POINT('Ctrl Pts',(-50.,6.26496857389736,-7.95397974400732));
#43306=CARTESIAN_POINT('Ctrl Pts',(-50.,6.25786529949278,-7.95107028292052));
#43307=CARTESIAN_POINT('Ctrl Pts',(-50.,6.23037340346061,-7.93974831559927));
#43308=CARTESIAN_POINT('Ctrl Pts',(-50.,6.1827347586952,-7.91971356466277));
#43309=CARTESIAN_POINT('Ctrl Pts',(-50.,6.11544012502743,-7.89037004192437));
#43310=CARTESIAN_POINT('Ctrl Pts',(-50.,6.02925624926082,-7.85082401216739));
#43311=CARTESIAN_POINT('Ctrl Pts',(-50.,5.93188366426367,-7.80335138726874));
#43312=CARTESIAN_POINT('Ctrl Pts',(-50.,5.83634515157351,-7.75384156215611));
#43313=CARTESIAN_POINT('Ctrl Pts',(-50.,5.74275901635157,-7.70221724602392));
#43314=CARTESIAN_POINT('Ctrl Pts',(-50.,5.65127930303142,-7.64836468312946));
#43315=CARTESIAN_POINT('Ctrl Pts',(-50.,5.5621084189074,-7.59213750764915));
#43316=CARTESIAN_POINT('Ctrl Pts',(-50.,5.47551271178446,-7.53335714794964));
#43317=CARTESIAN_POINT('Ctrl Pts',(-50.,5.39182944999988,-7.47181841290458));
#43318=CARTESIAN_POINT('Ctrl Pts',(-50.,5.31149612450297,-7.40728387468187));
#43319=CARTESIAN_POINT('Ctrl Pts',(-50.,5.23498395346241,-7.33952553391019));
#43320=CARTESIAN_POINT('Ctrl Pts',(-50.,5.16267694013817,-7.26839273674309));
#43321=CARTESIAN_POINT('Ctrl Pts',(-50.,5.09476012362649,-7.19387696930703));
#43322=CARTESIAN_POINT('Ctrl Pts',(-50.,5.03111729892527,-7.1161697713572));
#43323=CARTESIAN_POINT('Ctrl Pts',(-50.,4.97118523196097,-7.03574860294511));
#43324=CARTESIAN_POINT('Ctrl Pts',(-50.,4.91404818867789,-6.95331119177114));
#43325=CARTESIAN_POINT('Ctrl Pts',(-50.,4.85861849397619,-6.86965589298989));
#43326=CARTESIAN_POINT('Ctrl Pts',(-50.,4.80379072956909,-6.78557840443743));
#43327=CARTESIAN_POINT('Ctrl Pts',(-50.,4.74859881197601,-6.7017671151923));
#43328=CARTESIAN_POINT('Ctrl Pts',(-50.,4.69239210704599,-6.61868514985729));
#43329=CARTESIAN_POINT('Ctrl Pts',(-50.,4.63479108448607,-6.53660277498602));
#43330=CARTESIAN_POINT('Ctrl Pts',(-50.,4.58744600070291,-6.47184245854068));
#43331=CARTESIAN_POINT('Ctrl Pts',(-50.,4.55120043280854,-6.42379983595862));
#43332=CARTESIAN_POINT('Ctrl Pts',(-50.,4.52670967601697,-6.39200562736583));
#43333=CARTESIAN_POINT('Ctrl Pts',(-50.,4.51438253832981,-6.37616707337746));
#43334=CARTESIAN_POINT('Origin',(-50.,5.1702676791723,-7.97690222761574));
#43335=CARTESIAN_POINT('Origin',(-50.,0.,0.));
#43336=CARTESIAN_POINT('Origin',(-65.75,0.,0.));
#43337=CARTESIAN_POINT('',(-65.5,2.91799338807253,-10.216454354969));
#43338=CARTESIAN_POINT('Origin',(-65.5,0.,0.));
#43339=CARTESIAN_POINT('',(-66.,2.48815856278711,-9.81451435204152));
#43340=CARTESIAN_POINT('Ctrl Pts',(-65.5,2.91799338807253,-10.216454354969));
#43341=CARTESIAN_POINT('Ctrl Pts',(-65.6642587837351,2.76632796613792,-10.0889452570453));
#43342=CARTESIAN_POINT('Ctrl Pts',(-65.8310681634032,2.62232043935157,-9.95477792232024));
#43343=CARTESIAN_POINT('Ctrl Pts',(-66.,2.48815856278711,-9.81451435204153));
#43344=CARTESIAN_POINT('Origin',(-66.,0.,0.));
#43345=CARTESIAN_POINT('Origin',(-58.,0.,0.));
#43346=CARTESIAN_POINT('',(-50.5,2.91799338807254,-10.216454354969));
#43347=CARTESIAN_POINT('Origin',(-50.5,0.,0.));
#43348=CARTESIAN_POINT('Ctrl Pts',(-50.5,2.91799338807254,-10.216454354969));
#43349=CARTESIAN_POINT('Ctrl Pts',(-55.5,2.91799338807254,-10.216454354969));
#43350=CARTESIAN_POINT('Ctrl Pts',(-60.5,2.91799338807253,-10.216454354969));
#43351=CARTESIAN_POINT('Ctrl Pts',(-65.5,2.91799338807253,-10.216454354969));
#43352=CARTESIAN_POINT('Origin',(-50.25,0.,0.));
#43353=CARTESIAN_POINT('',(-50.,2.48815856278712,-9.81451435204154));
#43354=CARTESIAN_POINT('Origin',(-50.,0.,0.));
#43355=CARTESIAN_POINT('Ctrl Pts',(-50.,2.48815856278713,-9.81451435204155));
#43356=CARTESIAN_POINT('Ctrl Pts',(-50.1689318365966,2.62232043935141,-9.95477792232008));
#43357=CARTESIAN_POINT('Ctrl Pts',(-50.3357412162647,2.76632796613773,-10.0889452570451));
#43358=CARTESIAN_POINT('Ctrl Pts',(-50.5,2.91799338807254,-10.216454354969));
#43359=CARTESIAN_POINT('Origin',(-66.,1.47877611889991,-9.39020011572736));
#43360=CARTESIAN_POINT('',(-66.,-0.37977419449274,-10.1178751010871));
#43361=CARTESIAN_POINT('Origin',(-66.,0.,0.));
#43362=CARTESIAN_POINT('',(-66.,1.53067287083626,-7.66108326625458));
#43363=CARTESIAN_POINT('Ctrl Pts',(-66.,1.53067287083627,-7.66108326625457));
#43364=CARTESIAN_POINT('Ctrl Pts',(-66.,1.53549215119571,-7.68056640390788));
#43365=CARTESIAN_POINT('Ctrl Pts',(-66.,1.54493370114459,-7.71957314695095));
#43366=CARTESIAN_POINT('Ctrl Pts',(-66.,1.55850498002059,-7.77820466719577));
#43367=CARTESIAN_POINT('Ctrl Pts',(-66.,1.5754164725369,-7.85662314056401));
#43368=CARTESIAN_POINT('Ctrl Pts',(-66.,1.59465171544125,-7.95503756783394));
#43369=CARTESIAN_POINT('Ctrl Pts',(-66.,1.61220661573863,-8.05379804635934));
#43370=CARTESIAN_POINT('Ctrl Pts',(-66.,1.62853781891495,-8.15281204423512));
#43371=CARTESIAN_POINT('Ctrl Pts',(-66.,1.64442807858968,-8.25192111283452));
#43372=CARTESIAN_POINT('Ctrl Pts',(-66.,1.66103994900115,-8.35088931899355));
#43373=CARTESIAN_POINT('Ctrl Pts',(-66.,1.67970691947077,-8.44943937069158));
#43374=CARTESIAN_POINT('Ctrl Pts',(-66.,1.70174735094098,-8.54728433152241));
#43375=CARTESIAN_POINT('Ctrl Pts',(-66.,1.72828159952138,-8.64415925811045));
#43376=CARTESIAN_POINT('Ctrl Pts',(-66.,1.76001840564001,-8.73985705693077));
#43377=CARTESIAN_POINT('Ctrl Pts',(-66.,1.79714183408573,-8.83425001254252));
#43378=CARTESIAN_POINT('Ctrl Pts',(-66.,1.83947938032835,-8.92727064057537));
#43379=CARTESIAN_POINT('Ctrl Pts',(-66.,1.88661896349422,-9.01890038196952));
#43380=CARTESIAN_POINT('Ctrl Pts',(-66.,1.93803736866688,-9.10915586281889));
#43381=CARTESIAN_POINT('Ctrl Pts',(-66.,1.99323835737743,-9.19807604064094));
#43382=CARTESIAN_POINT('Ctrl Pts',(-66.,2.05183036091841,-9.28571118746575));
#43383=CARTESIAN_POINT('Ctrl Pts',(-66.,2.11349742683576,-9.37211610318578));
#43384=CARTESIAN_POINT('Ctrl Pts',(-66.,2.17799511452139,-9.45734217317086));
#43385=CARTESIAN_POINT('Ctrl Pts',(-66.,2.24513642875384,-9.54143066294722));
#43386=CARTESIAN_POINT('Ctrl Pts',(-66.,2.31478185538763,-9.62440406213512));
#43387=CARTESIAN_POINT('Ctrl Pts',(-66.,2.37742992422592,-9.69558529830397));
#43388=CARTESIAN_POINT('Ctrl Pts',(-66.,2.4269715452022,-9.74976313360791));
#43389=CARTESIAN_POINT('Ctrl Pts',(-66.,2.46234274539511,-9.78744217177351));
#43390=CARTESIAN_POINT('Ctrl Pts',(-66.,2.48285278315603,-9.80896726509533));
#43391=CARTESIAN_POINT('Ctrl Pts',(-66.,2.48815856278711,-9.81451435204152));
#43392=CARTESIAN_POINT('',(-66.,0.0956047792657981,-7.81191500057326));
#43393=CARTESIAN_POINT('Origin',(-66.,0.,0.));
#43394=CARTESIAN_POINT('Ctrl Pts',(-66.,-0.37977419449274,-10.1178751010871));
#43395=CARTESIAN_POINT('Ctrl Pts',(-66.,-0.368567642672759,-10.1014431656146));
#43396=CARTESIAN_POINT('Ctrl Pts',(-66.,-0.342983873814566,-10.0625463657097));
#43397=CARTESIAN_POINT('Ctrl Pts',(-66.,-0.306305681352163,-10.0014873049795));
#43398=CARTESIAN_POINT('Ctrl Pts',(-66.,-0.263208048664822,-9.91861219216684));
#43399=CARTESIAN_POINT('Ctrl Pts',(-66.,-0.215821651350525,-9.8135627421891));
#43400=CARTESIAN_POINT('Ctrl Pts',(-66.,-0.167403279296175,-9.70127984211144));
#43401=CARTESIAN_POINT('Ctrl Pts',(-66.,-0.117449636499862,-9.58714193598532));
#43402=CARTESIAN_POINT('Ctrl Pts',(-66.,-0.0667362885588257,-9.47123116944039));
#43403=CARTESIAN_POINT('Ctrl Pts',(-66.,-0.0180301475971287,-9.35400023708443));
#43404=CARTESIAN_POINT('Ctrl Pts',(-66.,0.025082147178823,-9.23606258270527));
#43405=CARTESIAN_POINT('Ctrl Pts',(-66.,0.0598872702371897,-9.11788334516365));
#43406=CARTESIAN_POINT('Ctrl Pts',(-66.,0.0854084408597768,-8.99963209550245));
#43407=CARTESIAN_POINT('Ctrl Pts',(-66.,0.101852305431236,-8.88131667109455));
#43408=CARTESIAN_POINT('Ctrl Pts',(-66.,0.110349727160855,-8.76285633348602));
#43409=CARTESIAN_POINT('Ctrl Pts',(-66.,0.112578665012154,-8.64418593096713));
#43410=CARTESIAN_POINT('Ctrl Pts',(-66.,0.110465593127282,-8.52532414388232));
#43411=CARTESIAN_POINT('Ctrl Pts',(-66.,0.105976022539028,-8.40633495491286));
#43412=CARTESIAN_POINT('Ctrl Pts',(-66.,0.10090393926479,-8.28730423313303));
#43413=CARTESIAN_POINT('Ctrl Pts',(-66.,0.0966499958546681,-8.16830957709138));
#43414=CARTESIAN_POINT('Ctrl Pts',(-66.,0.0940340960600895,-8.04939612696421));
#43415=CARTESIAN_POINT('Ctrl Pts',(-66.,0.0935766666762872,-7.95434831325083));
#43416=CARTESIAN_POINT('Ctrl Pts',(-66.,0.094211047308826,-7.88311229483827));
#43417=CARTESIAN_POINT('Ctrl Pts',(-66.,0.0950678851332727,-7.8356437441717));
#43418=CARTESIAN_POINT('Ctrl Pts',(-66.,0.0956047792657981,-7.81191500057326));
#43419=CARTESIAN_POINT('Ctrl Pts',(-66.,0.0956047792657981,-7.81191500057326));
#43420=CARTESIAN_POINT('Ctrl Pts',(-50.,0.0956047792657981,-7.81191500057326));
#43421=CARTESIAN_POINT('Ctrl Pts',(-66.,0.0950678851332727,-7.8356437441717));
#43422=CARTESIAN_POINT('Ctrl Pts',(-50.,0.0950678851332727,-7.8356437441717));
#43423=CARTESIAN_POINT('Ctrl Pts',(-66.,0.094211047308826,-7.88311229483827));
#43424=CARTESIAN_POINT('Ctrl Pts',(-50.,0.094211047308826,-7.88311229483827));
#43425=CARTESIAN_POINT('Ctrl Pts',(-66.,0.0935766666762872,-7.95434831325083));
#43426=CARTESIAN_POINT('Ctrl Pts',(-50.,0.0935766666762872,-7.95434831325083));
#43427=CARTESIAN_POINT('Ctrl Pts',(-66.,0.0940340960600895,-8.04939612696421));
#43428=CARTESIAN_POINT('Ctrl Pts',(-50.,0.0940340960600895,-8.04939612696421));
#43429=CARTESIAN_POINT('Ctrl Pts',(-66.,0.0966499958546681,-8.16830957709138));
#43430=CARTESIAN_POINT('Ctrl Pts',(-50.,0.0966499958546681,-8.16830957709138));
#43431=CARTESIAN_POINT('Ctrl Pts',(-66.,0.10090393926479,-8.28730423313303));
#43432=CARTESIAN_POINT('Ctrl Pts',(-50.,0.10090393926479,-8.28730423313303));
#43433=CARTESIAN_POINT('Ctrl Pts',(-66.,0.105976022539028,-8.40633495491286));
#43434=CARTESIAN_POINT('Ctrl Pts',(-50.,0.105976022539028,-8.40633495491286));
#43435=CARTESIAN_POINT('Ctrl Pts',(-66.,0.110465593127282,-8.52532414388232));
#43436=CARTESIAN_POINT('Ctrl Pts',(-50.,0.110465593127282,-8.52532414388232));
#43437=CARTESIAN_POINT('Ctrl Pts',(-66.,0.112578665012154,-8.64418593096713));
#43438=CARTESIAN_POINT('Ctrl Pts',(-50.,0.112578665012154,-8.64418593096713));
#43439=CARTESIAN_POINT('Ctrl Pts',(-66.,0.110349727160855,-8.76285633348602));
#43440=CARTESIAN_POINT('Ctrl Pts',(-50.,0.110349727160855,-8.76285633348602));
#43441=CARTESIAN_POINT('Ctrl Pts',(-66.,0.101852305431236,-8.88131667109455));
#43442=CARTESIAN_POINT('Ctrl Pts',(-50.,0.101852305431236,-8.88131667109455));
#43443=CARTESIAN_POINT('Ctrl Pts',(-66.,0.0854084408597768,-8.99963209550245));
#43444=CARTESIAN_POINT('Ctrl Pts',(-50.,0.0854084408597768,-8.99963209550245));
#43445=CARTESIAN_POINT('Ctrl Pts',(-66.,0.0598872702371897,-9.11788334516365));
#43446=CARTESIAN_POINT('Ctrl Pts',(-50.,0.0598872702371897,-9.11788334516365));
#43447=CARTESIAN_POINT('Ctrl Pts',(-66.,0.025082147178823,-9.23606258270527));
#43448=CARTESIAN_POINT('Ctrl Pts',(-50.,0.025082147178823,-9.23606258270527));
#43449=CARTESIAN_POINT('Ctrl Pts',(-66.,-0.0180301475971287,-9.35400023708443));
#43450=CARTESIAN_POINT('Ctrl Pts',(-50.,-0.0180301475971287,-9.35400023708443));
#43451=CARTESIAN_POINT('Ctrl Pts',(-66.,-0.0667362885588257,-9.47123116944039));
#43452=CARTESIAN_POINT('Ctrl Pts',(-50.,-0.0667362885588257,-9.47123116944039));
#43453=CARTESIAN_POINT('Ctrl Pts',(-66.,-0.117449636499862,-9.58714193598532));
#43454=CARTESIAN_POINT('Ctrl Pts',(-50.,-0.117449636499862,-9.58714193598532));
#43455=CARTESIAN_POINT('Ctrl Pts',(-66.,-0.167403279296175,-9.70127984211144));
#43456=CARTESIAN_POINT('Ctrl Pts',(-50.,-0.167403279296175,-9.70127984211144));
#43457=CARTESIAN_POINT('Ctrl Pts',(-66.,-0.215821651350525,-9.8135627421891));
#43458=CARTESIAN_POINT('Ctrl Pts',(-50.,-0.215821651350525,-9.8135627421891));
#43459=CARTESIAN_POINT('Ctrl Pts',(-66.,-0.26592997168988,-9.92464633978874));
#43460=CARTESIAN_POINT('Ctrl Pts',(-50.,-0.26592997168988,-9.92464633978874));
#43461=CARTESIAN_POINT('Ctrl Pts',(-66.,-0.324286511897233,-10.0357909150812));
#43462=CARTESIAN_POINT('Ctrl Pts',(-50.,-0.324286511897233,-10.0357909150812));
#43463=CARTESIAN_POINT('Ctrl Pts',(-66.,-0.39700574532375,-10.1481466231223));
#43464=CARTESIAN_POINT('Ctrl Pts',(-50.,-0.39700574532375,-10.1481466231223));
#43465=CARTESIAN_POINT('Ctrl Pts',(-66.,-0.486973508862013,-10.262225122541));
#43466=CARTESIAN_POINT('Ctrl Pts',(-50.,-0.486973508862013,-10.262225122541));
#43467=CARTESIAN_POINT('Ctrl Pts',(-66.,-0.590240356286357,-10.3772153712135));
#43468=CARTESIAN_POINT('Ctrl Pts',(-50.,-0.590240356286357,-10.3772153712135));
#43469=CARTESIAN_POINT('Ctrl Pts',(-66.,-0.693945237100309,-10.4905919041874));
#43470=CARTESIAN_POINT('Ctrl Pts',(-50.,-0.693945237100309,-10.4905919041874));
#43471=CARTESIAN_POINT('Ctrl Pts',(-66.,-0.779985182976566,-10.5988236061543));
#43472=CARTESIAN_POINT('Ctrl Pts',(-50.,-0.779985182976566,-10.5988236061543));
#43473=CARTESIAN_POINT('Ctrl Pts',(-66.,-0.827892052249358,-10.6979308384816));
#43474=CARTESIAN_POINT('Ctrl Pts',(-50.,-0.827892052249358,-10.6979308384816));
#43475=CARTESIAN_POINT('Ctrl Pts',(-66.,-0.817888684356991,-10.7840767489408));
#43476=CARTESIAN_POINT('Ctrl Pts',(-50.,-0.817888684356991,-10.7840767489408));
#43477=CARTESIAN_POINT('Ctrl Pts',(-66.,-0.734166310017649,-10.8542021162005));
#43478=CARTESIAN_POINT('Ctrl Pts',(-50.,-0.734166310017649,-10.8542021162005));
#43479=CARTESIAN_POINT('Ctrl Pts',(-66.,-0.564718360389463,-10.9059911076107));
#43480=CARTESIAN_POINT('Ctrl Pts',(-50.,-0.564718360389463,-10.9059911076107));
#43481=CARTESIAN_POINT('Ctrl Pts',(-66.,-0.300686455828779,-10.9377424805244));
#43482=CARTESIAN_POINT('Ctrl Pts',(-50.,-0.300686455828779,-10.9377424805244));
#43483=CARTESIAN_POINT('Ctrl Pts',(-66.,0.0640920428106455,-10.9482800696873));
#43484=CARTESIAN_POINT('Ctrl Pts',(-50.,0.0640920428106455,-10.9482800696873));
#43485=CARTESIAN_POINT('Ctrl Pts',(-66.,0.533594620897368,-10.9368521343596));
#43486=CARTESIAN_POINT('Ctrl Pts',(-50.,0.533594620897368,-10.9368521343596));
#43487=CARTESIAN_POINT('Ctrl Pts',(-66.,1.11007414229951,-10.9030405616214));
#43488=CARTESIAN_POINT('Ctrl Pts',(-50.,1.11007414229951,-10.9030405616214));
#43489=CARTESIAN_POINT('Ctrl Pts',(-66.,1.79451801082041,-10.8466704672255));
#43490=CARTESIAN_POINT('Ctrl Pts',(-50.,1.79451801082041,-10.8466704672255));
#43491=CARTESIAN_POINT('Ctrl Pts',(-66.,2.42857339986351,-10.7835131500112));
#43492=CARTESIAN_POINT('Ctrl Pts',(-50.,2.42857339986351,-10.7835131500112));
#43493=CARTESIAN_POINT('Ctrl Pts',(-66.,2.95266521836539,-10.7260102055487));
#43494=CARTESIAN_POINT('Ctrl Pts',(-50.,2.95266521836539,-10.7260102055487));
#43495=CARTESIAN_POINT('Ctrl Pts',(-66.,3.32360897979558,-10.6831764720218));
#43496=CARTESIAN_POINT('Ctrl Pts',(-50.,3.32360897979558,-10.6831764720218));
#43497=CARTESIAN_POINT('Ctrl Pts',(-66.,3.51446816599279,-10.6606349956381));
#43498=CARTESIAN_POINT('Ctrl Pts',(-50.,3.51446816599279,-10.6606349956381));
#43499=CARTESIAN_POINT('',(-65.5,-0.770750430887795,-10.5970075386067));
#43500=CARTESIAN_POINT('Ctrl Pts',(-66.,-0.37977419449274,-10.1178751010871));
#43501=CARTESIAN_POINT('Ctrl Pts',(-65.798241770306,-0.514032994126835,
-10.3147360059971));
#43502=CARTESIAN_POINT('Ctrl Pts',(-65.6331946192801,-0.690249448192153,
-10.469316144803));
#43503=CARTESIAN_POINT('Ctrl Pts',(-65.5,-0.770750430887792,-10.5970075386067));
#43504=CARTESIAN_POINT('',(-50.,0.0956047792657982,-7.81191500057326));
#43505=CARTESIAN_POINT('',(-66.,0.0956047792657981,-7.81191500057326));
#43506=CARTESIAN_POINT('',(-50.,-0.379774194492752,-10.1178751010871));
#43507=CARTESIAN_POINT('Ctrl Pts',(-50.,0.0956047792657981,-7.81191500057326));
#43508=CARTESIAN_POINT('Ctrl Pts',(-50.,0.0950678851332727,-7.8356437441717));
#43509=CARTESIAN_POINT('Ctrl Pts',(-50.,0.094211047308826,-7.88311229483827));
#43510=CARTESIAN_POINT('Ctrl Pts',(-50.,0.0935766666762872,-7.95434831325083));
#43511=CARTESIAN_POINT('Ctrl Pts',(-50.,0.0940340960600895,-8.04939612696421));
#43512=CARTESIAN_POINT('Ctrl Pts',(-50.,0.0966499958546681,-8.16830957709138));
#43513=CARTESIAN_POINT('Ctrl Pts',(-50.,0.10090393926479,-8.28730423313303));
#43514=CARTESIAN_POINT('Ctrl Pts',(-50.,0.105976022539028,-8.40633495491286));
#43515=CARTESIAN_POINT('Ctrl Pts',(-50.,0.110465593127282,-8.52532414388232));
#43516=CARTESIAN_POINT('Ctrl Pts',(-50.,0.112578665012154,-8.64418593096713));
#43517=CARTESIAN_POINT('Ctrl Pts',(-50.,0.110349727160855,-8.76285633348602));
#43518=CARTESIAN_POINT('Ctrl Pts',(-50.,0.101852305431236,-8.88131667109455));
#43519=CARTESIAN_POINT('Ctrl Pts',(-50.,0.0854084408597768,-8.99963209550245));
#43520=CARTESIAN_POINT('Ctrl Pts',(-50.,0.0598872702371897,-9.11788334516365));
#43521=CARTESIAN_POINT('Ctrl Pts',(-50.,0.025082147178823,-9.23606258270527));
#43522=CARTESIAN_POINT('Ctrl Pts',(-50.,-0.0180301475971287,-9.35400023708443));
#43523=CARTESIAN_POINT('Ctrl Pts',(-50.,-0.0667362885588257,-9.47123116944039));
#43524=CARTESIAN_POINT('Ctrl Pts',(-50.,-0.117449636499862,-9.58714193598532));
#43525=CARTESIAN_POINT('Ctrl Pts',(-50.,-0.167403279296175,-9.70127984211144));
#43526=CARTESIAN_POINT('Ctrl Pts',(-50.,-0.215821651350525,-9.8135627421891));
#43527=CARTESIAN_POINT('Ctrl Pts',(-50.,-0.263208048664824,-9.91861219216685));
#43528=CARTESIAN_POINT('Ctrl Pts',(-50.,-0.306305681352166,-10.0014873049795));
#43529=CARTESIAN_POINT('Ctrl Pts',(-50.,-0.342983873814572,-10.0625463657097));
#43530=CARTESIAN_POINT('Ctrl Pts',(-50.,-0.368567642672767,-10.1014431656146));
#43531=CARTESIAN_POINT('Ctrl Pts',(-50.,-0.379774194492751,-10.1178751010871));
#43532=CARTESIAN_POINT('',(-50.5,-0.770750430887795,-10.5970075386067));
#43533=CARTESIAN_POINT('Ctrl Pts',(-50.5,-0.770750430887802,-10.5970075386067));
#43534=CARTESIAN_POINT('Ctrl Pts',(-50.4694758939836,-0.75230208407391,
-10.5677446024392));
#43535=CARTESIAN_POINT('Ctrl Pts',(-50.437878488726,-0.729472368132695,
-10.5376844269166));
#43536=CARTESIAN_POINT('Ctrl Pts',(-50.2856976867209,-0.610696119298001,
-10.3931263178812));
#43537=CARTESIAN_POINT('Ctrl Pts',(-50.159960596002,-0.48621901035263,-10.2739529360615));
#43538=CARTESIAN_POINT('Ctrl Pts',(-50.,-0.37977419449275,-10.1178751010871));
#43539=CARTESIAN_POINT('Ctrl Pts',(-65.5,-0.770750430887794,-10.5970075386067));
#43540=CARTESIAN_POINT('Ctrl Pts',(-60.5,-0.770750430887794,-10.5970075386067));
#43541=CARTESIAN_POINT('Ctrl Pts',(-55.5,-0.770750430887795,-10.5970075386067));
#43542=CARTESIAN_POINT('Ctrl Pts',(-50.5,-0.770750430887795,-10.5970075386067));
#43543=CARTESIAN_POINT('Origin',(-66.,0.,0.));
#43544=CARTESIAN_POINT('',(-50.,1.53067287083626,-7.66108326625458));
#43545=CARTESIAN_POINT('',(-66.,1.53067287083626,-7.66108326625458));
#43546=CARTESIAN_POINT('Origin',(-50.,0.,0.));
#43547=CARTESIAN_POINT('Ctrl Pts',(-66.,3.51446816599279,-10.6606349956381));
#43548=CARTESIAN_POINT('Ctrl Pts',(-50.,3.51446816599279,-10.6606349956381));
#43549=CARTESIAN_POINT('Ctrl Pts',(-66.,3.49471085893672,-10.6475637798258));
#43550=CARTESIAN_POINT('Ctrl Pts',(-50.,3.49471085893672,-10.6475637798258));
#43551=CARTESIAN_POINT('Ctrl Pts',(-66.,3.45537023612148,-10.621297616078));
#43552=CARTESIAN_POINT('Ctrl Pts',(-50.,3.45537023612148,-10.621297616078));
#43553=CARTESIAN_POINT('Ctrl Pts',(-66.,3.39688127592428,-10.5815271743047));
#43554=CARTESIAN_POINT('Ctrl Pts',(-50.,3.39688127592428,-10.5815271743047));
#43555=CARTESIAN_POINT('Ctrl Pts',(-66.,3.31994133078549,-10.5277565371413));
#43556=CARTESIAN_POINT('Ctrl Pts',(-50.,3.31994133078549,-10.5277565371413));
#43557=CARTESIAN_POINT('Ctrl Pts',(-66.,3.22552017619803,-10.4592986611063));
#43558=CARTESIAN_POINT('Ctrl Pts',(-50.,3.22552017619803,-10.4592986611063));
#43559=CARTESIAN_POINT('Ctrl Pts',(-66.,3.13287341152958,-10.3895893192858));
#43560=CARTESIAN_POINT('Ctrl Pts',(-50.,3.13287341152958,-10.3895893192858));
#43561=CARTESIAN_POINT('Ctrl Pts',(-66.,3.04203169122768,-10.3186223773335));
#43562=CARTESIAN_POINT('Ctrl Pts',(-50.,3.04203169122768,-10.3186223773335));
#43563=CARTESIAN_POINT('Ctrl Pts',(-66.,2.95303632952095,-10.2463944394523));
#43564=CARTESIAN_POINT('Ctrl Pts',(-50.,2.95303632952095,-10.2463944394523));
#43565=CARTESIAN_POINT('Ctrl Pts',(-66.,2.86594045075721,-10.172907326731));
#43566=CARTESIAN_POINT('Ctrl Pts',(-50.,2.86594045075721,-10.172907326731));
#43567=CARTESIAN_POINT('Ctrl Pts',(-66.,2.78080594883332,-10.0981681361864));
#43568=CARTESIAN_POINT('Ctrl Pts',(-50.,2.78080594883332,-10.0981681361864));
#43569=CARTESIAN_POINT('Ctrl Pts',(-66.,2.69769949294062,-10.0221886955761));
#43570=CARTESIAN_POINT('Ctrl Pts',(-50.,2.69769949294062,-10.0221886955761));
#43571=CARTESIAN_POINT('Ctrl Pts',(-66.,2.61668829606168,-9.94498553626488));
#43572=CARTESIAN_POINT('Ctrl Pts',(-50.,2.61668829606168,-9.94498553626488));
#43573=CARTESIAN_POINT('Ctrl Pts',(-66.,2.53783659863859,-9.86657949215571));
#43574=CARTESIAN_POINT('Ctrl Pts',(-50.,2.53783659863859,-9.86657949215571));
#43575=CARTESIAN_POINT('Ctrl Pts',(-66.,2.46119946285178,-9.78699646071692));
#43576=CARTESIAN_POINT('Ctrl Pts',(-50.,2.46119946285178,-9.78699646071692));
#43577=CARTESIAN_POINT('Ctrl Pts',(-66.,2.38682820441919,-9.70626369932132));
#43578=CARTESIAN_POINT('Ctrl Pts',(-50.,2.38682820441919,-9.70626369932132));
#43579=CARTESIAN_POINT('Ctrl Pts',(-66.,2.31478185538763,-9.62440406213512));
#43580=CARTESIAN_POINT('Ctrl Pts',(-50.,2.31478185538763,-9.62440406213512));
#43581=CARTESIAN_POINT('Ctrl Pts',(-66.,2.24513642875384,-9.54143066294722));
#43582=CARTESIAN_POINT('Ctrl Pts',(-50.,2.24513642875384,-9.54143066294722));
#43583=CARTESIAN_POINT('Ctrl Pts',(-66.,2.17799511452139,-9.45734217317086));
#43584=CARTESIAN_POINT('Ctrl Pts',(-50.,2.17799511452139,-9.45734217317086));
#43585=CARTESIAN_POINT('Ctrl Pts',(-66.,2.11349742683576,-9.37211610318578));
#43586=CARTESIAN_POINT('Ctrl Pts',(-50.,2.11349742683576,-9.37211610318578));
#43587=CARTESIAN_POINT('Ctrl Pts',(-66.,2.05183036091841,-9.28571118746575));
#43588=CARTESIAN_POINT('Ctrl Pts',(-50.,2.05183036091841,-9.28571118746575));
#43589=CARTESIAN_POINT('Ctrl Pts',(-66.,1.99323835737743,-9.19807604064094));
#43590=CARTESIAN_POINT('Ctrl Pts',(-50.,1.99323835737743,-9.19807604064094));
#43591=CARTESIAN_POINT('Ctrl Pts',(-66.,1.93803736866688,-9.10915586281889));
#43592=CARTESIAN_POINT('Ctrl Pts',(-50.,1.93803736866688,-9.10915586281889));
#43593=CARTESIAN_POINT('Ctrl Pts',(-66.,1.88661896349422,-9.01890038196952));
#43594=CARTESIAN_POINT('Ctrl Pts',(-50.,1.88661896349422,-9.01890038196952));
#43595=CARTESIAN_POINT('Ctrl Pts',(-66.,1.83947938032835,-8.92727064057537));
#43596=CARTESIAN_POINT('Ctrl Pts',(-50.,1.83947938032835,-8.92727064057537));
#43597=CARTESIAN_POINT('Ctrl Pts',(-66.,1.79714183408573,-8.83425001254252));
#43598=CARTESIAN_POINT('Ctrl Pts',(-50.,1.79714183408573,-8.83425001254252));
#43599=CARTESIAN_POINT('Ctrl Pts',(-66.,1.76001840564001,-8.73985705693077));
#43600=CARTESIAN_POINT('Ctrl Pts',(-50.,1.76001840564001,-8.73985705693077));
#43601=CARTESIAN_POINT('Ctrl Pts',(-66.,1.72828159952138,-8.64415925811045));
#43602=CARTESIAN_POINT('Ctrl Pts',(-50.,1.72828159952138,-8.64415925811045));
#43603=CARTESIAN_POINT('Ctrl Pts',(-66.,1.70174735094098,-8.54728433152241));
#43604=CARTESIAN_POINT('Ctrl Pts',(-50.,1.70174735094098,-8.54728433152241));
#43605=CARTESIAN_POINT('Ctrl Pts',(-66.,1.67970691947077,-8.44943937069158));
#43606=CARTESIAN_POINT('Ctrl Pts',(-50.,1.67970691947077,-8.44943937069158));
#43607=CARTESIAN_POINT('Ctrl Pts',(-66.,1.66103994900115,-8.35088931899355));
#43608=CARTESIAN_POINT('Ctrl Pts',(-50.,1.66103994900115,-8.35088931899355));
#43609=CARTESIAN_POINT('Ctrl Pts',(-66.,1.64442807858968,-8.25192111283452));
#43610=CARTESIAN_POINT('Ctrl Pts',(-50.,1.64442807858968,-8.25192111283452));
#43611=CARTESIAN_POINT('Ctrl Pts',(-66.,1.62853781891495,-8.15281204423512));
#43612=CARTESIAN_POINT('Ctrl Pts',(-50.,1.62853781891495,-8.15281204423512));
#43613=CARTESIAN_POINT('Ctrl Pts',(-66.,1.61220661573863,-8.05379804635934));
#43614=CARTESIAN_POINT('Ctrl Pts',(-50.,1.61220661573863,-8.05379804635934));
#43615=CARTESIAN_POINT('Ctrl Pts',(-66.,1.59465171544125,-7.95503756783394));
#43616=CARTESIAN_POINT('Ctrl Pts',(-50.,1.59465171544125,-7.95503756783394));
#43617=CARTESIAN_POINT('Ctrl Pts',(-66.,1.5754164725369,-7.85662314056401));
#43618=CARTESIAN_POINT('Ctrl Pts',(-50.,1.5754164725369,-7.85662314056401));
#43619=CARTESIAN_POINT('Ctrl Pts',(-66.,1.55850498002059,-7.77820466719577));
#43620=CARTESIAN_POINT('Ctrl Pts',(-50.,1.55850498002059,-7.77820466719577));
#43621=CARTESIAN_POINT('Ctrl Pts',(-66.,1.54493370114459,-7.71957314695095));
#43622=CARTESIAN_POINT('Ctrl Pts',(-50.,1.54493370114459,-7.71957314695095));
#43623=CARTESIAN_POINT('Ctrl Pts',(-66.,1.53549215119571,-7.68056640390788));
#43624=CARTESIAN_POINT('Ctrl Pts',(-50.,1.53549215119571,-7.68056640390788));
#43625=CARTESIAN_POINT('Ctrl Pts',(-66.,1.53067287083627,-7.66108326625457));
#43626=CARTESIAN_POINT('Ctrl Pts',(-50.,1.53067287083627,-7.66108326625457));
#43627=CARTESIAN_POINT('Ctrl Pts',(-50.,2.48815856278712,-9.81451435204154));
#43628=CARTESIAN_POINT('Ctrl Pts',(-50.,2.48285278315604,-9.80896726509534));
#43629=CARTESIAN_POINT('Ctrl Pts',(-50.,2.46234274539512,-9.78744217177353));
#43630=CARTESIAN_POINT('Ctrl Pts',(-50.,2.4269715452022,-9.74976313360792));
#43631=CARTESIAN_POINT('Ctrl Pts',(-50.,2.37742992422592,-9.69558529830397));
#43632=CARTESIAN_POINT('Ctrl Pts',(-50.,2.31478185538763,-9.62440406213512));
#43633=CARTESIAN_POINT('Ctrl Pts',(-50.,2.24513642875384,-9.54143066294722));
#43634=CARTESIAN_POINT('Ctrl Pts',(-50.,2.17799511452139,-9.45734217317086));
#43635=CARTESIAN_POINT('Ctrl Pts',(-50.,2.11349742683576,-9.37211610318578));
#43636=CARTESIAN_POINT('Ctrl Pts',(-50.,2.05183036091841,-9.28571118746575));
#43637=CARTESIAN_POINT('Ctrl Pts',(-50.,1.99323835737743,-9.19807604064094));
#43638=CARTESIAN_POINT('Ctrl Pts',(-50.,1.93803736866688,-9.10915586281889));
#43639=CARTESIAN_POINT('Ctrl Pts',(-50.,1.88661896349422,-9.01890038196952));
#43640=CARTESIAN_POINT('Ctrl Pts',(-50.,1.83947938032835,-8.92727064057537));
#43641=CARTESIAN_POINT('Ctrl Pts',(-50.,1.79714183408573,-8.83425001254252));
#43642=CARTESIAN_POINT('Ctrl Pts',(-50.,1.76001840564001,-8.73985705693077));
#43643=CARTESIAN_POINT('Ctrl Pts',(-50.,1.72828159952138,-8.64415925811045));
#43644=CARTESIAN_POINT('Ctrl Pts',(-50.,1.70174735094098,-8.54728433152241));
#43645=CARTESIAN_POINT('Ctrl Pts',(-50.,1.67970691947077,-8.44943937069158));
#43646=CARTESIAN_POINT('Ctrl Pts',(-50.,1.66103994900115,-8.35088931899355));
#43647=CARTESIAN_POINT('Ctrl Pts',(-50.,1.64442807858968,-8.25192111283452));
#43648=CARTESIAN_POINT('Ctrl Pts',(-50.,1.62853781891495,-8.15281204423512));
#43649=CARTESIAN_POINT('Ctrl Pts',(-50.,1.61220661573863,-8.05379804635934));
#43650=CARTESIAN_POINT('Ctrl Pts',(-50.,1.59465171544125,-7.95503756783394));
#43651=CARTESIAN_POINT('Ctrl Pts',(-50.,1.5754164725369,-7.85662314056401));
#43652=CARTESIAN_POINT('Ctrl Pts',(-50.,1.55850498002059,-7.77820466719577));
#43653=CARTESIAN_POINT('Ctrl Pts',(-50.,1.54493370114459,-7.71957314695095));
#43654=CARTESIAN_POINT('Ctrl Pts',(-50.,1.53549215119571,-7.68056640390788));
#43655=CARTESIAN_POINT('Ctrl Pts',(-50.,1.53067287083627,-7.66108326625457));
#43656=CARTESIAN_POINT('Origin',(-50.,1.47877611889991,-9.39020011572736));
#43657=CARTESIAN_POINT('Origin',(-50.,0.,0.));
#43658=CARTESIAN_POINT('Origin',(-65.75,0.,0.));
#43659=CARTESIAN_POINT('',(-65.5,-1.48968674337242,-10.5200503043769));
#43660=CARTESIAN_POINT('Origin',(-65.5,0.,0.));
#43661=CARTESIAN_POINT('',(-66.,-1.71887666803992,-9.97803026654399));
#43662=CARTESIAN_POINT('Ctrl Pts',(-65.5,-1.48968674337242,-10.5200503043769));
#43663=CARTESIAN_POINT('Ctrl Pts',(-65.6641545839451,-1.57632238482973,
-10.3419900891876));
#43664=CARTESIAN_POINT('Ctrl Pts',(-65.8307068049194,-1.65322389214929,
-10.1611267872057));
#43665=CARTESIAN_POINT('Ctrl Pts',(-66.,-1.71887666803992,-9.97803026654399));
#43666=CARTESIAN_POINT('Origin',(-66.,0.,0.));
#43667=CARTESIAN_POINT('Origin',(-58.,0.,0.));
#43668=CARTESIAN_POINT('',(-50.5,-1.48968674337242,-10.5200503043769));
#43669=CARTESIAN_POINT('Origin',(-50.5,0.,0.));
#43670=CARTESIAN_POINT('Ctrl Pts',(-50.5,-1.48968674337242,-10.5200503043769));
#43671=CARTESIAN_POINT('Ctrl Pts',(-55.5,-1.48968674337242,-10.5200503043769));
#43672=CARTESIAN_POINT('Ctrl Pts',(-60.5,-1.48968674337242,-10.5200503043769));
#43673=CARTESIAN_POINT('Ctrl Pts',(-65.5,-1.48968674337242,-10.5200503043769));
#43674=CARTESIAN_POINT('Origin',(-50.25,0.,0.));
#43675=CARTESIAN_POINT('',(-50.,-1.71887666803992,-9.97803026654401));
#43676=CARTESIAN_POINT('Origin',(-50.,0.,0.));
#43677=CARTESIAN_POINT('Ctrl Pts',(-50.,-1.71887666803992,-9.97803026654401));
#43678=CARTESIAN_POINT('Ctrl Pts',(-50.1692931950804,-1.65322389214937,
-10.1611267872055));
#43679=CARTESIAN_POINT('Ctrl Pts',(-50.3358454160543,-1.57632238483005,
-10.341990089187));
#43680=CARTESIAN_POINT('Ctrl Pts',(-50.5,-1.48968674337242,-10.5200503043769));
#43681=CARTESIAN_POINT('Origin',(-66.,-2.46840926658957,-9.17984709653976));
#43682=CARTESIAN_POINT('',(-66.,-4.46225154398509,-9.08867075859846));
#43683=CARTESIAN_POINT('Origin',(-66.,0.,0.));
#43684=CARTESIAN_POINT('',(-66.,-1.71770404175135,-7.62132856363975));
#43685=CARTESIAN_POINT('Ctrl Pts',(-66.,-1.71770404175134,-7.62132856363975));
#43686=CARTESIAN_POINT('Ctrl Pts',(-66.,-1.72122591607555,-7.64108747345899));
#43687=CARTESIAN_POINT('Ctrl Pts',(-66.,-1.7284661027293,-7.68056213071507));
#43688=CARTESIAN_POINT('Ctrl Pts',(-66.,-1.73991571028055,-7.73964462612166));
#43689=CARTESIAN_POINT('Ctrl Pts',(-66.,-1.75636195972324,-7.81816198995797));
#43690=CARTESIAN_POINT('Ctrl Pts',(-66.,-1.77881844471932,-7.91589172108458));
#43691=CARTESIAN_POINT('Ctrl Pts',(-66.,-1.80295075079726,-8.01325412885256));
#43692=CARTESIAN_POINT('Ctrl Pts',(-66.,-1.8283040754312,-8.11035041561234));
#43693=CARTESIAN_POINT('Ctrl Pts',(-66.,-1.85409889074508,-8.20735420592021));
#43694=CARTESIAN_POINT('Ctrl Pts',(-66.,-1.87917718793209,-8.3045228175142));
#43695=CARTESIAN_POINT('Ctrl Pts',(-66.,-1.90220797905422,-8.40214531049858));
#43696=CARTESIAN_POINT('Ctrl Pts',(-66.,-1.92187017391035,-8.50049578112694));
#43697=CARTESIAN_POINT('Ctrl Pts',(-66.,-1.9370325140864,-8.59978788146503));
#43698=CARTESIAN_POINT('Ctrl Pts',(-66.,-1.94696330045856,-8.70012069286638));
#43699=CARTESIAN_POINT('Ctrl Pts',(-66.,-1.95144243492538,-8.80145240736443));
#43700=CARTESIAN_POINT('Ctrl Pts',(-66.,-1.95060005985058,-8.90365121100569));
#43701=CARTESIAN_POINT('Ctrl Pts',(-66.,-1.94480508119479,-9.00653254085416));
#43702=CARTESIAN_POINT('Ctrl Pts',(-66.,-1.93454224200995,-9.10989877492369));
#43703=CARTESIAN_POINT('Ctrl Pts',(-66.,-1.92028072414509,-9.21358366430839));
#43704=CARTESIAN_POINT('Ctrl Pts',(-66.,-1.90239869089103,-9.31747386945138));
#43705=CARTESIAN_POINT('Ctrl Pts',(-66.,-1.8812070683013,-9.42149094310496));
#43706=CARTESIAN_POINT('Ctrl Pts',(-66.,-1.85695006429591,-9.52558240518797));
#43707=CARTESIAN_POINT('Ctrl Pts',(-66.,-1.82981529171165,-9.6297098958258));
#43708=CARTESIAN_POINT('Ctrl Pts',(-66.,-1.79993935041505,-9.73383721479367));
#43709=CARTESIAN_POINT('Ctrl Pts',(-66.,-1.77165950874705,-9.82434577497958));
#43710=CARTESIAN_POINT('Ctrl Pts',(-66.,-1.74843709680056,-9.89399008293483));
#43711=CARTESIAN_POINT('Ctrl Pts',(-66.,-1.73144934303076,-9.94279836032739));
#43712=CARTESIAN_POINT('Ctrl Pts',(-66.,-1.72146753539781,-9.97080469546509));
#43713=CARTESIAN_POINT('Ctrl Pts',(-66.,-1.71887666803992,-9.97803026654399));
#43714=CARTESIAN_POINT('',(-66.,-3.09005277149946,-7.17542543124437));
#43715=CARTESIAN_POINT('Origin',(-66.,0.,0.));
#43716=CARTESIAN_POINT('Ctrl Pts',(-66.,-4.46225154398509,-9.08867075859846));
#43717=CARTESIAN_POINT('Ctrl Pts',(-66.,-4.44533037920078,-9.07821755385499));
#43718=CARTESIAN_POINT('Ctrl Pts',(-66.,-4.4061376895513,-9.05308941524767));
#43719=CARTESIAN_POINT('Ctrl Pts',(-66.,-4.34779553604197,-9.0122275525459));
#43720=CARTESIAN_POINT('Ctrl Pts',(-66.,-4.27471554428536,-8.95404675612808));
#43721=CARTESIAN_POINT('Ctrl Pts',(-66.,-4.18869845562393,-8.87735309244413));
#43722=CARTESIAN_POINT('Ctrl Pts',(-66.,-4.09879650191483,-8.79447108521983));
#43723=CARTESIAN_POINT('Ctrl Pts',(-66.,-4.00673750966012,-8.71051889651385));
#43724=CARTESIAN_POINT('Ctrl Pts',(-66.,-3.91326340492591,-8.62525611914553));
#43725=CARTESIAN_POINT('Ctrl Pts',(-66.,-3.82108601519994,-8.53797090566847));
#43726=CARTESIAN_POINT('Ctrl Pts',(-66.,-3.73373140850441,-8.44776484727783));
#43727=CARTESIAN_POINT('Ctrl Pts',(-66.,-3.65386752007281,-8.35395926054862));
#43728=CARTESIAN_POINT('Ctrl Pts',(-66.,-3.58245565425011,-8.25631176382647));
#43729=CARTESIAN_POINT('Ctrl Pts',(-66.,-3.519310217917,-8.15491356756456));
#43730=CARTESIAN_POINT('Ctrl Pts',(-66.,-3.46336527683772,-8.05015087702059));
#43731=CARTESIAN_POINT('Ctrl Pts',(-66.,-3.41306143963531,-7.9426466605421));
#43732=CARTESIAN_POINT('Ctrl Pts',(-66.,-3.36664638258854,-7.83320155109845));
#43733=CARTESIAN_POINT('Ctrl Pts',(-66.,-3.32235054612245,-7.72267344513691));
#43734=CARTESIAN_POINT('Ctrl Pts',(-66.,-3.2785699685588,-7.61187046781066));
#43735=CARTESIAN_POINT('Ctrl Pts',(-66.,-3.23405665229585,-7.5014332056376));
#43736=CARTESIAN_POINT('Ctrl Pts',(-66.,-3.18807993814955,-7.39173638112025));
#43737=CARTESIAN_POINT('Ctrl Pts',(-66.,-3.14983839200384,-7.30471982935151));
#43738=CARTESIAN_POINT('Ctrl Pts',(-66.,-3.12028455746335,-7.23990051415909));
#43739=CARTESIAN_POINT('Ctrl Pts',(-66.,-3.1001945982111,-7.19688434265714));
#43740=CARTESIAN_POINT('Ctrl Pts',(-66.,-3.09005277149946,-7.17542543124437));
#43741=CARTESIAN_POINT('Ctrl Pts',(-66.,-3.09005277149946,-7.17542543124437));
#43742=CARTESIAN_POINT('Ctrl Pts',(-50.,-3.09005277149946,-7.17542543124437));
#43743=CARTESIAN_POINT('Ctrl Pts',(-66.,-3.1001945982111,-7.19688434265714));
#43744=CARTESIAN_POINT('Ctrl Pts',(-50.,-3.1001945982111,-7.19688434265714));
#43745=CARTESIAN_POINT('Ctrl Pts',(-66.,-3.12028455746335,-7.23990051415909));
#43746=CARTESIAN_POINT('Ctrl Pts',(-50.,-3.12028455746335,-7.23990051415909));
#43747=CARTESIAN_POINT('Ctrl Pts',(-66.,-3.14983839200384,-7.30471982935151));
#43748=CARTESIAN_POINT('Ctrl Pts',(-50.,-3.14983839200384,-7.30471982935151));
#43749=CARTESIAN_POINT('Ctrl Pts',(-66.,-3.18807993814955,-7.39173638112025));
#43750=CARTESIAN_POINT('Ctrl Pts',(-50.,-3.18807993814955,-7.39173638112025));
#43751=CARTESIAN_POINT('Ctrl Pts',(-66.,-3.23405665229585,-7.5014332056376));
#43752=CARTESIAN_POINT('Ctrl Pts',(-50.,-3.23405665229585,-7.5014332056376));
#43753=CARTESIAN_POINT('Ctrl Pts',(-66.,-3.2785699685588,-7.61187046781066));
#43754=CARTESIAN_POINT('Ctrl Pts',(-50.,-3.2785699685588,-7.61187046781066));
#43755=CARTESIAN_POINT('Ctrl Pts',(-66.,-3.32235054612245,-7.72267344513691));
#43756=CARTESIAN_POINT('Ctrl Pts',(-50.,-3.32235054612245,-7.72267344513691));
#43757=CARTESIAN_POINT('Ctrl Pts',(-66.,-3.36664638258854,-7.83320155109845));
#43758=CARTESIAN_POINT('Ctrl Pts',(-50.,-3.36664638258854,-7.83320155109845));
#43759=CARTESIAN_POINT('Ctrl Pts',(-66.,-3.41306143963531,-7.9426466605421));
#43760=CARTESIAN_POINT('Ctrl Pts',(-50.,-3.41306143963531,-7.9426466605421));
#43761=CARTESIAN_POINT('Ctrl Pts',(-66.,-3.46336527683772,-8.05015087702059));
#43762=CARTESIAN_POINT('Ctrl Pts',(-50.,-3.46336527683772,-8.05015087702059));
#43763=CARTESIAN_POINT('Ctrl Pts',(-66.,-3.519310217917,-8.15491356756456));
#43764=CARTESIAN_POINT('Ctrl Pts',(-50.,-3.519310217917,-8.15491356756456));
#43765=CARTESIAN_POINT('Ctrl Pts',(-66.,-3.58245565425011,-8.25631176382647));
#43766=CARTESIAN_POINT('Ctrl Pts',(-50.,-3.58245565425011,-8.25631176382647));
#43767=CARTESIAN_POINT('Ctrl Pts',(-66.,-3.65386752007281,-8.35395926054862));
#43768=CARTESIAN_POINT('Ctrl Pts',(-50.,-3.65386752007281,-8.35395926054862));
#43769=CARTESIAN_POINT('Ctrl Pts',(-66.,-3.73373140850441,-8.44776484727783));
#43770=CARTESIAN_POINT('Ctrl Pts',(-50.,-3.73373140850441,-8.44776484727783));
#43771=CARTESIAN_POINT('Ctrl Pts',(-66.,-3.82108601519994,-8.53797090566847));
#43772=CARTESIAN_POINT('Ctrl Pts',(-50.,-3.82108601519994,-8.53797090566847));
#43773=CARTESIAN_POINT('Ctrl Pts',(-66.,-3.91326340492591,-8.62525611914553));
#43774=CARTESIAN_POINT('Ctrl Pts',(-50.,-3.91326340492591,-8.62525611914553));
#43775=CARTESIAN_POINT('Ctrl Pts',(-66.,-4.00673750966012,-8.71051889651385));
#43776=CARTESIAN_POINT('Ctrl Pts',(-50.,-4.00673750966012,-8.71051889651385));
#43777=CARTESIAN_POINT('Ctrl Pts',(-66.,-4.09879650191483,-8.79447108521983));
#43778=CARTESIAN_POINT('Ctrl Pts',(-50.,-4.09879650191483,-8.79447108521983));
#43779=CARTESIAN_POINT('Ctrl Pts',(-66.,-4.18869845562393,-8.87735309244413));
#43780=CARTESIAN_POINT('Ctrl Pts',(-50.,-4.18869845562393,-8.87735309244413));
#43781=CARTESIAN_POINT('Ctrl Pts',(-66.,-4.27965645364851,-8.95845211844488));
#43782=CARTESIAN_POINT('Ctrl Pts',(-50.,-4.27965645364851,-8.95845211844488));
#43783=CARTESIAN_POINT('Ctrl Pts',(-66.,-4.3781743773292,-9.03625199707944));
#43784=CARTESIAN_POINT('Ctrl Pts',(-50.,-4.3781743773292,-9.03625199707944));
#43785=CARTESIAN_POINT('Ctrl Pts',(-66.,-4.4903058862283,-9.10931646690967));
#43786=CARTESIAN_POINT('Ctrl Pts',(-50.,-4.4903058862283,-9.10931646690967));
#43787=CARTESIAN_POINT('Ctrl Pts',(-66.,-4.61889543384362,-9.17693917574169));
#43788=CARTESIAN_POINT('Ctrl Pts',(-50.,-4.61889543384362,-9.17693917574169));
#43789=CARTESIAN_POINT('Ctrl Pts',(-66.,-4.76000514096471,-9.23998558422727));
#43790=CARTESIAN_POINT('Ctrl Pts',(-50.,-4.76000514096471,-9.23998558422727));
#43791=CARTESIAN_POINT('Ctrl Pts',(-66.,-4.90085865419307,-9.30137962583606));
#43792=CARTESIAN_POINT('Ctrl Pts',(-50.,-4.90085865419307,-9.30137962583606));
#43793=CARTESIAN_POINT('Ctrl Pts',(-66.,-5.02348185505654,-9.36525860678472));
#43794=CARTESIAN_POINT('Ctrl Pts',(-50.,-5.02348185505654,-9.36525860678472));
#43795=CARTESIAN_POINT('Ctrl Pts',(-66.,-5.10755750085189,-9.43631208950852));
#43796=CARTESIAN_POINT('Ctrl Pts',(-50.,-5.10755750085189,-9.43631208950852));
#43797=CARTESIAN_POINT('Ctrl Pts',(-66.,-5.13345766798759,-9.51907903097904));
#43798=CARTESIAN_POINT('Ctrl Pts',(-50.,-5.13345766798759,-9.51907903097904));
#43799=CARTESIAN_POINT('Ctrl Pts',(-66.,-5.08549602968051,-9.61719469919379));
#43800=CARTESIAN_POINT('Ctrl Pts',(-50.,-5.08549602968051,-9.61719469919379));
#43801=CARTESIAN_POINT('Ctrl Pts',(-66.,-4.95176210550526,-9.73342698726024));
#43802=CARTESIAN_POINT('Ctrl Pts',(-50.,-4.95176210550526,-9.73342698726024));
#43803=CARTESIAN_POINT('Ctrl Pts',(-66.,-4.72347140525311,-9.86982476028545));
#43804=CARTESIAN_POINT('Ctrl Pts',(-50.,-4.72347140525311,-9.86982476028545));
#43805=CARTESIAN_POINT('Ctrl Pts',(-66.,-4.39451568841758,-10.0278201090025));
#43806=CARTESIAN_POINT('Ctrl Pts',(-50.,-4.39451568841758,-10.0278201090025));
#43807=CARTESIAN_POINT('Ctrl Pts',(-66.,-3.96095558080252,-10.2083440731201));
#43808=CARTESIAN_POINT('Ctrl Pts',(-50.,-3.96095558080252,-10.2083440731201));
#43809=CARTESIAN_POINT('Ctrl Pts',(-66.,-3.42056292700896,-10.4119310097664));
#43810=CARTESIAN_POINT('Ctrl Pts',(-50.,-3.42056292700896,-10.4119310097664));
#43811=CARTESIAN_POINT('Ctrl Pts',(-66.,-2.77236455694589,-10.6388227675402));
#43812=CARTESIAN_POINT('Ctrl Pts',(-50.,-2.77236455694589,-10.6388227675402));
#43813=CARTESIAN_POINT('Ctrl Pts',(-66.,-2.16743774120234,-10.8390192477456));
#43814=CARTESIAN_POINT('Ctrl Pts',(-50.,-2.16743774120234,-10.8390192477456));
#43815=CARTESIAN_POINT('Ctrl Pts',(-66.,-1.66526748642465,-10.9996550409518));
#43816=CARTESIAN_POINT('Ctrl Pts',(-50.,-1.66526748642465,-10.9996550409518));
#43817=CARTESIAN_POINT('Ctrl Pts',(-66.,-1.30897144914411,-11.1114008985485));
#43818=CARTESIAN_POINT('Ctrl Pts',(-50.,-1.30897144914411,-11.1114008985485));
#43819=CARTESIAN_POINT('Ctrl Pts',(-66.,-1.12544446210999,-11.1684376598836));
#43820=CARTESIAN_POINT('Ctrl Pts',(-50.,-1.12544446210999,-11.1684376598836));
#43821=CARTESIAN_POINT('',(-65.5,-5.01430682801544,-9.36735565858998));
#43822=CARTESIAN_POINT('Ctrl Pts',(-66.,-4.46225154398508,-9.08867075859845));
#43823=CARTESIAN_POINT('Ctrl Pts',(-65.798241770306,-4.6649736041553,-9.21390417059987));
#43824=CARTESIAN_POINT('Ctrl Pts',(-65.6331946192802,-4.8888287520727,-9.28344646526655));
#43825=CARTESIAN_POINT('Ctrl Pts',(-65.5,-5.01430682801543,-9.36735565858998));
#43826=CARTESIAN_POINT('',(-50.,-3.09005277149946,-7.17542543124437));
#43827=CARTESIAN_POINT('',(-66.,-3.09005277149946,-7.17542543124437));
#43828=CARTESIAN_POINT('',(-50.,-4.46225154398511,-9.08867075859847));
#43829=CARTESIAN_POINT('Ctrl Pts',(-50.,-3.09005277149946,-7.17542543124437));
#43830=CARTESIAN_POINT('Ctrl Pts',(-50.,-3.1001945982111,-7.19688434265714));
#43831=CARTESIAN_POINT('Ctrl Pts',(-50.,-3.12028455746335,-7.23990051415909));
#43832=CARTESIAN_POINT('Ctrl Pts',(-50.,-3.14983839200384,-7.30471982935151));
#43833=CARTESIAN_POINT('Ctrl Pts',(-50.,-3.18807993814955,-7.39173638112025));
#43834=CARTESIAN_POINT('Ctrl Pts',(-50.,-3.23405665229585,-7.5014332056376));
#43835=CARTESIAN_POINT('Ctrl Pts',(-50.,-3.2785699685588,-7.61187046781066));
#43836=CARTESIAN_POINT('Ctrl Pts',(-50.,-3.32235054612245,-7.72267344513691));
#43837=CARTESIAN_POINT('Ctrl Pts',(-50.,-3.36664638258854,-7.83320155109845));
#43838=CARTESIAN_POINT('Ctrl Pts',(-50.,-3.41306143963531,-7.9426466605421));
#43839=CARTESIAN_POINT('Ctrl Pts',(-50.,-3.46336527683772,-8.05015087702059));
#43840=CARTESIAN_POINT('Ctrl Pts',(-50.,-3.519310217917,-8.15491356756456));
#43841=CARTESIAN_POINT('Ctrl Pts',(-50.,-3.58245565425011,-8.25631176382647));
#43842=CARTESIAN_POINT('Ctrl Pts',(-50.,-3.65386752007281,-8.35395926054862));
#43843=CARTESIAN_POINT('Ctrl Pts',(-50.,-3.73373140850441,-8.44776484727783));
#43844=CARTESIAN_POINT('Ctrl Pts',(-50.,-3.82108601519994,-8.53797090566847));
#43845=CARTESIAN_POINT('Ctrl Pts',(-50.,-3.91326340492591,-8.62525611914553));
#43846=CARTESIAN_POINT('Ctrl Pts',(-50.,-4.00673750966012,-8.71051889651385));
#43847=CARTESIAN_POINT('Ctrl Pts',(-50.,-4.09879650191483,-8.79447108521983));
#43848=CARTESIAN_POINT('Ctrl Pts',(-50.,-4.18869845562393,-8.87735309244413));
#43849=CARTESIAN_POINT('Ctrl Pts',(-50.,-4.27471554428537,-8.95404675612808));
#43850=CARTESIAN_POINT('Ctrl Pts',(-50.,-4.34779553604197,-9.01222755254591));
#43851=CARTESIAN_POINT('Ctrl Pts',(-50.,-4.40613768955131,-9.05308941524767));
#43852=CARTESIAN_POINT('Ctrl Pts',(-50.,-4.4453303792008,-9.078217553855));
#43853=CARTESIAN_POINT('Ctrl Pts',(-50.,-4.46225154398511,-9.08867075859847));
#43854=CARTESIAN_POINT('',(-50.5,-5.01430682801544,-9.36735565858998));
#43855=CARTESIAN_POINT('Ctrl Pts',(-50.5,-5.01430682801073,-9.36735565858683));
#43856=CARTESIAN_POINT('Ctrl Pts',(-50.4646931597002,-4.98104387220113,
-9.3451121888133));
#43857=CARTESIAN_POINT('Ctrl Pts',(-50.4273092286687,-4.94135377127855,
-9.3238710729983));
#43858=CARTESIAN_POINT('Ctrl Pts',(-50.3882921463906,-4.89776472393815,
-9.3027242489053));
#43859=CARTESIAN_POINT('Ctrl Pts',(-50.3470342768248,-4.85167231710866,
-9.28036294305628));
#43860=CARTESIAN_POINT('Ctrl Pts',(-50.3039502825837,-4.80121938499207,
-9.25810755978088));
#43861=CARTESIAN_POINT('Ctrl Pts',(-50.2595650675693,-4.74936366142675,
-9.23486526462329));
#43862=CARTESIAN_POINT('Ctrl Pts',(-50.2356844321301,-4.7214636584754,-9.22236018208065));
#43863=CARTESIAN_POINT('Ctrl Pts',(-50.2117779267271,-4.69355955980766,
-9.20974769064843));
#43864=CARTESIAN_POINT('Ctrl Pts',(-50.187514972923,-4.66565475603887,-9.19668496860533));
#43865=CARTESIAN_POINT('Ctrl Pts',(-50.1572202993005,-4.63081287613014,
-9.18037488104914));
#43866=CARTESIAN_POINT('Ctrl Pts',(-50.1263699237746,-4.59596559770358,
-9.16336504760852));
#43867=CARTESIAN_POINT('Ctrl Pts',(-50.0943203555449,-4.5610688467911,-9.14496806771221));
#43868=CARTESIAN_POINT('Ctrl Pts',(-50.0678556302452,-4.53225307866182,
-9.1297768796185));
#43869=CARTESIAN_POINT('Ctrl Pts',(-50.0405732324447,-4.50340555423355,
-9.11363890457985));
#43870=CARTESIAN_POINT('Ctrl Pts',(-50.0121108541095,-4.47448813501866,
-9.09615015924532));
#43871=CARTESIAN_POINT('Ctrl Pts',(-50.0080976999835,-4.47041082078763,
-9.0936842714804));
#43872=CARTESIAN_POINT('Ctrl Pts',(-50.0040610871464,-4.46633203157711,
-9.09119151723395));
#43873=CARTESIAN_POINT('Ctrl Pts',(-50.,-4.46225154398511,-9.08867075859847));
#43874=CARTESIAN_POINT('Ctrl Pts',(-65.5,-5.01430682801544,-9.36735565858998));
#43875=CARTESIAN_POINT('Ctrl Pts',(-60.5,-5.01430682801544,-9.36735565858998));
#43876=CARTESIAN_POINT('Ctrl Pts',(-55.5,-5.01430682801544,-9.36735565858998));
#43877=CARTESIAN_POINT('Ctrl Pts',(-50.5,-5.01430682801544,-9.36735565858998));
#43878=CARTESIAN_POINT('Origin',(-66.,0.,0.));
#43879=CARTESIAN_POINT('',(-50.,-1.71770404175135,-7.62132856363975));
#43880=CARTESIAN_POINT('',(-66.,-1.71770404175135,-7.62132856363975));
#43881=CARTESIAN_POINT('Origin',(-50.,0.,0.));
#43882=CARTESIAN_POINT('Ctrl Pts',(-66.,-1.12544446210999,-11.1684376598836));
#43883=CARTESIAN_POINT('Ctrl Pts',(-50.,-1.12544446210999,-11.1684376598836));
#43884=CARTESIAN_POINT('Ctrl Pts',(-66.,-1.13817711778593,-11.1484604893043));
#43885=CARTESIAN_POINT('Ctrl Pts',(-50.,-1.13817711778593,-11.1484604893043));
#43886=CARTESIAN_POINT('Ctrl Pts',(-66.,-1.16343315379036,-11.1084638818624));
#43887=CARTESIAN_POINT('Ctrl Pts',(-50.,-1.16343315379036,-11.1084638818624));
#43888=CARTESIAN_POINT('Ctrl Pts',(-66.,-1.20068938172024,-11.0483421721043));
#43889=CARTESIAN_POINT('Ctrl Pts',(-50.,-1.20068938172024,-11.0483421721043));
#43890=CARTESIAN_POINT('Ctrl Pts',(-66.,-1.24910703065715,-10.9679259557649));
#43891=CARTESIAN_POINT('Ctrl Pts',(-50.,-1.24910703065715,-10.9679259557649));
#43892=CARTESIAN_POINT('Ctrl Pts',(-66.,-1.30752072084532,-10.8669820306211));
#43893=CARTESIAN_POINT('Ctrl Pts',(-50.,-1.30752072084532,-10.8669820306211));
#43894=CARTESIAN_POINT('Ctrl Pts',(-66.,-1.36380440819035,-10.7656165439926));
#43895=CARTESIAN_POINT('Ctrl Pts',(-50.,-1.36380440819035,-10.7656165439926));
#43896=CARTESIAN_POINT('Ctrl Pts',(-66.,-1.41792759339758,-10.6638363601625));
#43897=CARTESIAN_POINT('Ctrl Pts',(-50.,-1.41792759339758,-10.6638363601625));
#43898=CARTESIAN_POINT('Ctrl Pts',(-66.,-1.46985115284591,-10.5616551809262));
#43899=CARTESIAN_POINT('Ctrl Pts',(-50.,-1.46985115284591,-10.5616551809262));
#43900=CARTESIAN_POINT('Ctrl Pts',(-66.,-1.51952729573235,-10.4590962775504));
#43901=CARTESIAN_POINT('Ctrl Pts',(-50.,-1.51952729573235,-10.4590962775504));
#43902=CARTESIAN_POINT('Ctrl Pts',(-66.,-1.56690236578525,-10.356191307998));
#43903=CARTESIAN_POINT('Ctrl Pts',(-50.,-1.56690236578525,-10.356191307998));
#43904=CARTESIAN_POINT('Ctrl Pts',(-66.,-1.6119202684502,-10.2529781942665));
#43905=CARTESIAN_POINT('Ctrl Pts',(-50.,-1.6119202684502,-10.2529781942665));
#43906=CARTESIAN_POINT('Ctrl Pts',(-66.,-1.65452632552406,-10.149499376492));
#43907=CARTESIAN_POINT('Ctrl Pts',(-50.,-1.65452632552406,-10.149499376492));
#43908=CARTESIAN_POINT('Ctrl Pts',(-66.,-1.69467032435451,-10.0458000163337));
#43909=CARTESIAN_POINT('Ctrl Pts',(-50.,-1.69467032435451,-10.0458000163337));
#43910=CARTESIAN_POINT('Ctrl Pts',(-66.,-1.73231249658609,-9.94192616811245));
#43911=CARTESIAN_POINT('Ctrl Pts',(-50.,-1.73231249658609,-9.94192616811245));
#43912=CARTESIAN_POINT('Ctrl Pts',(-66.,-1.76741704955006,-9.83792360466036));
#43913=CARTESIAN_POINT('Ctrl Pts',(-50.,-1.76741704955006,-9.83792360466036));
#43914=CARTESIAN_POINT('Ctrl Pts',(-66.,-1.79993935041505,-9.73383721479367));
#43915=CARTESIAN_POINT('Ctrl Pts',(-50.,-1.79993935041505,-9.73383721479367));
#43916=CARTESIAN_POINT('Ctrl Pts',(-66.,-1.82981529171165,-9.6297098958258));
#43917=CARTESIAN_POINT('Ctrl Pts',(-50.,-1.82981529171165,-9.6297098958258));
#43918=CARTESIAN_POINT('Ctrl Pts',(-66.,-1.85695006429591,-9.52558240518797));
#43919=CARTESIAN_POINT('Ctrl Pts',(-50.,-1.85695006429591,-9.52558240518797));
#43920=CARTESIAN_POINT('Ctrl Pts',(-66.,-1.8812070683013,-9.42149094310496));
#43921=CARTESIAN_POINT('Ctrl Pts',(-50.,-1.8812070683013,-9.42149094310496));
#43922=CARTESIAN_POINT('Ctrl Pts',(-66.,-1.90239869089103,-9.31747386945138));
#43923=CARTESIAN_POINT('Ctrl Pts',(-50.,-1.90239869089103,-9.31747386945138));
#43924=CARTESIAN_POINT('Ctrl Pts',(-66.,-1.92028072414509,-9.21358366430839));
#43925=CARTESIAN_POINT('Ctrl Pts',(-50.,-1.92028072414509,-9.21358366430839));
#43926=CARTESIAN_POINT('Ctrl Pts',(-66.,-1.93454224200995,-9.10989877492369));
#43927=CARTESIAN_POINT('Ctrl Pts',(-50.,-1.93454224200995,-9.10989877492369));
#43928=CARTESIAN_POINT('Ctrl Pts',(-66.,-1.94480508119479,-9.00653254085416));
#43929=CARTESIAN_POINT('Ctrl Pts',(-50.,-1.94480508119479,-9.00653254085416));
#43930=CARTESIAN_POINT('Ctrl Pts',(-66.,-1.95060005985058,-8.90365121100569));
#43931=CARTESIAN_POINT('Ctrl Pts',(-50.,-1.95060005985058,-8.90365121100569));
#43932=CARTESIAN_POINT('Ctrl Pts',(-66.,-1.95144243492538,-8.80145240736443));
#43933=CARTESIAN_POINT('Ctrl Pts',(-50.,-1.95144243492538,-8.80145240736443));
#43934=CARTESIAN_POINT('Ctrl Pts',(-66.,-1.94696330045856,-8.70012069286638));
#43935=CARTESIAN_POINT('Ctrl Pts',(-50.,-1.94696330045856,-8.70012069286638));
#43936=CARTESIAN_POINT('Ctrl Pts',(-66.,-1.9370325140864,-8.59978788146503));
#43937=CARTESIAN_POINT('Ctrl Pts',(-50.,-1.9370325140864,-8.59978788146503));
#43938=CARTESIAN_POINT('Ctrl Pts',(-66.,-1.92187017391035,-8.50049578112694));
#43939=CARTESIAN_POINT('Ctrl Pts',(-50.,-1.92187017391035,-8.50049578112694));
#43940=CARTESIAN_POINT('Ctrl Pts',(-66.,-1.90220797905422,-8.40214531049858));
#43941=CARTESIAN_POINT('Ctrl Pts',(-50.,-1.90220797905422,-8.40214531049858));
#43942=CARTESIAN_POINT('Ctrl Pts',(-66.,-1.87917718793209,-8.3045228175142));
#43943=CARTESIAN_POINT('Ctrl Pts',(-50.,-1.87917718793209,-8.3045228175142));
#43944=CARTESIAN_POINT('Ctrl Pts',(-66.,-1.85409889074508,-8.20735420592021));
#43945=CARTESIAN_POINT('Ctrl Pts',(-50.,-1.85409889074508,-8.20735420592021));
#43946=CARTESIAN_POINT('Ctrl Pts',(-66.,-1.8283040754312,-8.11035041561234));
#43947=CARTESIAN_POINT('Ctrl Pts',(-50.,-1.8283040754312,-8.11035041561234));
#43948=CARTESIAN_POINT('Ctrl Pts',(-66.,-1.80295075079726,-8.01325412885256));
#43949=CARTESIAN_POINT('Ctrl Pts',(-50.,-1.80295075079726,-8.01325412885256));
#43950=CARTESIAN_POINT('Ctrl Pts',(-66.,-1.77881844471932,-7.91589172108458));
#43951=CARTESIAN_POINT('Ctrl Pts',(-50.,-1.77881844471932,-7.91589172108458));
#43952=CARTESIAN_POINT('Ctrl Pts',(-66.,-1.75636195972324,-7.81816198995797));
#43953=CARTESIAN_POINT('Ctrl Pts',(-50.,-1.75636195972324,-7.81816198995797));
#43954=CARTESIAN_POINT('Ctrl Pts',(-66.,-1.73991571028055,-7.73964462612166));
#43955=CARTESIAN_POINT('Ctrl Pts',(-50.,-1.73991571028055,-7.73964462612166));
#43956=CARTESIAN_POINT('Ctrl Pts',(-66.,-1.7284661027293,-7.68056213071507));
#43957=CARTESIAN_POINT('Ctrl Pts',(-50.,-1.7284661027293,-7.68056213071507));
#43958=CARTESIAN_POINT('Ctrl Pts',(-66.,-1.72122591607555,-7.64108747345899));
#43959=CARTESIAN_POINT('Ctrl Pts',(-50.,-1.72122591607555,-7.64108747345899));
#43960=CARTESIAN_POINT('Ctrl Pts',(-66.,-1.71770404175134,-7.62132856363975));
#43961=CARTESIAN_POINT('Ctrl Pts',(-50.,-1.71770404175134,-7.62132856363975));
#43962=CARTESIAN_POINT('Ctrl Pts',(-50.,-1.71887666803992,-9.97803026654401));
#43963=CARTESIAN_POINT('Ctrl Pts',(-50.,-1.7214675353978,-9.97080469546511));
#43964=CARTESIAN_POINT('Ctrl Pts',(-50.,-1.73144934303076,-9.9427983603274));
#43965=CARTESIAN_POINT('Ctrl Pts',(-50.,-1.74843709680056,-9.89399008293484));
#43966=CARTESIAN_POINT('Ctrl Pts',(-50.,-1.77165950874705,-9.82434577497958));
#43967=CARTESIAN_POINT('Ctrl Pts',(-50.,-1.79993935041505,-9.73383721479367));
#43968=CARTESIAN_POINT('Ctrl Pts',(-50.,-1.82981529171165,-9.6297098958258));
#43969=CARTESIAN_POINT('Ctrl Pts',(-50.,-1.85695006429591,-9.52558240518797));
#43970=CARTESIAN_POINT('Ctrl Pts',(-50.,-1.8812070683013,-9.42149094310496));
#43971=CARTESIAN_POINT('Ctrl Pts',(-50.,-1.90239869089103,-9.31747386945138));
#43972=CARTESIAN_POINT('Ctrl Pts',(-50.,-1.92028072414509,-9.21358366430839));
#43973=CARTESIAN_POINT('Ctrl Pts',(-50.,-1.93454224200995,-9.10989877492369));
#43974=CARTESIAN_POINT('Ctrl Pts',(-50.,-1.94480508119479,-9.00653254085416));
#43975=CARTESIAN_POINT('Ctrl Pts',(-50.,-1.95060005985058,-8.90365121100569));
#43976=CARTESIAN_POINT('Ctrl Pts',(-50.,-1.95144243492538,-8.80145240736443));
#43977=CARTESIAN_POINT('Ctrl Pts',(-50.,-1.94696330045856,-8.70012069286638));
#43978=CARTESIAN_POINT('Ctrl Pts',(-50.,-1.9370325140864,-8.59978788146503));
#43979=CARTESIAN_POINT('Ctrl Pts',(-50.,-1.92187017391035,-8.50049578112694));
#43980=CARTESIAN_POINT('Ctrl Pts',(-50.,-1.90220797905422,-8.40214531049858));
#43981=CARTESIAN_POINT('Ctrl Pts',(-50.,-1.87917718793209,-8.3045228175142));
#43982=CARTESIAN_POINT('Ctrl Pts',(-50.,-1.85409889074508,-8.20735420592021));
#43983=CARTESIAN_POINT('Ctrl Pts',(-50.,-1.8283040754312,-8.11035041561234));
#43984=CARTESIAN_POINT('Ctrl Pts',(-50.,-1.80295075079726,-8.01325412885256));
#43985=CARTESIAN_POINT('Ctrl Pts',(-50.,-1.77881844471932,-7.91589172108458));
#43986=CARTESIAN_POINT('Ctrl Pts',(-50.,-1.75636195972324,-7.81816198995797));
#43987=CARTESIAN_POINT('Ctrl Pts',(-50.,-1.73991571028055,-7.73964462612166));
#43988=CARTESIAN_POINT('Ctrl Pts',(-50.,-1.7284661027293,-7.68056213071507));
#43989=CARTESIAN_POINT('Ctrl Pts',(-50.,-1.72122591607555,-7.64108747345899));
#43990=CARTESIAN_POINT('Ctrl Pts',(-50.,-1.71770404175134,-7.62132856363975));
#43991=CARTESIAN_POINT('Origin',(-50.,-2.46840926658957,-9.17984709653976));
#43992=CARTESIAN_POINT('Origin',(-50.,0.,0.));
#43993=CARTESIAN_POINT('Origin',(-65.75,0.,0.));
#43994=CARTESIAN_POINT('',(-65.5,-5.63978650350908,-9.00463398450136));
#43995=CARTESIAN_POINT('Origin',(-65.5,0.,0.));
#43996=CARTESIAN_POINT('',(-66.,-5.62870250745855,-8.41625410040178));
#43997=CARTESIAN_POINT('Ctrl Pts',(-65.5,-5.63978650350908,-9.00463398450135));
#43998=CARTESIAN_POINT('Ctrl Pts',(-65.6642917360001,-5.64651410229415,
-8.8065646438819));
#43999=CARTESIAN_POINT('Ctrl Pts',(-65.8311182354836,-5.64316254881277,
-8.60975308169117));
#44000=CARTESIAN_POINT('Ctrl Pts',(-66.,-5.62870250745855,-8.41625410040178));
#44001=CARTESIAN_POINT('Origin',(-66.,0.,0.));
#44002=CARTESIAN_POINT('Origin',(-58.,0.,0.));
#44003=CARTESIAN_POINT('',(-50.5,-5.63978650350908,-9.00463398450136));
#44004=CARTESIAN_POINT('Origin',(-50.5,0.,0.));
#44005=CARTESIAN_POINT('Ctrl Pts',(-50.5,-5.63978650350908,-9.00463398450136));
#44006=CARTESIAN_POINT('Ctrl Pts',(-55.5,-5.63978650350908,-9.00463398450136));
#44007=CARTESIAN_POINT('Ctrl Pts',(-60.5,-5.63978650350908,-9.00463398450136));
#44008=CARTESIAN_POINT('Ctrl Pts',(-65.5,-5.63978650350908,-9.00463398450136));
#44009=CARTESIAN_POINT('Origin',(-50.25,0.,0.));
#44010=CARTESIAN_POINT('',(-50.,-5.62870250745855,-8.4162541004018));
#44011=CARTESIAN_POINT('Origin',(-50.,0.,0.));
#44012=CARTESIAN_POINT('Ctrl Pts',(-50.,-5.62870250745855,-8.4162541004018));
#44013=CARTESIAN_POINT('Ctrl Pts',(-50.1688817645161,-5.64316254881275,
-8.6097530816908));
#44014=CARTESIAN_POINT('Ctrl Pts',(-50.3357082639996,-5.64651410229418,
-8.8065646438815));
#44015=CARTESIAN_POINT('Ctrl Pts',(-50.5,-5.63978650350908,-9.00463398450137));
#44016=CARTESIAN_POINT('Origin',(-66.,-5.98878426509152,-7.38221511806768));
#44017=CARTESIAN_POINT('',(-66.,-7.77316506323978,-6.48795267396646));
#44018=CARTESIAN_POINT('Origin',(-66.,0.,0.));
#44019=CARTESIAN_POINT('',(-66.,-4.66907432066882,-6.26377691477522));
#44020=CARTESIAN_POINT('Ctrl Pts',(-66.,-4.66907432066881,-6.26377691477523));
#44021=CARTESIAN_POINT('Ctrl Pts',(-66.,-4.6803283856108,-6.2803951017486));
#44022=CARTESIAN_POINT('Ctrl Pts',(-66.,-4.70299841481972,-6.3135121463621));
#44023=CARTESIAN_POINT('Ctrl Pts',(-66.,-4.73748916763617,-6.36282971672706));
#44024=CARTESIAN_POINT('Ctrl Pts',(-66.,-4.78444945309974,-6.42786960551628));
#44025=CARTESIAN_POINT('Ctrl Pts',(-66.,-4.84471473572967,-6.50801628214104));
#44026=CARTESIAN_POINT('Ctrl Pts',(-66.,-4.90636155322694,-6.5871457743388));
#44027=CARTESIAN_POINT('Ctrl Pts',(-66.,-4.96901558551421,-6.66553551990974));
#44028=CARTESIAN_POINT('Ctrl Pts',(-66.,-5.03203531791038,-6.74366119533008));
#44029=CARTESIAN_POINT('Ctrl Pts',(-66.,-5.09446751728307,-6.82222887666531));
#44030=CARTESIAN_POINT('Ctrl Pts',(-66.,-5.15521383698376,-6.90204399502655));
#44031=CARTESIAN_POINT('Ctrl Pts',(-66.,-5.21317888605016,-6.98389428559481));
#44032=CARTESIAN_POINT('Ctrl Pts',(-66.,-5.26741610862069,-7.06843505349409));
#44033=CARTESIAN_POINT('Ctrl Pts',(-66.,-5.31729736430153,-7.15605442289018));
#44034=CARTESIAN_POINT('Ctrl Pts',(-66.,-5.36260457863992,-7.2468037222681));
#44035=CARTESIAN_POINT('Ctrl Pts',(-66.,-5.40340302903612,-7.34050959992121));
#44036=CARTESIAN_POINT('Ctrl Pts',(-66.,-5.43995465934573,-7.43685340164567));
#44037=CARTESIAN_POINT('Ctrl Pts',(-66.,-5.47262192427873,-7.53545742801198));
#44038=CARTESIAN_POINT('Ctrl Pts',(-66.,-5.50176582326021,-7.63597896963706));
#44039=CARTESIAN_POINT('Ctrl Pts',(-66.,-5.52768572629587,-7.73816067281613));
#44040=CARTESIAN_POINT('Ctrl Pts',(-66.,-5.55063377109937,-7.84180440740311));
#44041=CARTESIAN_POINT('Ctrl Pts',(-66.,-5.57081170713472,-7.94676290214864));
#44042=CARTESIAN_POINT('Ctrl Pts',(-66.,-5.58837532489015,-8.0529248045481));
#44043=CARTESIAN_POINT('Ctrl Pts',(-66.,-5.60343469059531,-8.16020148387941));
#44044=CARTESIAN_POINT('Ctrl Pts',(-66.,-5.6144129176363,-8.25438761578178));
#44045=CARTESIAN_POINT('Ctrl Pts',(-66.,-5.62152508071414,-8.3274562628442));
#44046=CARTESIAN_POINT('Ctrl Pts',(-66.,-5.62585811032315,-8.37895438489326));
#44047=CARTESIAN_POINT('Ctrl Pts',(-66.,-5.62813047803977,-8.40859941207198));
#44048=CARTESIAN_POINT('Ctrl Pts',(-66.,-5.62870250745855,-8.41625410040178));
#44049=CARTESIAN_POINT('',(-66.,-5.74141212582432,-5.29823961815974));
#44050=CARTESIAN_POINT('Origin',(-66.,0.,0.));
#44051=CARTESIAN_POINT('Ctrl Pts',(-66.,-7.77316506323978,-6.48795267396646));
#44052=CARTESIAN_POINT('Ctrl Pts',(-66.,-7.75345510860632,-6.48528565401655));
#44053=CARTESIAN_POINT('Ctrl Pts',(-66.,-7.70743027026035,-6.47827106015396));
#44054=CARTESIAN_POINT('Ctrl Pts',(-66.,-7.63751204406767,-6.46467178276015));
#44055=CARTESIAN_POINT('Ctrl Pts',(-66.,-7.5470858877274,-6.4412452909937));
#44056=CARTESIAN_POINT('Ctrl Pts',(-66.,-7.43731124378912,-6.40616844479457));
#44057=CARTESIAN_POINT('Ctrl Pts',(-66.,-7.32147057295518,-6.3670183824321));
#44058=CARTESIAN_POINT('Ctrl Pts',(-66.,-7.20322406733259,-6.32776800725522));
#44059=CARTESIAN_POINT('Ctrl Pts',(-66.,-7.08315172769933,-6.28789592785851));
#44060=CARTESIAN_POINT('Ctrl Pts',(-66.,-6.96344139729801,-6.24564883963181));
#44061=CARTESIAN_POINT('Ctrl Pts',(-66.,-6.84694888377224,-6.19877182422175));
#44062=CARTESIAN_POINT('Ctrl Pts',(-66.,-6.73583542181789,-6.14555972644743));
#44063=CARTESIAN_POINT('Ctrl Pts',(-66.,-6.63088062115226,-6.08540012194724));
#44064=CARTESIAN_POINT('Ctrl Pts',(-66.,-6.53195203265778,-6.0184518231387));
#44065=CARTESIAN_POINT('Ctrl Pts',(-66.,-6.43823296078527,-5.9455012005935));
#44066=CARTESIAN_POINT('Ctrl Pts',(-66.,-6.34855221468005,-5.86775162582969));
#44067=CARTESIAN_POINT('Ctrl Pts',(-66.,-6.26163461373259,-5.78664724772762));
#44068=CARTESIAN_POINT('Ctrl Pts',(-66.,-6.17621252275219,-5.70369153841107));
#44069=CARTESIAN_POINT('Ctrl Pts',(-66.,-6.09114934394547,-5.62027514693155));
#44070=CARTESIAN_POINT('Ctrl Pts',(-66.,-6.00556552478208,-5.53749088454784));
#44071=CARTESIAN_POINT('Ctrl Pts',(-66.,-5.91894598825613,-5.45597826316371));
#44072=CARTESIAN_POINT('Ctrl Pts',(-66.,-5.84861777732304,-5.392038925661));
#44073=CARTESIAN_POINT('Ctrl Pts',(-66.,-5.79525461535482,-5.34484416215046));
#44074=CARTESIAN_POINT('Ctrl Pts',(-66.,-5.75940527114103,-5.31371825665548));
#44075=CARTESIAN_POINT('Ctrl Pts',(-66.,-5.74141212582432,-5.29823961815974));
#44076=CARTESIAN_POINT('Ctrl Pts',(-66.,-5.74141212582432,-5.29823961815974));
#44077=CARTESIAN_POINT('Ctrl Pts',(-50.,-5.74141212582432,-5.29823961815974));
#44078=CARTESIAN_POINT('Ctrl Pts',(-66.,-5.75940527114103,-5.31371825665548));
#44079=CARTESIAN_POINT('Ctrl Pts',(-50.,-5.75940527114103,-5.31371825665548));
#44080=CARTESIAN_POINT('Ctrl Pts',(-66.,-5.79525461535482,-5.34484416215046));
#44081=CARTESIAN_POINT('Ctrl Pts',(-50.,-5.79525461535482,-5.34484416215046));
#44082=CARTESIAN_POINT('Ctrl Pts',(-66.,-5.84861777732304,-5.392038925661));
#44083=CARTESIAN_POINT('Ctrl Pts',(-50.,-5.84861777732304,-5.392038925661));
#44084=CARTESIAN_POINT('Ctrl Pts',(-66.,-5.91894598825613,-5.45597826316371));
#44085=CARTESIAN_POINT('Ctrl Pts',(-50.,-5.91894598825613,-5.45597826316371));
#44086=CARTESIAN_POINT('Ctrl Pts',(-66.,-6.00556552478208,-5.53749088454784));
#44087=CARTESIAN_POINT('Ctrl Pts',(-50.,-6.00556552478208,-5.53749088454784));
#44088=CARTESIAN_POINT('Ctrl Pts',(-66.,-6.09114934394547,-5.62027514693155));
#44089=CARTESIAN_POINT('Ctrl Pts',(-50.,-6.09114934394547,-5.62027514693155));
#44090=CARTESIAN_POINT('Ctrl Pts',(-66.,-6.17621252275219,-5.70369153841107));
#44091=CARTESIAN_POINT('Ctrl Pts',(-50.,-6.17621252275219,-5.70369153841107));
#44092=CARTESIAN_POINT('Ctrl Pts',(-66.,-6.26163461373259,-5.78664724772762));
#44093=CARTESIAN_POINT('Ctrl Pts',(-50.,-6.26163461373259,-5.78664724772762));
#44094=CARTESIAN_POINT('Ctrl Pts',(-66.,-6.34855221468005,-5.86775162582969));
#44095=CARTESIAN_POINT('Ctrl Pts',(-50.,-6.34855221468005,-5.86775162582969));
#44096=CARTESIAN_POINT('Ctrl Pts',(-66.,-6.43823296078527,-5.9455012005935));
#44097=CARTESIAN_POINT('Ctrl Pts',(-50.,-6.43823296078527,-5.9455012005935));
#44098=CARTESIAN_POINT('Ctrl Pts',(-66.,-6.53195203265778,-6.0184518231387));
#44099=CARTESIAN_POINT('Ctrl Pts',(-50.,-6.53195203265778,-6.0184518231387));
#44100=CARTESIAN_POINT('Ctrl Pts',(-66.,-6.63088062115226,-6.08540012194724));
#44101=CARTESIAN_POINT('Ctrl Pts',(-50.,-6.63088062115226,-6.08540012194724));
#44102=CARTESIAN_POINT('Ctrl Pts',(-66.,-6.73583542181789,-6.14555972644743));
#44103=CARTESIAN_POINT('Ctrl Pts',(-50.,-6.73583542181789,-6.14555972644743));
#44104=CARTESIAN_POINT('Ctrl Pts',(-66.,-6.84694888377224,-6.19877182422175));
#44105=CARTESIAN_POINT('Ctrl Pts',(-50.,-6.84694888377224,-6.19877182422175));
#44106=CARTESIAN_POINT('Ctrl Pts',(-66.,-6.96344139729801,-6.24564883963181));
#44107=CARTESIAN_POINT('Ctrl Pts',(-50.,-6.96344139729801,-6.24564883963181));
#44108=CARTESIAN_POINT('Ctrl Pts',(-66.,-7.08315172769933,-6.28789592785851));
#44109=CARTESIAN_POINT('Ctrl Pts',(-50.,-7.08315172769933,-6.28789592785851));
#44110=CARTESIAN_POINT('Ctrl Pts',(-66.,-7.20322406733259,-6.32776800725522));
#44111=CARTESIAN_POINT('Ctrl Pts',(-50.,-7.20322406733259,-6.32776800725522));
#44112=CARTESIAN_POINT('Ctrl Pts',(-66.,-7.32147057295518,-6.3670183824321));
#44113=CARTESIAN_POINT('Ctrl Pts',(-50.,-7.32147057295518,-6.3670183824321));
#44114=CARTESIAN_POINT('Ctrl Pts',(-66.,-7.43731124378912,-6.40616844479457));
#44115=CARTESIAN_POINT('Ctrl Pts',(-50.,-7.43731124378912,-6.40616844479457));
#44116=CARTESIAN_POINT('Ctrl Pts',(-66.,-7.553391455313,-6.44326014083938));
#44117=CARTESIAN_POINT('Ctrl Pts',(-50.,-7.553391455313,-6.44326014083938));
#44118=CARTESIAN_POINT('Ctrl Pts',(-66.,-7.6750361184554,-6.47426301701044));
#44119=CARTESIAN_POINT('Ctrl Pts',(-50.,-7.6750361184554,-6.47426301701044));
#44120=CARTESIAN_POINT('Ctrl Pts',(-66.,-7.80719134625564,-6.49540273802627));
#44121=CARTESIAN_POINT('Ctrl Pts',(-50.,-7.80719134625564,-6.49540273802627));
#44122=CARTESIAN_POINT('Ctrl Pts',(-66.,-7.95216837696596,-6.50487707558157));
#44123=CARTESIAN_POINT('Ctrl Pts',(-50.,-7.95216837696596,-6.50487707558157));
#44124=CARTESIAN_POINT('Ctrl Pts',(-66.,-8.10672179348113,-6.5050783470944));
#44125=CARTESIAN_POINT('Ctrl Pts',(-50.,-8.10672179348113,-6.5050783470944));
#44126=CARTESIAN_POINT('Ctrl Pts',(-66.,-8.2603690870727,-6.5038743097965));
#44127=CARTESIAN_POINT('Ctrl Pts',(-50.,-8.2603690870727,-6.5038743097965));
#44128=CARTESIAN_POINT('Ctrl Pts',(-66.,-8.39837287749729,-6.51235531359857));
#44129=CARTESIAN_POINT('Ctrl Pts',(-50.,-8.39837287749729,-6.51235531359857));
#44130=CARTESIAN_POINT('Ctrl Pts',(-66.,-8.50407985685393,-6.54306925405535));
#44131=CARTESIAN_POINT('Ctrl Pts',(-50.,-8.50407985685393,-6.54306925405535));
#44132=CARTESIAN_POINT('Ctrl Pts',(-66.,-8.5614051848243,-6.60814607044284));
#44133=CARTESIAN_POINT('Ctrl Pts',(-50.,-8.5614051848243,-6.60814607044284));
#44134=CARTESIAN_POINT('Ctrl Pts',(-66.,-8.55749728553057,-6.71728694922543));
#44135=CARTESIAN_POINT('Ctrl Pts',(-50.,-8.55749728553057,-6.71728694922543));
#44136=CARTESIAN_POINT('Ctrl Pts',(-66.,-8.48260119723272,-6.87786491540434));
#44137=CARTESIAN_POINT('Ctrl Pts',(-50.,-8.48260119723272,-6.87786491540434));
#44138=CARTESIAN_POINT('Ctrl Pts',(-66.,-8.32952523731861,-7.09532467445007));
#44139=CARTESIAN_POINT('Ctrl Pts',(-50.,-8.32952523731861,-7.09532467445007));
#44140=CARTESIAN_POINT('Ctrl Pts',(-66.,-8.0932717341967,-7.37345895158545));
#44141=CARTESIAN_POINT('Ctrl Pts',(-50.,-8.0932717341967,-7.37345895158545));
#44142=CARTESIAN_POINT('Ctrl Pts',(-66.,-7.77062057842988,-7.7147205817437));
#44143=CARTESIAN_POINT('Ctrl Pts',(-50.,-7.77062057842988,-7.7147205817437));
#44144=CARTESIAN_POINT('Ctrl Pts',(-66.,-7.35975359139894,-8.12050399689911));
#44145=CARTESIAN_POINT('Ctrl Pts',(-50.,-7.35975359139894,-8.12050399689911));
#44146=CARTESIAN_POINT('Ctrl Pts',(-66.,-6.85988010667493,-8.59142596067649));
#44147=CARTESIAN_POINT('Ctrl Pts',(-50.,-6.85988010667493,-8.59142596067649));
#44148=CARTESIAN_POINT('Ctrl Pts',(-66.,-6.38867920626058,-9.02036044814632));
#44149=CARTESIAN_POINT('Ctrl Pts',(-50.,-6.38867920626058,-9.02036044814632));
#44150=CARTESIAN_POINT('Ctrl Pts',(-66.,-5.99526031433169,-9.37135959104543));
#44151=CARTESIAN_POINT('Ctrl Pts',(-50.,-5.99526031433169,-9.37135959104543));
#44152=CARTESIAN_POINT('Ctrl Pts',(-66.,-5.71521882289448,-9.61836316580793));
#44153=CARTESIAN_POINT('Ctrl Pts',(-50.,-5.71521882289448,-9.61836316580793));
#44154=CARTESIAN_POINT('Ctrl Pts',(-66.,-5.57075751837199,-9.74511599066435));
#44155=CARTESIAN_POINT('Ctrl Pts',(-50.,-5.57075751837199,-9.74511599066435));
#44156=CARTESIAN_POINT('',(-65.5,-8.39084402103177,-6.51800288544853));
#44157=CARTESIAN_POINT('Ctrl Pts',(-66.,-7.77316506323978,-6.48795267396645));
#44158=CARTESIAN_POINT('Ctrl Pts',(-65.7982417703064,-8.00929789807026,
-6.51990459841432));
#44159=CARTESIAN_POINT('Ctrl Pts',(-65.6331946192803,-8.24208515110479,
-6.49238455442199));
#44160=CARTESIAN_POINT('Ctrl Pts',(-65.5,-8.39084402103177,-6.51800288544853));
#44161=CARTESIAN_POINT('',(-50.,-5.74141212582432,-5.29823961815974));
#44162=CARTESIAN_POINT('',(-66.,-5.74141212582432,-5.29823961815974));
#44163=CARTESIAN_POINT('',(-50.,-7.7731650632398,-6.48795267396646));
#44164=CARTESIAN_POINT('Ctrl Pts',(-50.,-5.74141212582432,-5.29823961815974));
#44165=CARTESIAN_POINT('Ctrl Pts',(-50.,-5.75940527114103,-5.31371825665548));
#44166=CARTESIAN_POINT('Ctrl Pts',(-50.,-5.79525461535482,-5.34484416215046));
#44167=CARTESIAN_POINT('Ctrl Pts',(-50.,-5.84861777732304,-5.392038925661));
#44168=CARTESIAN_POINT('Ctrl Pts',(-50.,-5.91894598825613,-5.45597826316371));
#44169=CARTESIAN_POINT('Ctrl Pts',(-50.,-6.00556552478208,-5.53749088454784));
#44170=CARTESIAN_POINT('Ctrl Pts',(-50.,-6.09114934394547,-5.62027514693155));
#44171=CARTESIAN_POINT('Ctrl Pts',(-50.,-6.17621252275219,-5.70369153841107));
#44172=CARTESIAN_POINT('Ctrl Pts',(-50.,-6.26163461373259,-5.78664724772762));
#44173=CARTESIAN_POINT('Ctrl Pts',(-50.,-6.34855221468005,-5.86775162582969));
#44174=CARTESIAN_POINT('Ctrl Pts',(-50.,-6.43823296078527,-5.9455012005935));
#44175=CARTESIAN_POINT('Ctrl Pts',(-50.,-6.53195203265778,-6.0184518231387));
#44176=CARTESIAN_POINT('Ctrl Pts',(-50.,-6.63088062115226,-6.08540012194724));
#44177=CARTESIAN_POINT('Ctrl Pts',(-50.,-6.73583542181789,-6.14555972644743));
#44178=CARTESIAN_POINT('Ctrl Pts',(-50.,-6.84694888377224,-6.19877182422175));
#44179=CARTESIAN_POINT('Ctrl Pts',(-50.,-6.96344139729801,-6.24564883963181));
#44180=CARTESIAN_POINT('Ctrl Pts',(-50.,-7.08315172769933,-6.28789592785851));
#44181=CARTESIAN_POINT('Ctrl Pts',(-50.,-7.20322406733259,-6.32776800725522));
#44182=CARTESIAN_POINT('Ctrl Pts',(-50.,-7.32147057295518,-6.3670183824321));
#44183=CARTESIAN_POINT('Ctrl Pts',(-50.,-7.43731124378912,-6.40616844479457));
#44184=CARTESIAN_POINT('Ctrl Pts',(-50.,-7.54708588772741,-6.44124529099371));
#44185=CARTESIAN_POINT('Ctrl Pts',(-50.,-7.63751204406767,-6.46467178276015));
#44186=CARTESIAN_POINT('Ctrl Pts',(-50.,-7.70743027026036,-6.47827106015396));
#44187=CARTESIAN_POINT('Ctrl Pts',(-50.,-7.75345510860633,-6.48528565401655));
#44188=CARTESIAN_POINT('Ctrl Pts',(-50.,-7.7731650632398,-6.48795267396646));
#44189=CARTESIAN_POINT('',(-50.5,-8.39084402103177,-6.51800288544853));
#44190=CARTESIAN_POINT('Ctrl Pts',(-50.5,-8.39084402103178,-6.51800288544854));
#44191=CARTESIAN_POINT('Ctrl Pts',(-50.49825670698,-8.38889701820982,-6.5176675846841));
#44192=CARTESIAN_POINT('Ctrl Pts',(-50.4965113438761,-8.3869400955467,-6.51734148071378));
#44193=CARTESIAN_POINT('Ctrl Pts',(-50.3581212730775,-8.23119318026662,
-6.49221711279462));
#44194=CARTESIAN_POINT('Ctrl Pts',(-50.2022201285458,-8.00983849304637,
-6.51997774813044));
#44195=CARTESIAN_POINT('Ctrl Pts',(-50.,-7.7731650632398,-6.48795267396646));
#44196=CARTESIAN_POINT('Ctrl Pts',(-65.5,-8.39084402103177,-6.51800288544853));
#44197=CARTESIAN_POINT('Ctrl Pts',(-60.5,-8.39084402103177,-6.51800288544853));
#44198=CARTESIAN_POINT('Ctrl Pts',(-55.5,-8.39084402103177,-6.51800288544853));
#44199=CARTESIAN_POINT('Ctrl Pts',(-50.5,-8.39084402103177,-6.51800288544853));
#44200=CARTESIAN_POINT('Origin',(-66.,0.,0.));
#44201=CARTESIAN_POINT('',(-50.,-4.66907432066882,-6.26377691477522));
#44202=CARTESIAN_POINT('',(-66.,-4.66907432066882,-6.26377691477522));
#44203=CARTESIAN_POINT('Origin',(-50.,0.,0.));
#44204=CARTESIAN_POINT('Ctrl Pts',(-66.,-5.57075751837199,-9.74511599066435));
#44205=CARTESIAN_POINT('Ctrl Pts',(-50.,-5.57075751837199,-9.74511599066435));
#44206=CARTESIAN_POINT('Ctrl Pts',(-66.,-5.57426393082888,-9.72168709959797));
#44207=CARTESIAN_POINT('Ctrl Pts',(-50.,-5.57426393082888,-9.72168709959797));
#44208=CARTESIAN_POINT('Ctrl Pts',(-66.,-5.58106838195346,-9.67487582524648));
#44209=CARTESIAN_POINT('Ctrl Pts',(-50.,-5.58106838195346,-9.67487582524648));
#44210=CARTESIAN_POINT('Ctrl Pts',(-66.,-5.59064993734473,-9.60479843730945));
#44211=CARTESIAN_POINT('Ctrl Pts',(-50.,-5.59064993734473,-9.60479843730945));
#44212=CARTESIAN_POINT('Ctrl Pts',(-66.,-5.60217343871804,-9.51164133615758));
#44213=CARTESIAN_POINT('Ctrl Pts',(-50.,-5.60217343871804,-9.51164133615758));
#44214=CARTESIAN_POINT('Ctrl Pts',(-66.,-5.61447940680167,-9.39566548360896));
#44215=CARTESIAN_POINT('Ctrl Pts',(-50.,-5.61447940680167,-9.39566548360896));
#44216=CARTESIAN_POINT('Ctrl Pts',(-66.,-5.62466805596007,-9.28017086568711));
#44217=CARTESIAN_POINT('Ctrl Pts',(-50.,-5.62466805596007,-9.28017086568711));
#44218=CARTESIAN_POINT('Ctrl Pts',(-66.,-5.63271431565661,-9.16517615840736));
#44219=CARTESIAN_POINT('Ctrl Pts',(-50.,-5.63271431565661,-9.16517615840736));
#44220=CARTESIAN_POINT('Ctrl Pts',(-66.,-5.63858801770719,-9.05070979199298));
#44221=CARTESIAN_POINT('Ctrl Pts',(-50.,-5.63858801770719,-9.05070979199298));
#44222=CARTESIAN_POINT('Ctrl Pts',(-66.,-5.64225496831767,-8.93681246407458));
#44223=CARTESIAN_POINT('Ctrl Pts',(-50.,-5.64225496831767,-8.93681246407458));
#44224=CARTESIAN_POINT('Ctrl Pts',(-66.,-5.64367902649844,-8.82353491961232));
#44225=CARTESIAN_POINT('Ctrl Pts',(-50.,-5.64367902649844,-8.82353491961232));
#44226=CARTESIAN_POINT('Ctrl Pts',(-66.,-5.64282437159007,-8.71093461778555));
#44227=CARTESIAN_POINT('Ctrl Pts',(-50.,-5.64282437159007,-8.71093461778555));
#44228=CARTESIAN_POINT('Ctrl Pts',(-66.,-5.63965831452689,-8.5990725692165));
#44229=CARTESIAN_POINT('Ctrl Pts',(-50.,-5.63965831452689,-8.5990725692165));
#44230=CARTESIAN_POINT('Ctrl Pts',(-66.,-5.63415335267014,-8.48801045445945));
#44231=CARTESIAN_POINT('Ctrl Pts',(-50.,-5.63415335267014,-8.48801045445945));
#44232=CARTESIAN_POINT('Ctrl Pts',(-66.,-5.62629188779924,-8.37780652147756));
#44233=CARTESIAN_POINT('Ctrl Pts',(-50.,-5.62629188779924,-8.37780652147756));
#44234=CARTESIAN_POINT('Ctrl Pts',(-66.,-5.61605983917227,-8.26851714402347));
#44235=CARTESIAN_POINT('Ctrl Pts',(-50.,-5.61605983917227,-8.26851714402347));
#44236=CARTESIAN_POINT('Ctrl Pts',(-66.,-5.60343469059531,-8.16020148387941));
#44237=CARTESIAN_POINT('Ctrl Pts',(-50.,-5.60343469059531,-8.16020148387941));
#44238=CARTESIAN_POINT('Ctrl Pts',(-66.,-5.58837532489015,-8.0529248045481));
#44239=CARTESIAN_POINT('Ctrl Pts',(-50.,-5.58837532489015,-8.0529248045481));
#44240=CARTESIAN_POINT('Ctrl Pts',(-66.,-5.57081170713472,-7.94676290214864));
#44241=CARTESIAN_POINT('Ctrl Pts',(-50.,-5.57081170713472,-7.94676290214864));
#44242=CARTESIAN_POINT('Ctrl Pts',(-66.,-5.55063377109937,-7.84180440740311));
#44243=CARTESIAN_POINT('Ctrl Pts',(-50.,-5.55063377109937,-7.84180440740311));
#44244=CARTESIAN_POINT('Ctrl Pts',(-66.,-5.52768572629587,-7.73816067281613));
#44245=CARTESIAN_POINT('Ctrl Pts',(-50.,-5.52768572629587,-7.73816067281613));
#44246=CARTESIAN_POINT('Ctrl Pts',(-66.,-5.50176582326021,-7.63597896963706));
#44247=CARTESIAN_POINT('Ctrl Pts',(-50.,-5.50176582326021,-7.63597896963706));
#44248=CARTESIAN_POINT('Ctrl Pts',(-66.,-5.47262192427873,-7.53545742801198));
#44249=CARTESIAN_POINT('Ctrl Pts',(-50.,-5.47262192427873,-7.53545742801198));
#44250=CARTESIAN_POINT('Ctrl Pts',(-66.,-5.43995465934573,-7.43685340164567));
#44251=CARTESIAN_POINT('Ctrl Pts',(-50.,-5.43995465934573,-7.43685340164567));
#44252=CARTESIAN_POINT('Ctrl Pts',(-66.,-5.40340302903612,-7.34050959992121));
#44253=CARTESIAN_POINT('Ctrl Pts',(-50.,-5.40340302903612,-7.34050959992121));
#44254=CARTESIAN_POINT('Ctrl Pts',(-66.,-5.36260457863992,-7.2468037222681));
#44255=CARTESIAN_POINT('Ctrl Pts',(-50.,-5.36260457863992,-7.2468037222681));
#44256=CARTESIAN_POINT('Ctrl Pts',(-66.,-5.31729736430153,-7.15605442289018));
#44257=CARTESIAN_POINT('Ctrl Pts',(-50.,-5.31729736430153,-7.15605442289018));
#44258=CARTESIAN_POINT('Ctrl Pts',(-66.,-5.26741610862069,-7.06843505349409));
#44259=CARTESIAN_POINT('Ctrl Pts',(-50.,-5.26741610862069,-7.06843505349409));
#44260=CARTESIAN_POINT('Ctrl Pts',(-66.,-5.21317888605016,-6.98389428559481));
#44261=CARTESIAN_POINT('Ctrl Pts',(-50.,-5.21317888605016,-6.98389428559481));
#44262=CARTESIAN_POINT('Ctrl Pts',(-66.,-5.15521383698376,-6.90204399502655));
#44263=CARTESIAN_POINT('Ctrl Pts',(-50.,-5.15521383698376,-6.90204399502655));
#44264=CARTESIAN_POINT('Ctrl Pts',(-66.,-5.09446751728307,-6.82222887666531));
#44265=CARTESIAN_POINT('Ctrl Pts',(-50.,-5.09446751728307,-6.82222887666531));
#44266=CARTESIAN_POINT('Ctrl Pts',(-66.,-5.03203531791038,-6.74366119533008));
#44267=CARTESIAN_POINT('Ctrl Pts',(-50.,-5.03203531791038,-6.74366119533008));
#44268=CARTESIAN_POINT('Ctrl Pts',(-66.,-4.96901558551421,-6.66553551990974));
#44269=CARTESIAN_POINT('Ctrl Pts',(-50.,-4.96901558551421,-6.66553551990974));
#44270=CARTESIAN_POINT('Ctrl Pts',(-66.,-4.90636155322694,-6.5871457743388));
#44271=CARTESIAN_POINT('Ctrl Pts',(-50.,-4.90636155322694,-6.5871457743388));
#44272=CARTESIAN_POINT('Ctrl Pts',(-66.,-4.84471473572967,-6.50801628214104));
#44273=CARTESIAN_POINT('Ctrl Pts',(-50.,-4.84471473572967,-6.50801628214104));
#44274=CARTESIAN_POINT('Ctrl Pts',(-66.,-4.78444945309974,-6.42786960551628));
#44275=CARTESIAN_POINT('Ctrl Pts',(-50.,-4.78444945309974,-6.42786960551628));
#44276=CARTESIAN_POINT('Ctrl Pts',(-66.,-4.73748916763617,-6.36282971672706));
#44277=CARTESIAN_POINT('Ctrl Pts',(-50.,-4.73748916763617,-6.36282971672706));
#44278=CARTESIAN_POINT('Ctrl Pts',(-66.,-4.70299841481972,-6.3135121463621));
#44279=CARTESIAN_POINT('Ctrl Pts',(-50.,-4.70299841481972,-6.3135121463621));
#44280=CARTESIAN_POINT('Ctrl Pts',(-66.,-4.6803283856108,-6.2803951017486));
#44281=CARTESIAN_POINT('Ctrl Pts',(-50.,-4.6803283856108,-6.2803951017486));
#44282=CARTESIAN_POINT('Ctrl Pts',(-66.,-4.66907432066881,-6.26377691477523));
#44283=CARTESIAN_POINT('Ctrl Pts',(-50.,-4.66907432066881,-6.26377691477523));
#44284=CARTESIAN_POINT('Ctrl Pts',(-50.,-5.62870250745855,-8.4162541004018));
#44285=CARTESIAN_POINT('Ctrl Pts',(-50.,-5.62813047803977,-8.40859941207199));
#44286=CARTESIAN_POINT('Ctrl Pts',(-50.,-5.62585811032315,-8.37895438489327));
#44287=CARTESIAN_POINT('Ctrl Pts',(-50.,-5.62152508071414,-8.3274562628442));
#44288=CARTESIAN_POINT('Ctrl Pts',(-50.,-5.6144129176363,-8.25438761578178));
#44289=CARTESIAN_POINT('Ctrl Pts',(-50.,-5.60343469059531,-8.16020148387941));
#44290=CARTESIAN_POINT('Ctrl Pts',(-50.,-5.58837532489015,-8.0529248045481));
#44291=CARTESIAN_POINT('Ctrl Pts',(-50.,-5.57081170713472,-7.94676290214864));
#44292=CARTESIAN_POINT('Ctrl Pts',(-50.,-5.55063377109937,-7.84180440740311));
#44293=CARTESIAN_POINT('Ctrl Pts',(-50.,-5.52768572629587,-7.73816067281613));
#44294=CARTESIAN_POINT('Ctrl Pts',(-50.,-5.50176582326021,-7.63597896963706));
#44295=CARTESIAN_POINT('Ctrl Pts',(-50.,-5.47262192427873,-7.53545742801198));
#44296=CARTESIAN_POINT('Ctrl Pts',(-50.,-5.43995465934573,-7.43685340164567));
#44297=CARTESIAN_POINT('Ctrl Pts',(-50.,-5.40340302903612,-7.34050959992121));
#44298=CARTESIAN_POINT('Ctrl Pts',(-50.,-5.36260457863992,-7.2468037222681));
#44299=CARTESIAN_POINT('Ctrl Pts',(-50.,-5.31729736430153,-7.15605442289018));
#44300=CARTESIAN_POINT('Ctrl Pts',(-50.,-5.26741610862069,-7.06843505349409));
#44301=CARTESIAN_POINT('Ctrl Pts',(-50.,-5.21317888605016,-6.98389428559481));
#44302=CARTESIAN_POINT('Ctrl Pts',(-50.,-5.15521383698376,-6.90204399502655));
#44303=CARTESIAN_POINT('Ctrl Pts',(-50.,-5.09446751728307,-6.82222887666531));
#44304=CARTESIAN_POINT('Ctrl Pts',(-50.,-5.03203531791038,-6.74366119533008));
#44305=CARTESIAN_POINT('Ctrl Pts',(-50.,-4.96901558551421,-6.66553551990974));
#44306=CARTESIAN_POINT('Ctrl Pts',(-50.,-4.90636155322694,-6.5871457743388));
#44307=CARTESIAN_POINT('Ctrl Pts',(-50.,-4.84471473572967,-6.50801628214104));
#44308=CARTESIAN_POINT('Ctrl Pts',(-50.,-4.78444945309974,-6.42786960551628));
#44309=CARTESIAN_POINT('Ctrl Pts',(-50.,-4.73748916763617,-6.36282971672706));
#44310=CARTESIAN_POINT('Ctrl Pts',(-50.,-4.70299841481972,-6.3135121463621));
#44311=CARTESIAN_POINT('Ctrl Pts',(-50.,-4.6803283856108,-6.2803951017486));
#44312=CARTESIAN_POINT('Ctrl Pts',(-50.,-4.66907432066881,-6.26377691477523));
#44313=CARTESIAN_POINT('Origin',(-50.,-5.98878426509152,-7.38221511806768));
#44314=CARTESIAN_POINT('Origin',(-50.,0.,0.));
#44315=CARTESIAN_POINT('Origin',(-65.75,0.,0.));
#44316=CARTESIAN_POINT('',(-65.5,-8.81471594133711,-5.93223464417393));
#44317=CARTESIAN_POINT('Origin',(-65.5,0.,0.));
#44318=CARTESIAN_POINT('',(-66.,-8.56527454818064,-5.39923114103193));
#44319=CARTESIAN_POINT('Ctrl Pts',(-65.5,-8.81471594133711,-5.93223464417392));
#44320=CARTESIAN_POINT('Ctrl Pts',(-65.6642917360001,-8.74029984994827,
-5.74855293680691));
#44321=CARTESIAN_POINT('Ctrl Pts',(-65.8311182354827,-8.6571875793658,-5.57011982776901));
#44322=CARTESIAN_POINT('Ctrl Pts',(-66.,-8.56527454818064,-5.39923114103193));
#44323=CARTESIAN_POINT('Origin',(-66.,0.,0.));
#44324=CARTESIAN_POINT('Origin',(-58.,0.,0.));
#44325=CARTESIAN_POINT('',(-50.5,-8.81471594133712,-5.93223464417392));
#44326=CARTESIAN_POINT('Origin',(-50.5,0.,0.));
#44327=CARTESIAN_POINT('Ctrl Pts',(-50.5,-8.81471594133712,-5.93223464417392));
#44328=CARTESIAN_POINT('Ctrl Pts',(-55.5,-8.81471594133712,-5.93223464417392));
#44329=CARTESIAN_POINT('Ctrl Pts',(-60.5,-8.81471594133712,-5.93223464417392));
#44330=CARTESIAN_POINT('Ctrl Pts',(-65.5,-8.81471594133712,-5.93223464417392));
#44331=CARTESIAN_POINT('Origin',(-50.25,0.,0.));
#44332=CARTESIAN_POINT('',(-50.,-8.56527454818065,-5.39923114103194));
#44333=CARTESIAN_POINT('Origin',(-50.,0.,0.));
#44334=CARTESIAN_POINT('Ctrl Pts',(-50.,-8.56527454818065,-5.39923114103195));
#44335=CARTESIAN_POINT('Ctrl Pts',(-50.1688817645164,-8.65718757936533,
-5.57011982776812));
#44336=CARTESIAN_POINT('Ctrl Pts',(-50.335708263999,-8.74029984994787,-5.74855293680593));
#44337=CARTESIAN_POINT('Ctrl Pts',(-50.5,-8.81471594133712,-5.93223464417393));
#44338=CARTESIAN_POINT('Origin',(-66.,-8.4736440577621,-4.30813108036277));
#44339=CARTESIAN_POINT('',(-66.,-9.74002772607264,-2.76540863080598));
#44340=CARTESIAN_POINT('Origin',(-66.,0.,0.));
#44341=CARTESIAN_POINT('',(-66.,-6.81311923233408,-3.82316133271923));
#44342=CARTESIAN_POINT('Ctrl Pts',(-66.,-6.81311923233407,-3.82316133271924));
#44343=CARTESIAN_POINT('Ctrl Pts',(-66.,-6.8301595578254,-3.83376536134756));
#44344=CARTESIAN_POINT('Ctrl Pts',(-66.,-6.86433957558852,-3.8547985554459));
#44345=CARTESIAN_POINT('Ctrl Pts',(-66.,-6.91590770916956,-3.88582374481706));
#44346=CARTESIAN_POINT('Ctrl Pts',(-66.,-6.98526217067656,-3.92614017091869));
#44347=CARTESIAN_POINT('Ctrl Pts',(-66.,-7.0729158360807,-3.97484570454348));
#44348=CARTESIAN_POINT('Ctrl Pts',(-66.,-7.16141787020827,-4.02206007310117));
#44349=CARTESIAN_POINT('Ctrl Pts',(-66.,-7.25053915877239,-4.06818897832557));
#44350=CARTESIAN_POINT('Ctrl Pts',(-66.,-7.33988712400327,-4.11392789982873));
#44351=CARTESIAN_POINT('Ctrl Pts',(-66.,-7.42887813111136,-4.16030958503735));
#44352=CARTESIAN_POINT('Ctrl Pts',(-66.,-7.51683638885138,-4.2085165697132));
#44353=CARTESIAN_POINT('Ctrl Pts',(-66.,-7.60308160854854,-4.25971402139557));
#44354=CARTESIAN_POINT('Ctrl Pts',(-66.,-7.68701560500139,-4.31488559005748));
#44355=CARTESIAN_POINT('Ctrl Pts',(-66.,-7.76822240772673,-4.37464133248276));
#44356=CARTESIAN_POINT('Ctrl Pts',(-66.,-7.84652367297445,-4.43911683844659));
#44357=CARTESIAN_POINT('Ctrl Pts',(-66.,-7.92190852612585,-4.50812719257416));
#44358=CARTESIAN_POINT('Ctrl Pts',(-66.,-7.9944866564592,-4.58127474760048));
#44359=CARTESIAN_POINT('Ctrl Pts',(-66.,-8.06443555863034,-4.65806703431538));
#44360=CARTESIAN_POINT('Ctrl Pts',(-66.,-8.13194562956026,-4.73804414042434));
#44361=CARTESIAN_POINT('Ctrl Pts',(-66.,-8.19718568217584,-4.82084919686819));
#44362=CARTESIAN_POINT('Ctrl Pts',(-66.,-8.26030546894961,-4.90619864910471));
#44363=CARTESIAN_POINT('Ctrl Pts',(-66.,-8.32142939657439,-4.99387589925328));
#44364=CARTESIAN_POINT('Ctrl Pts',(-66.,-8.38065449559913,-5.08371585603889));
#44365=CARTESIAN_POINT('Ctrl Pts',(-66.,-8.43804526716559,-5.17559278329922));
#44366=CARTESIAN_POINT('Ctrl Pts',(-66.,-8.48638332772613,-5.25717084905798));
#44367=CARTESIAN_POINT('Ctrl Pts',(-66.,-8.52260030822015,-5.32102960234266));
#44368=CARTESIAN_POINT('Ctrl Pts',(-66.,-8.54750490102424,-5.36631307590019));
#44369=CARTESIAN_POINT('Ctrl Pts',(-66.,-8.56163853106841,-5.39247090060411));
#44370=CARTESIAN_POINT('Ctrl Pts',(-66.,-8.56527454818064,-5.39923114103193));
#44371=CARTESIAN_POINT('',(-66.,-7.40002916450246,-2.50494004209942));
#44372=CARTESIAN_POINT('Origin',(-66.,0.,0.));
#44373=CARTESIAN_POINT('Ctrl Pts',(-66.,-9.74002772607264,-2.76540863080598));
#44374=CARTESIAN_POINT('Ctrl Pts',(-66.,-9.72093701180546,-2.7709889476281));
#44375=CARTESIAN_POINT('Ctrl Pts',(-66.,-9.67603813743555,-2.78330078551466));
#44376=CARTESIAN_POINT('Ctrl Pts',(-66.,-9.60663333505538,-2.79931553203575));
#44377=CARTESIAN_POINT('Ctrl Pts',(-66.,-9.51449651805853,-2.8146939981701));
#44378=CARTESIAN_POINT('Ctrl Pts',(-66.,-9.39994535205166,-2.82729907482675));
#44379=CARTESIAN_POINT('Ctrl Pts',(-66.,-9.27819586845952,-2.83865035877574));
#44380=CARTESIAN_POINT('Ctrl Pts',(-66.,-9.15420774452698,-2.85088854357451));
#44381=CARTESIAN_POINT('Ctrl Pts',(-66.,-9.02829876834023,-2.86330140690357));
#44382=CARTESIAN_POINT('Ctrl Pts',(-66.,-8.90175450092416,-2.87339734928437));
#44383=CARTESIAN_POINT('Ctrl Pts',(-66.,-8.77626669445802,-2.87795483868359));
#44384=CARTESIAN_POINT('Ctrl Pts',(-66.,-8.65311618598693,-2.87453708498607));
#44385=CARTESIAN_POINT('Ctrl Pts',(-66.,-8.53276608899787,-2.86226751485878));
#44386=CARTESIAN_POINT('Ctrl Pts',(-66.,-8.41516000003073,-2.84134508257382));
#44387=CARTESIAN_POINT('Ctrl Pts',(-66.,-8.29987167630279,-2.81282035340105));
#44388=CARTESIAN_POINT('Ctrl Pts',(-66.,-8.18632063702037,-2.77826902816129));
#44389=CARTESIAN_POINT('Ctrl Pts',(-66.,-8.07392933499764,-2.7395290651848));
#44390=CARTESIAN_POINT('Ctrl Pts',(-66.,-7.96215124506878,-2.69848954828302));
#44391=CARTESIAN_POINT('Ctrl Pts',(-66.,-7.85051366140938,-2.65688319455118));
#44392=CARTESIAN_POINT('Ctrl Pts',(-66.,-7.73865755918351,-2.61606608299436));
#44393=CARTESIAN_POINT('Ctrl Pts',(-66.,-7.62637250505703,-2.5768319374997));
#44394=CARTESIAN_POINT('Ctrl Pts',(-66.,-7.53611801591863,-2.54702550658787));
#44395=CARTESIAN_POINT('Ctrl Pts',(-66.,-7.46817250201609,-2.52561569812117));
#44396=CARTESIAN_POINT('Ctrl Pts',(-66.,-7.42276245013638,-2.5117620104632));
#44397=CARTESIAN_POINT('Ctrl Pts',(-66.,-7.40002916450246,-2.50494004209942));
#44398=CARTESIAN_POINT('Ctrl Pts',(-66.,-7.40002916450246,-2.50494004209942));
#44399=CARTESIAN_POINT('Ctrl Pts',(-50.,-7.40002916450246,-2.50494004209942));
#44400=CARTESIAN_POINT('Ctrl Pts',(-66.,-7.42276245013638,-2.5117620104632));
#44401=CARTESIAN_POINT('Ctrl Pts',(-50.,-7.42276245013638,-2.5117620104632));
#44402=CARTESIAN_POINT('Ctrl Pts',(-66.,-7.46817250201609,-2.52561569812117));
#44403=CARTESIAN_POINT('Ctrl Pts',(-50.,-7.46817250201609,-2.52561569812117));
#44404=CARTESIAN_POINT('Ctrl Pts',(-66.,-7.53611801591863,-2.54702550658787));
#44405=CARTESIAN_POINT('Ctrl Pts',(-50.,-7.53611801591863,-2.54702550658787));
#44406=CARTESIAN_POINT('Ctrl Pts',(-66.,-7.62637250505703,-2.5768319374997));
#44407=CARTESIAN_POINT('Ctrl Pts',(-50.,-7.62637250505703,-2.5768319374997));
#44408=CARTESIAN_POINT('Ctrl Pts',(-66.,-7.73865755918351,-2.61606608299436));
#44409=CARTESIAN_POINT('Ctrl Pts',(-50.,-7.73865755918351,-2.61606608299436));
#44410=CARTESIAN_POINT('Ctrl Pts',(-66.,-7.85051366140938,-2.65688319455118));
#44411=CARTESIAN_POINT('Ctrl Pts',(-50.,-7.85051366140938,-2.65688319455118));
#44412=CARTESIAN_POINT('Ctrl Pts',(-66.,-7.96215124506878,-2.69848954828302));
#44413=CARTESIAN_POINT('Ctrl Pts',(-50.,-7.96215124506878,-2.69848954828302));
#44414=CARTESIAN_POINT('Ctrl Pts',(-66.,-8.07392933499764,-2.7395290651848));
#44415=CARTESIAN_POINT('Ctrl Pts',(-50.,-8.07392933499764,-2.7395290651848));
#44416=CARTESIAN_POINT('Ctrl Pts',(-66.,-8.18632063702037,-2.77826902816129));
#44417=CARTESIAN_POINT('Ctrl Pts',(-50.,-8.18632063702037,-2.77826902816129));
#44418=CARTESIAN_POINT('Ctrl Pts',(-66.,-8.29987167630279,-2.81282035340105));
#44419=CARTESIAN_POINT('Ctrl Pts',(-50.,-8.29987167630279,-2.81282035340105));
#44420=CARTESIAN_POINT('Ctrl Pts',(-66.,-8.41516000003073,-2.84134508257382));
#44421=CARTESIAN_POINT('Ctrl Pts',(-50.,-8.41516000003073,-2.84134508257382));
#44422=CARTESIAN_POINT('Ctrl Pts',(-66.,-8.53276608899787,-2.86226751485878));
#44423=CARTESIAN_POINT('Ctrl Pts',(-50.,-8.53276608899787,-2.86226751485878));
#44424=CARTESIAN_POINT('Ctrl Pts',(-66.,-8.65311618598693,-2.87453708498607));
#44425=CARTESIAN_POINT('Ctrl Pts',(-50.,-8.65311618598693,-2.87453708498607));
#44426=CARTESIAN_POINT('Ctrl Pts',(-66.,-8.77626669445802,-2.87795483868359));
#44427=CARTESIAN_POINT('Ctrl Pts',(-50.,-8.77626669445802,-2.87795483868359));
#44428=CARTESIAN_POINT('Ctrl Pts',(-66.,-8.90175450092416,-2.87339734928437));
#44429=CARTESIAN_POINT('Ctrl Pts',(-50.,-8.90175450092416,-2.87339734928437));
#44430=CARTESIAN_POINT('Ctrl Pts',(-66.,-9.02829876834023,-2.86330140690357));
#44431=CARTESIAN_POINT('Ctrl Pts',(-50.,-9.02829876834023,-2.86330140690357));
#44432=CARTESIAN_POINT('Ctrl Pts',(-66.,-9.15420774452698,-2.85088854357451));
#44433=CARTESIAN_POINT('Ctrl Pts',(-50.,-9.15420774452698,-2.85088854357451));
#44434=CARTESIAN_POINT('Ctrl Pts',(-66.,-9.27819586845952,-2.83865035877574));
#44435=CARTESIAN_POINT('Ctrl Pts',(-50.,-9.27819586845952,-2.83865035877574));
#44436=CARTESIAN_POINT('Ctrl Pts',(-66.,-9.39994535205166,-2.82729907482675));
#44437=CARTESIAN_POINT('Ctrl Pts',(-50.,-9.39994535205166,-2.82729907482675));
#44438=CARTESIAN_POINT('Ctrl Pts',(-66.,-9.52107645394674,-2.813969949702));
#44439=CARTESIAN_POINT('Ctrl Pts',(-50.,-9.52107645394674,-2.813969949702));
#44440=CARTESIAN_POINT('Ctrl Pts',(-66.,-9.64481438918646,-2.7928151444673));
#44441=CARTESIAN_POINT('Ctrl Pts',(-50.,-9.64481438918646,-2.7928151444673));
#44442=CARTESIAN_POINT('Ctrl Pts',(-66.,-9.77414249640863,-2.75837486685676));
#44443=CARTESIAN_POINT('Ctrl Pts',(-50.,-9.77414249640863,-2.75837486685676));
#44444=CARTESIAN_POINT('Ctrl Pts',(-66.,-9.91043916452916,-2.70806263410035));
#44445=CARTESIAN_POINT('Ctrl Pts',(-50.,-9.91043916452916,-2.70806263410035));
#44446=CARTESIAN_POINT('Ctrl Pts',(-66.,-10.0517126006492,-2.64538396696739));
#44447=CARTESIAN_POINT('Ctrl Pts',(-50.,-10.0517126006492,-2.64538396696739));
#44448=CARTESIAN_POINT('Ctrl Pts',(-66.,-10.1915866617002,-2.58179003974993));
#44449=CARTESIAN_POINT('Ctrl Pts',(-50.,-10.1915866617002,-2.58179003974993));
#44450=CARTESIAN_POINT('Ctrl Pts',(-66.,-10.3211089325964,-2.53340662380053));
#44451=CARTESIAN_POINT('Ctrl Pts',(-50.,-10.3211089325964,-2.53340662380053));
#44452=CARTESIAN_POINT('Ctrl Pts',(-66.,-10.4301695484658,-2.51847030265793));
#44453=CARTESIAN_POINT('Ctrl Pts',(-50.,-10.4301695484658,-2.51847030265793));
#44454=CARTESIAN_POINT('Ctrl Pts',(-66.,-10.5090079672805,-2.55460462120467));
#44455=CARTESIAN_POINT('Ctrl Pts',(-50.,-10.5090079672805,-2.55460462120467));
#44456=CARTESIAN_POINT('Ctrl Pts',(-66.,-10.5498295182902,-2.65589926109984));
#44457=CARTESIAN_POINT('Ctrl Pts',(-50.,-10.5498295182902,-2.65589926109984));
#44458=CARTESIAN_POINT('Ctrl Pts',(-66.,-10.546721479946,-2.83305751623384));
#44459=CARTESIAN_POINT('Ctrl Pts',(-50.,-10.546721479946,-2.83305751623384));
#44460=CARTESIAN_POINT('Ctrl Pts',(-66.,-10.4953284844905,-3.09397849340119));
#44461=CARTESIAN_POINT('Ctrl Pts',(-50.,-10.4953284844905,-3.09397849340119));
#44462=CARTESIAN_POINT('Ctrl Pts',(-66.,-10.3926275720677,-3.44415975566763));
#44463=CARTESIAN_POINT('Ctrl Pts',(-50.,-10.3926275720677,-3.44415975566763));
#44464=CARTESIAN_POINT('Ctrl Pts',(-66.,-10.236674684175,-3.88715181574754));
#44465=CARTESIAN_POINT('Ctrl Pts',(-50.,-10.236674684175,-3.88715181574754));
#44466=CARTESIAN_POINT('Ctrl Pts',(-66.,-10.0263759985737,-4.4249680705051));
#44467=CARTESIAN_POINT('Ctrl Pts',(-50.,-10.0263759985737,-4.4249680705051));
#44468=CARTESIAN_POINT('Ctrl Pts',(-66.,-9.76126006590556,-5.0584935545573));
#44469=CARTESIAN_POINT('Ctrl Pts',(-50.,-9.76126006590556,-5.0584935545573));
#44470=CARTESIAN_POINT('Ctrl Pts',(-66.,-9.50525999722784,-5.64199937966045));
#44471=CARTESIAN_POINT('Ctrl Pts',(-50.,-9.50525999722784,-5.64199937966045));
#44472=CARTESIAN_POINT('Ctrl Pts',(-66.,-9.28861816866069,-6.12267093171814));
#44473=CARTESIAN_POINT('Ctrl Pts',(-50.,-9.28861816866069,-6.12267093171814));
#44474=CARTESIAN_POINT('Ctrl Pts',(-66.,-9.13325294103339,-6.46222306161301));
#44475=CARTESIAN_POINT('Ctrl Pts',(-50.,-9.13325294103339,-6.46222306161301));
#44476=CARTESIAN_POINT('Ctrl Pts',(-66.,-9.05283599096422,-6.63677523505979));
#44477=CARTESIAN_POINT('Ctrl Pts',(-50.,-9.05283599096422,-6.63677523505979));
#44478=CARTESIAN_POINT('',(-65.5,-10.3165280543869,-2.54162819921576));
#44479=CARTESIAN_POINT('Ctrl Pts',(-66.,-9.74002772607264,-2.76540863080598));
#44480=CARTESIAN_POINT('Ctrl Pts',(-65.7982417703062,-9.96874182322222,
-2.6985542896893));
#44481=CARTESIAN_POINT('Ctrl Pts',(-65.6331946192802,-10.1702101505182,
-2.5787303726559));
#44482=CARTESIAN_POINT('Ctrl Pts',(-65.5,-10.3165280543869,-2.54162819921576));
#44483=CARTESIAN_POINT('',(-50.,-7.40002916450246,-2.50494004209942));
#44484=CARTESIAN_POINT('',(-66.,-7.40002916450246,-2.50494004209942));
#44485=CARTESIAN_POINT('',(-50.,-9.74002772607266,-2.76540863080597));
#44486=CARTESIAN_POINT('Ctrl Pts',(-50.,-7.40002916450246,-2.50494004209942));
#44487=CARTESIAN_POINT('Ctrl Pts',(-50.,-7.42276245013638,-2.5117620104632));
#44488=CARTESIAN_POINT('Ctrl Pts',(-50.,-7.46817250201609,-2.52561569812117));
#44489=CARTESIAN_POINT('Ctrl Pts',(-50.,-7.53611801591863,-2.54702550658787));
#44490=CARTESIAN_POINT('Ctrl Pts',(-50.,-7.62637250505703,-2.5768319374997));
#44491=CARTESIAN_POINT('Ctrl Pts',(-50.,-7.73865755918351,-2.61606608299436));
#44492=CARTESIAN_POINT('Ctrl Pts',(-50.,-7.85051366140938,-2.65688319455118));
#44493=CARTESIAN_POINT('Ctrl Pts',(-50.,-7.96215124506878,-2.69848954828302));
#44494=CARTESIAN_POINT('Ctrl Pts',(-50.,-8.07392933499764,-2.7395290651848));
#44495=CARTESIAN_POINT('Ctrl Pts',(-50.,-8.18632063702037,-2.77826902816129));
#44496=CARTESIAN_POINT('Ctrl Pts',(-50.,-8.29987167630279,-2.81282035340105));
#44497=CARTESIAN_POINT('Ctrl Pts',(-50.,-8.41516000003073,-2.84134508257382));
#44498=CARTESIAN_POINT('Ctrl Pts',(-50.,-8.53276608899787,-2.86226751485878));
#44499=CARTESIAN_POINT('Ctrl Pts',(-50.,-8.65311618598693,-2.87453708498607));
#44500=CARTESIAN_POINT('Ctrl Pts',(-50.,-8.77626669445802,-2.87795483868359));
#44501=CARTESIAN_POINT('Ctrl Pts',(-50.,-8.90175450092416,-2.87339734928437));
#44502=CARTESIAN_POINT('Ctrl Pts',(-50.,-9.02829876834023,-2.86330140690357));
#44503=CARTESIAN_POINT('Ctrl Pts',(-50.,-9.15420774452698,-2.85088854357451));
#44504=CARTESIAN_POINT('Ctrl Pts',(-50.,-9.27819586845952,-2.83865035877574));
#44505=CARTESIAN_POINT('Ctrl Pts',(-50.,-9.39994535205166,-2.82729907482675));
#44506=CARTESIAN_POINT('Ctrl Pts',(-50.,-9.51449651805853,-2.8146939981701));
#44507=CARTESIAN_POINT('Ctrl Pts',(-50.,-9.60663333505539,-2.79931553203575));
#44508=CARTESIAN_POINT('Ctrl Pts',(-50.,-9.67603813743556,-2.78330078551466));
#44509=CARTESIAN_POINT('Ctrl Pts',(-50.,-9.72093701180547,-2.77098894762809));
#44510=CARTESIAN_POINT('Ctrl Pts',(-50.,-9.74002772607266,-2.76540863080597));
#44511=CARTESIAN_POINT('',(-50.5,-10.3165280543869,-2.54162819921576));
#44512=CARTESIAN_POINT('Ctrl Pts',(-50.5,-10.3165280543869,-2.54162819921576));
#44513=CARTESIAN_POINT('Ctrl Pts',(-50.4982567069806,-10.3146129996962,
-2.54211380411715));
#44514=CARTESIAN_POINT('Ctrl Pts',(-50.4965113438773,-10.3126926234528,
-2.54261184547092));
#44515=CARTESIAN_POINT('Ctrl Pts',(-50.3581212730791,-10.1601917353906,
-2.5830075707719));
#44516=CARTESIAN_POINT('Ctrl Pts',(-50.2022201285467,-9.969265433978,-2.69840123549405));
#44517=CARTESIAN_POINT('Ctrl Pts',(-50.,-9.74002772607266,-2.76540863080597));
#44518=CARTESIAN_POINT('Ctrl Pts',(-65.5,-10.3165280543869,-2.54162819921576));
#44519=CARTESIAN_POINT('Ctrl Pts',(-60.5,-10.3165280543869,-2.54162819921576));
#44520=CARTESIAN_POINT('Ctrl Pts',(-55.5,-10.3165280543869,-2.54162819921576));
#44521=CARTESIAN_POINT('Ctrl Pts',(-50.5,-10.3165280543869,-2.54162819921576));
#44522=CARTESIAN_POINT('Origin',(-66.,0.,0.));
#44523=CARTESIAN_POINT('',(-50.,-6.81311923233408,-3.82316133271923));
#44524=CARTESIAN_POINT('',(-66.,-6.81311923233408,-3.82316133271923));
#44525=CARTESIAN_POINT('Origin',(-50.,0.,0.));
#44526=CARTESIAN_POINT('Ctrl Pts',(-66.,-9.05283599096422,-6.63677523505979));
#44527=CARTESIAN_POINT('Ctrl Pts',(-50.,-9.05283599096422,-6.63677523505979));
#44528=CARTESIAN_POINT('Ctrl Pts',(-66.,-9.04650986963351,-6.61394569161654));
#44529=CARTESIAN_POINT('Ctrl Pts',(-50.,-9.04650986963351,-6.61394569161654));
#44530=CARTESIAN_POINT('Ctrl Pts',(-66.,-9.03368618446229,-6.56841384495789));
#44531=CARTESIAN_POINT('Ctrl Pts',(-50.,-9.03368618446229,-6.56841384495789));
#44532=CARTESIAN_POINT('Ctrl Pts',(-66.,-9.01393632934211,-6.50049779584927));
#44533=CARTESIAN_POINT('Ctrl Pts',(-50.,-9.01393632934211,-6.50049779584927));
#44534=CARTESIAN_POINT('Ctrl Pts',(-66.,-8.98657316507665,-6.41070751897976));
#44535=CARTESIAN_POINT('Ctrl Pts',(-50.,-8.98657316507665,-6.41070751897976));
#44536=CARTESIAN_POINT('Ctrl Pts',(-66.,-8.95064359737786,-6.29975301753961));
#44537=CARTESIAN_POINT('Ctrl Pts',(-50.,-8.95064359737786,-6.29975301753961));
#44538=CARTESIAN_POINT('Ctrl Pts',(-66.,-8.91297549834918,-6.19009933699878));
#44539=CARTESIAN_POINT('Ctrl Pts',(-50.,-8.91297549834918,-6.19009933699878));
#44540=CARTESIAN_POINT('Ctrl Pts',(-66.,-8.87355356113552,-6.08177373585213));
#44541=CARTESIAN_POINT('Ctrl Pts',(-50.,-8.87355356113552,-6.08177373585213));
#44542=CARTESIAN_POINT('Ctrl Pts',(-66.,-8.8323617893429,-5.97481445690694));
#44543=CARTESIAN_POINT('Ctrl Pts',(-50.,-8.8323617893429,-5.97481445690694));
#44544=CARTESIAN_POINT('Ctrl Pts',(-66.,-8.78938549860367,-5.86927258716782));
#44545=CARTESIAN_POINT('Ctrl Pts',(-50.,-8.78938549860367,-5.86927258716782));
#44546=CARTESIAN_POINT('Ctrl Pts',(-66.,-8.74461231231568,-5.76520918432743));
#44547=CARTESIAN_POINT('Ctrl Pts',(-50.,-8.74461231231568,-5.76520918432743));
#44548=CARTESIAN_POINT('Ctrl Pts',(-66.,-8.69803287743194,-5.66269130953282));
#44549=CARTESIAN_POINT('Ctrl Pts',(-50.,-8.69803287743194,-5.66269130953282));
#44550=CARTESIAN_POINT('Ctrl Pts',(-66.,-8.64964214626068,-5.56178799460163));
#44551=CARTESIAN_POINT('Ctrl Pts',(-50.,-8.64964214626068,-5.56178799460163));
#44552=CARTESIAN_POINT('Ctrl Pts',(-66.,-8.59944008163277,-5.46256677385502));
#44553=CARTESIAN_POINT('Ctrl Pts',(-50.,-8.59944008163277,-5.46256677385502));
#44554=CARTESIAN_POINT('Ctrl Pts',(-66.,-8.54743429835474,-5.36508801729631));
#44555=CARTESIAN_POINT('Ctrl Pts',(-50.,-8.54743429835474,-5.36508801729631));
#44556=CARTESIAN_POINT('Ctrl Pts',(-66.,-8.49363486229967,-5.26940895206487));
#44557=CARTESIAN_POINT('Ctrl Pts',(-50.,-8.49363486229967,-5.26940895206487));
#44558=CARTESIAN_POINT('Ctrl Pts',(-66.,-8.43804526716559,-5.17559278329922));
#44559=CARTESIAN_POINT('Ctrl Pts',(-50.,-8.43804526716559,-5.17559278329922));
#44560=CARTESIAN_POINT('Ctrl Pts',(-66.,-8.38065449559913,-5.08371585603889));
#44561=CARTESIAN_POINT('Ctrl Pts',(-50.,-8.38065449559913,-5.08371585603889));
#44562=CARTESIAN_POINT('Ctrl Pts',(-66.,-8.32142939657439,-4.99387589925328));
#44563=CARTESIAN_POINT('Ctrl Pts',(-50.,-8.32142939657439,-4.99387589925328));
#44564=CARTESIAN_POINT('Ctrl Pts',(-66.,-8.26030546894961,-4.90619864910471));
#44565=CARTESIAN_POINT('Ctrl Pts',(-50.,-8.26030546894961,-4.90619864910471));
#44566=CARTESIAN_POINT('Ctrl Pts',(-66.,-8.19718568217584,-4.82084919686819));
#44567=CARTESIAN_POINT('Ctrl Pts',(-50.,-8.19718568217584,-4.82084919686819));
#44568=CARTESIAN_POINT('Ctrl Pts',(-66.,-8.13194562956026,-4.73804414042434));
#44569=CARTESIAN_POINT('Ctrl Pts',(-50.,-8.13194562956026,-4.73804414042434));
#44570=CARTESIAN_POINT('Ctrl Pts',(-66.,-8.06443555863034,-4.65806703431538));
#44571=CARTESIAN_POINT('Ctrl Pts',(-50.,-8.06443555863034,-4.65806703431538));
#44572=CARTESIAN_POINT('Ctrl Pts',(-66.,-7.9944866564592,-4.58127474760048));
#44573=CARTESIAN_POINT('Ctrl Pts',(-50.,-7.9944866564592,-4.58127474760048));
#44574=CARTESIAN_POINT('Ctrl Pts',(-66.,-7.92190852612585,-4.50812719257416));
#44575=CARTESIAN_POINT('Ctrl Pts',(-50.,-7.92190852612585,-4.50812719257416));
#44576=CARTESIAN_POINT('Ctrl Pts',(-66.,-7.84652367297445,-4.43911683844659));
#44577=CARTESIAN_POINT('Ctrl Pts',(-50.,-7.84652367297445,-4.43911683844659));
#44578=CARTESIAN_POINT('Ctrl Pts',(-66.,-7.76822240772673,-4.37464133248276));
#44579=CARTESIAN_POINT('Ctrl Pts',(-50.,-7.76822240772673,-4.37464133248276));
#44580=CARTESIAN_POINT('Ctrl Pts',(-66.,-7.68701560500139,-4.31488559005748));
#44581=CARTESIAN_POINT('Ctrl Pts',(-50.,-7.68701560500139,-4.31488559005748));
#44582=CARTESIAN_POINT('Ctrl Pts',(-66.,-7.60308160854854,-4.25971402139557));
#44583=CARTESIAN_POINT('Ctrl Pts',(-50.,-7.60308160854854,-4.25971402139557));
#44584=CARTESIAN_POINT('Ctrl Pts',(-66.,-7.51683638885138,-4.2085165697132));
#44585=CARTESIAN_POINT('Ctrl Pts',(-50.,-7.51683638885138,-4.2085165697132));
#44586=CARTESIAN_POINT('Ctrl Pts',(-66.,-7.42887813111136,-4.16030958503735));
#44587=CARTESIAN_POINT('Ctrl Pts',(-50.,-7.42887813111136,-4.16030958503735));
#44588=CARTESIAN_POINT('Ctrl Pts',(-66.,-7.33988712400327,-4.11392789982873));
#44589=CARTESIAN_POINT('Ctrl Pts',(-50.,-7.33988712400327,-4.11392789982873));
#44590=CARTESIAN_POINT('Ctrl Pts',(-66.,-7.25053915877239,-4.06818897832557));
#44591=CARTESIAN_POINT('Ctrl Pts',(-50.,-7.25053915877239,-4.06818897832557));
#44592=CARTESIAN_POINT('Ctrl Pts',(-66.,-7.16141787020827,-4.02206007310117));
#44593=CARTESIAN_POINT('Ctrl Pts',(-50.,-7.16141787020827,-4.02206007310117));
#44594=CARTESIAN_POINT('Ctrl Pts',(-66.,-7.0729158360807,-3.97484570454348));
#44595=CARTESIAN_POINT('Ctrl Pts',(-50.,-7.0729158360807,-3.97484570454348));
#44596=CARTESIAN_POINT('Ctrl Pts',(-66.,-6.98526217067656,-3.92614017091869));
#44597=CARTESIAN_POINT('Ctrl Pts',(-50.,-6.98526217067656,-3.92614017091869));
#44598=CARTESIAN_POINT('Ctrl Pts',(-66.,-6.91590770916956,-3.88582374481706));
#44599=CARTESIAN_POINT('Ctrl Pts',(-50.,-6.91590770916956,-3.88582374481706));
#44600=CARTESIAN_POINT('Ctrl Pts',(-66.,-6.86433957558852,-3.8547985554459));
#44601=CARTESIAN_POINT('Ctrl Pts',(-50.,-6.86433957558852,-3.8547985554459));
#44602=CARTESIAN_POINT('Ctrl Pts',(-66.,-6.8301595578254,-3.83376536134756));
#44603=CARTESIAN_POINT('Ctrl Pts',(-50.,-6.8301595578254,-3.83376536134756));
#44604=CARTESIAN_POINT('Ctrl Pts',(-66.,-6.81311923233407,-3.82316133271924));
#44605=CARTESIAN_POINT('Ctrl Pts',(-50.,-6.81311923233407,-3.82316133271924));
#44606=CARTESIAN_POINT('Ctrl Pts',(-50.,-8.56527454818065,-5.39923114103194));
#44607=CARTESIAN_POINT('Ctrl Pts',(-50.,-8.56163853106842,-5.39247090060412));
#44608=CARTESIAN_POINT('Ctrl Pts',(-50.,-8.54750490102424,-5.3663130759002));
#44609=CARTESIAN_POINT('Ctrl Pts',(-50.,-8.52260030822016,-5.32102960234266));
#44610=CARTESIAN_POINT('Ctrl Pts',(-50.,-8.48638332772613,-5.25717084905799));
#44611=CARTESIAN_POINT('Ctrl Pts',(-50.,-8.43804526716559,-5.17559278329922));
#44612=CARTESIAN_POINT('Ctrl Pts',(-50.,-8.38065449559913,-5.08371585603889));
#44613=CARTESIAN_POINT('Ctrl Pts',(-50.,-8.32142939657439,-4.99387589925328));
#44614=CARTESIAN_POINT('Ctrl Pts',(-50.,-8.26030546894961,-4.90619864910471));
#44615=CARTESIAN_POINT('Ctrl Pts',(-50.,-8.19718568217584,-4.82084919686819));
#44616=CARTESIAN_POINT('Ctrl Pts',(-50.,-8.13194562956026,-4.73804414042434));
#44617=CARTESIAN_POINT('Ctrl Pts',(-50.,-8.06443555863034,-4.65806703431538));
#44618=CARTESIAN_POINT('Ctrl Pts',(-50.,-7.9944866564592,-4.58127474760048));
#44619=CARTESIAN_POINT('Ctrl Pts',(-50.,-7.92190852612585,-4.50812719257416));
#44620=CARTESIAN_POINT('Ctrl Pts',(-50.,-7.84652367297445,-4.43911683844659));
#44621=CARTESIAN_POINT('Ctrl Pts',(-50.,-7.76822240772673,-4.37464133248276));
#44622=CARTESIAN_POINT('Ctrl Pts',(-50.,-7.68701560500139,-4.31488559005748));
#44623=CARTESIAN_POINT('Ctrl Pts',(-50.,-7.60308160854854,-4.25971402139557));
#44624=CARTESIAN_POINT('Ctrl Pts',(-50.,-7.51683638885138,-4.2085165697132));
#44625=CARTESIAN_POINT('Ctrl Pts',(-50.,-7.42887813111136,-4.16030958503735));
#44626=CARTESIAN_POINT('Ctrl Pts',(-50.,-7.33988712400327,-4.11392789982873));
#44627=CARTESIAN_POINT('Ctrl Pts',(-50.,-7.25053915877239,-4.06818897832557));
#44628=CARTESIAN_POINT('Ctrl Pts',(-50.,-7.16141787020827,-4.02206007310117));
#44629=CARTESIAN_POINT('Ctrl Pts',(-50.,-7.0729158360807,-3.97484570454348));
#44630=CARTESIAN_POINT('Ctrl Pts',(-50.,-6.98526217067656,-3.92614017091869));
#44631=CARTESIAN_POINT('Ctrl Pts',(-50.,-6.91590770916956,-3.88582374481706));
#44632=CARTESIAN_POINT('Ctrl Pts',(-50.,-6.86433957558852,-3.8547985554459));
#44633=CARTESIAN_POINT('Ctrl Pts',(-50.,-6.8301595578254,-3.83376536134756));
#44634=CARTESIAN_POINT('Ctrl Pts',(-50.,-6.81311923233407,-3.82316133271924));
#44635=CARTESIAN_POINT('Origin',(-50.,-8.4736440577621,-4.30813108036277));
#44636=CARTESIAN_POINT('Origin',(-50.,0.,0.));
#44637=CARTESIAN_POINT('Origin',(-65.75,0.,0.));
#44638=CARTESIAN_POINT('',(-65.5,-10.4655009137276,-1.83409804120896));
#44639=CARTESIAN_POINT('Origin',(-65.5,0.,0.));
#44640=CARTESIAN_POINT('',(-66.,-10.0208328064459,-1.44863206690261));
#44641=CARTESIAN_POINT('Ctrl Pts',(-65.5,-10.4655009137276,-1.83409804120895));
#44642=CARTESIAN_POINT('Ctrl Pts',(-65.6641206711811,-10.3229569256148,
-1.69670740679554));
#44643=CARTESIAN_POINT('Ctrl Pts',(-65.8307448212024,-10.1746455742797,
-1.56762477685534));
#44644=CARTESIAN_POINT('Ctrl Pts',(-66.,-10.0208328064459,-1.44863206690261));
#44645=CARTESIAN_POINT('Origin',(-66.,0.,0.));
#44646=CARTESIAN_POINT('Origin',(-58.,0.,0.));
#44647=CARTESIAN_POINT('',(-50.5,-10.4655009137276,-1.83409804120895));
#44648=CARTESIAN_POINT('Origin',(-50.5,0.,0.));
#44649=CARTESIAN_POINT('Ctrl Pts',(-50.5,-10.4655009137276,-1.83409804120896));
#44650=CARTESIAN_POINT('Ctrl Pts',(-55.5,-10.4655009137276,-1.83409804120896));
#44651=CARTESIAN_POINT('Ctrl Pts',(-60.5,-10.4655009137276,-1.83409804120895));
#44652=CARTESIAN_POINT('Ctrl Pts',(-65.5,-10.4655009137276,-1.83409804120895));
#44653=CARTESIAN_POINT('Origin',(-50.25,0.,0.));
#44654=CARTESIAN_POINT('',(-50.,-10.0208328064459,-1.44863206690262));
#44655=CARTESIAN_POINT('Origin',(-50.,0.,0.));
#44656=CARTESIAN_POINT('Ctrl Pts',(-50.,-10.0208328064459,-1.44863206690262));
#44657=CARTESIAN_POINT('Ctrl Pts',(-50.1692551787974,-10.1746455742796,
-1.56762477685526));
#44658=CARTESIAN_POINT('Ctrl Pts',(-50.3358793288183,-10.3229569256143,
-1.69670740679502));
#44659=CARTESIAN_POINT('Ctrl Pts',(-50.5,-10.4655009137276,-1.83409804120896));
#44660=CARTESIAN_POINT('Origin',(-66.,-9.49333381220606,-0.489132040720954));
#44661=CARTESIAN_POINT('',(-66.,-10.0227511096935,1.43529968756956));
#44662=CARTESIAN_POINT('',(-66.,-10.125,-1.23995488413669E-15));
#44663=CARTESIAN_POINT('Origin',(-66.,0.,0.));
#44664=CARTESIAN_POINT('Origin',(-66.,0.,0.));
#44665=CARTESIAN_POINT('',(-66.,-7.77911393348366,-0.72148642390575));
#44666=CARTESIAN_POINT('Ctrl Pts',(-66.,-7.77911393348366,-0.721486423905757));
#44667=CARTESIAN_POINT('Ctrl Pts',(-66.,-7.79899409244038,-0.724242761304609));
#44668=CARTESIAN_POINT('Ctrl Pts',(-66.,-7.83877406317074,-0.72955527454762));
#44669=CARTESIAN_POINT('Ctrl Pts',(-66.,-7.89850297873842,-0.736923545827707));
#44670=CARTESIAN_POINT('Ctrl Pts',(-66.,-7.97825959982878,-0.745545432905555));
#44671=CARTESIAN_POINT('Ctrl Pts',(-66.,-8.07814553295023,-0.75438819429077));
#44672=CARTESIAN_POINT('Ctrl Pts',(-66.,-8.17819997799169,-0.761523645955682));
#44673=CARTESIAN_POINT('Ctrl Pts',(-66.,-8.27837864239844,-0.767415604052299));
#44674=CARTESIAN_POINT('Ctrl Pts',(-66.,-8.37860576557482,-0.772859096585322));
#44675=CARTESIAN_POINT('Ctrl Pts',(-66.,-8.4787682268314,-0.77903497093039));
#44676=CARTESIAN_POINT('Ctrl Pts',(-66.,-8.57872964077182,-0.787298396323681));
#44677=CARTESIAN_POINT('Ctrl Pts',(-66.,-8.67834244910087,-0.798990504610031));
#44678=CARTESIAN_POINT('Ctrl Pts',(-66.,-8.77746026893294,-0.81525320859497));
#44679=CARTESIAN_POINT('Ctrl Pts',(-66.,-8.8759512247709,-0.836813013320223));
#44680=CARTESIAN_POINT('Ctrl Pts',(-66.,-8.97370754082197,-0.86386632514724));
#44681=CARTESIAN_POINT('Ctrl Pts',(-66.,-9.07064407076881,-0.896248638581227));
#44682=CARTESIAN_POINT('Ctrl Pts',(-66.,-9.16669928303964,-0.933552070120681));
#44683=CARTESIAN_POINT('Ctrl Pts',(-66.,-9.2618350217977,-0.975254533175137));
#44684=CARTESIAN_POINT('Ctrl Pts',(-66.,-9.35603816010254,-1.02085843555253));
#44685=CARTESIAN_POINT('Ctrl Pts',(-66.,-9.44931776451354,-1.0699690987417));
#44686=CARTESIAN_POINT('Ctrl Pts',(-66.,-9.54169530869912,-1.12226657296063));
#44687=CARTESIAN_POINT('Ctrl Pts',(-66.,-9.63319634553357,-1.17750238543874));
#44688=CARTESIAN_POINT('Ctrl Pts',(-66.,-9.7238423681631,-1.23548625191189));
#44689=CARTESIAN_POINT('Ctrl Pts',(-66.,-9.81364115980824,-1.29607707170225));
#44690=CARTESIAN_POINT('Ctrl Pts',(-66.,-9.8909809640799,-1.35094148263425));
#44691=CARTESIAN_POINT('Ctrl Pts',(-66.,-9.95004051704176,-1.3945485835597));
#44692=CARTESIAN_POINT('Ctrl Pts',(-66.,-9.99121044269398,-1.42578748466016));
#44693=CARTESIAN_POINT('Ctrl Pts',(-66.,-10.0147615020311,-1.44393518136159));
#44694=CARTESIAN_POINT('Ctrl Pts',(-66.,-10.0208328064459,-1.44863206690261));
#44695=CARTESIAN_POINT('',(-66.,-7.77911393348366,0.721486423905763));
#44696=CARTESIAN_POINT('Origin',(-66.,0.,0.));
#44697=CARTESIAN_POINT('Ctrl Pts',(-66.,-10.0227511096935,1.43529968756956));
#44698=CARTESIAN_POINT('Ctrl Pts',(-66.,-10.0075805937231,1.42243692144955));
#44699=CARTESIAN_POINT('Ctrl Pts',(-66.,-9.97157110660129,1.39292748043395));
#44700=CARTESIAN_POINT('Ctrl Pts',(-66.,-9.91468044888801,1.35006780516087));
#44701=CARTESIAN_POINT('Ctrl Pts',(-66.,-9.83676426393002,1.29854345762933));
#44702=CARTESIAN_POINT('Ctrl Pts',(-66.,-9.73724351312182,1.24043599038436));
#44703=CARTESIAN_POINT('Ctrl Pts',(-66.,-9.6306368085439,1.18054610024187));
#44704=CARTESIAN_POINT('Ctrl Pts',(-66.,-9.5223457393261,1.11893544879958));
#44705=CARTESIAN_POINT('Ctrl Pts',(-66.,-9.41237093241568,1.05638393958167));
#44706=CARTESIAN_POINT('Ctrl Pts',(-66.,-9.30087338143967,0.995690646749764));
#44707=CARTESIAN_POINT('Ctrl Pts',(-66.,-9.18808826379209,0.940486683861864));
#44708=CARTESIAN_POINT('Ctrl Pts',(-66.,-9.07419455050615,0.893519132818963));
#44709=CARTESIAN_POINT('Ctrl Pts',(-66.,-8.9592587823094,0.855777148432806));
#44710=CARTESIAN_POINT('Ctrl Pts',(-66.,-8.84331035406979,0.8270560355778));
#44711=CARTESIAN_POINT('Ctrl Pts',(-66.,-8.72638717702053,0.80622268656513));
#44712=CARTESIAN_POINT('Ctrl Pts',(-66.,-8.60859985083163,0.791601524257944));
#44713=CARTESIAN_POINT('Ctrl Pts',(-66.,-8.49016832489629,0.781278580568713));
#44714=CARTESIAN_POINT('Ctrl Pts',(-66.,-8.37136168323973,0.773305799751092));
#44715=CARTESIAN_POINT('Ctrl Pts',(-66.,-8.25245284713798,0.765907999193168));
#44716=CARTESIAN_POINT('Ctrl Pts',(-66.,-8.13366539810525,0.757700310523095));
#44717=CARTESIAN_POINT('Ctrl Pts',(-66.,-8.01512993231441,0.747872039941245));
#44718=CARTESIAN_POINT('Ctrl Pts',(-66.,-7.92055498607902,0.738391761574612));
#44719=CARTESIAN_POINT('Ctrl Pts',(-66.,-7.84977551686152,0.730314664611583));
#44720=CARTESIAN_POINT('Ctrl Pts',(-66.,-7.80265656782328,0.724500705979671));
#44721=CARTESIAN_POINT('Ctrl Pts',(-66.,-7.77911393348366,0.721486423905763));
#44722=CARTESIAN_POINT('Ctrl Pts',(-66.,-7.77911393348366,0.721486423905763));
#44723=CARTESIAN_POINT('Ctrl Pts',(-50.,-7.77911393348366,0.721486423905763));
#44724=CARTESIAN_POINT('Ctrl Pts',(-66.,-7.80265656782328,0.724500705979671));
#44725=CARTESIAN_POINT('Ctrl Pts',(-50.,-7.80265656782328,0.724500705979671));
#44726=CARTESIAN_POINT('Ctrl Pts',(-66.,-7.84977551686152,0.730314664611583));
#44727=CARTESIAN_POINT('Ctrl Pts',(-50.,-7.84977551686152,0.730314664611583));
#44728=CARTESIAN_POINT('Ctrl Pts',(-66.,-7.92055498607902,0.738391761574612));
#44729=CARTESIAN_POINT('Ctrl Pts',(-50.,-7.92055498607902,0.738391761574612));
#44730=CARTESIAN_POINT('Ctrl Pts',(-66.,-8.01512993231441,0.747872039941245));
#44731=CARTESIAN_POINT('Ctrl Pts',(-50.,-8.01512993231441,0.747872039941245));
#44732=CARTESIAN_POINT('Ctrl Pts',(-66.,-8.13366539810525,0.757700310523095));
#44733=CARTESIAN_POINT('Ctrl Pts',(-50.,-8.13366539810525,0.757700310523095));
#44734=CARTESIAN_POINT('Ctrl Pts',(-66.,-8.25245284713798,0.765907999193168));
#44735=CARTESIAN_POINT('Ctrl Pts',(-50.,-8.25245284713798,0.765907999193168));
#44736=CARTESIAN_POINT('Ctrl Pts',(-66.,-8.37136168323973,0.773305799751092));
#44737=CARTESIAN_POINT('Ctrl Pts',(-50.,-8.37136168323973,0.773305799751092));
#44738=CARTESIAN_POINT('Ctrl Pts',(-66.,-8.49016832489629,0.781278580568713));
#44739=CARTESIAN_POINT('Ctrl Pts',(-50.,-8.49016832489629,0.781278580568713));
#44740=CARTESIAN_POINT('Ctrl Pts',(-66.,-8.60859985083163,0.791601524257944));
#44741=CARTESIAN_POINT('Ctrl Pts',(-50.,-8.60859985083163,0.791601524257944));
#44742=CARTESIAN_POINT('Ctrl Pts',(-66.,-8.72638717702053,0.80622268656513));
#44743=CARTESIAN_POINT('Ctrl Pts',(-50.,-8.72638717702053,0.80622268656513));
#44744=CARTESIAN_POINT('Ctrl Pts',(-66.,-8.84331035406979,0.8270560355778));
#44745=CARTESIAN_POINT('Ctrl Pts',(-50.,-8.84331035406979,0.8270560355778));
#44746=CARTESIAN_POINT('Ctrl Pts',(-66.,-8.9592587823094,0.855777148432806));
#44747=CARTESIAN_POINT('Ctrl Pts',(-50.,-8.9592587823094,0.855777148432806));
#44748=CARTESIAN_POINT('Ctrl Pts',(-66.,-9.07419455050615,0.893519132818963));
#44749=CARTESIAN_POINT('Ctrl Pts',(-50.,-9.07419455050615,0.893519132818963));
#44750=CARTESIAN_POINT('Ctrl Pts',(-66.,-9.18808826379209,0.940486683861864));
#44751=CARTESIAN_POINT('Ctrl Pts',(-50.,-9.18808826379209,0.940486683861864));
#44752=CARTESIAN_POINT('Ctrl Pts',(-66.,-9.30087338143967,0.995690646749764));
#44753=CARTESIAN_POINT('Ctrl Pts',(-50.,-9.30087338143967,0.995690646749764));
#44754=CARTESIAN_POINT('Ctrl Pts',(-66.,-9.41237093241568,1.05638393958167));
#44755=CARTESIAN_POINT('Ctrl Pts',(-50.,-9.41237093241568,1.05638393958167));
#44756=CARTESIAN_POINT('Ctrl Pts',(-66.,-9.5223457393261,1.11893544879958));
#44757=CARTESIAN_POINT('Ctrl Pts',(-50.,-9.5223457393261,1.11893544879958));
#44758=CARTESIAN_POINT('Ctrl Pts',(-66.,-9.6306368085439,1.18054610024187));
#44759=CARTESIAN_POINT('Ctrl Pts',(-50.,-9.6306368085439,1.18054610024187));
#44760=CARTESIAN_POINT('Ctrl Pts',(-66.,-9.73724351312182,1.24043599038436));
#44761=CARTESIAN_POINT('Ctrl Pts',(-50.,-9.73724351312182,1.24043599038436));
#44762=CARTESIAN_POINT('Ctrl Pts',(-66.,-9.84248083742894,1.30188120985331));
#44763=CARTESIAN_POINT('Ctrl Pts',(-50.,-9.84248083742894,1.30188120985331));
#44764=CARTESIAN_POINT('Ctrl Pts',(-66.,-9.94691663163917,1.37153583848331));
#44765=CARTESIAN_POINT('Ctrl Pts',(-50.,-9.94691663163917,1.37153583848331));
#44766=CARTESIAN_POINT('Ctrl Pts',(-66.,-10.0510556136356,1.45560107784126));
#44767=CARTESIAN_POINT('Ctrl Pts',(-50.,-10.0510556136356,1.45560107784126));
#44768=CARTESIAN_POINT('Ctrl Pts',(-66.,-10.1551049870319,1.5570004387935));
#44769=CARTESIAN_POINT('Ctrl Pts',(-50.,-10.1551049870319,1.5570004387935));
#44770=CARTESIAN_POINT('Ctrl Pts',(-66.,-10.2586709822228,1.67172133360717));
#44771=CARTESIAN_POINT('Ctrl Pts',(-50.,-10.2586709822228,1.67172133360717));
#44772=CARTESIAN_POINT('Ctrl Pts',(-66.,-10.3605863148615,1.78670918299558));
#44773=CARTESIAN_POINT('Ctrl Pts',(-50.,-10.3605863148615,1.78670918299558));
#44774=CARTESIAN_POINT('Ctrl Pts',(-66.,-10.4592314889185,1.88359108652926));
#44775=CARTESIAN_POINT('Ctrl Pts',(-50.,-10.4592314889185,1.88359108652926));
#44776=CARTESIAN_POINT('Ctrl Pts',(-66.,-10.5527881700323,1.94159504365348));
#44777=CARTESIAN_POINT('Ctrl Pts',(-50.,-10.5527881700323,1.94159504365348));
#44778=CARTESIAN_POINT('Ctrl Pts',(-66.,-10.6395078008537,1.94065117489419));
#44779=CARTESIAN_POINT('Ctrl Pts',(-50.,-10.6395078008537,1.94065117489419));
#44780=CARTESIAN_POINT('Ctrl Pts',(-66.,-10.7180003851451,1.86471753735723));
#44781=CARTESIAN_POINT('Ctrl Pts',(-50.,-10.7180003851451,1.86471753735723));
#44782=CARTESIAN_POINT('Ctrl Pts',(-66.,-10.78721780482,1.70161126501303));
#44783=CARTESIAN_POINT('Ctrl Pts',(-50.,-10.78721780482,1.70161126501303));
#44784=CARTESIAN_POINT('Ctrl Pts',(-66.,-10.8463940896281,1.44234467706895));
#44785=CARTESIAN_POINT('Ctrl Pts',(-50.,-10.8463940896281,1.44234467706895));
#44786=CARTESIAN_POINT('Ctrl Pts',(-66.,-10.8950036886707,1.08066595121422));
#44787=CARTESIAN_POINT('Ctrl Pts',(-50.,-10.8950036886707,1.08066595121422));
#44788=CARTESIAN_POINT('Ctrl Pts',(-66.,-10.9327147397562,0.612540812857));
#44789=CARTESIAN_POINT('Ctrl Pts',(-50.,-10.9327147397562,0.612540812857));
#44790=CARTESIAN_POINT('Ctrl Pts',(-66.,-10.9593469088286,0.0356850348521551));
#44791=CARTESIAN_POINT('Ctrl Pts',(-50.,-10.9593469088286,0.0356850348521551));
#44792=CARTESIAN_POINT('Ctrl Pts',(-66.,-10.9748294814774,-0.650901657883903));
#44793=CARTESIAN_POINT('Ctrl Pts',(-50.,-10.9748294814774,-0.650901657883903));
#44794=CARTESIAN_POINT('Ctrl Pts',(-66.,-10.9782949820983,-1.28808536247603));
#44795=CARTESIAN_POINT('Ctrl Pts',(-50.,-10.9782949820983,-1.28808536247603));
#44796=CARTESIAN_POINT('Ctrl Pts',(-66.,-10.9758895571813,-1.81531684557756));
#44797=CARTESIAN_POINT('Ctrl Pts',(-50.,-10.9758895571813,-1.81531684557756));
#44798=CARTESIAN_POINT('Ctrl Pts',(-66.,-10.9720646526695,-2.18870588261173));
#44799=CARTESIAN_POINT('Ctrl Pts',(-50.,-10.9720646526695,-2.18870588261173));
#44800=CARTESIAN_POINT('Ctrl Pts',(-66.,-10.9695968782856,-2.3808757481032));
#44801=CARTESIAN_POINT('Ctrl Pts',(-50.,-10.9695968782856,-2.3808757481032));
#44802=CARTESIAN_POINT('',(-65.5,-10.4583906644234,1.87421709262873));
#44803=CARTESIAN_POINT('Ctrl Pts',(-66.,-10.0227511096935,1.43529968756956));
#44804=CARTESIAN_POINT('Ctrl Pts',(-65.8225584213011,-10.1825947061167,
1.57082776061481));
#44805=CARTESIAN_POINT('Ctrl Pts',(-65.6845963763178,-10.2971553372475,
1.72560541037367));
#44806=CARTESIAN_POINT('Ctrl Pts',(-65.5373483115606,-10.4253681088298,
1.84668138012166));
#44807=CARTESIAN_POINT('Ctrl Pts',(-65.518392043377,-10.4420170465692,1.86131903035675));
#44808=CARTESIAN_POINT('Ctrl Pts',(-65.5,-10.4583906644234,1.87421709262873));
#44809=CARTESIAN_POINT('',(-50.,-7.77911393348366,0.721486423905763));
#44810=CARTESIAN_POINT('',(-66.,-7.77911393348366,0.721486423905763));
#44811=CARTESIAN_POINT('',(-50.,-10.0227511096935,1.43529968756957));
#44812=CARTESIAN_POINT('Ctrl Pts',(-50.,-7.77911393348366,0.721486423905763));
#44813=CARTESIAN_POINT('Ctrl Pts',(-50.,-7.80265656782328,0.724500705979671));
#44814=CARTESIAN_POINT('Ctrl Pts',(-50.,-7.84977551686152,0.730314664611583));
#44815=CARTESIAN_POINT('Ctrl Pts',(-50.,-7.92055498607902,0.738391761574612));
#44816=CARTESIAN_POINT('Ctrl Pts',(-50.,-8.01512993231441,0.747872039941245));
#44817=CARTESIAN_POINT('Ctrl Pts',(-50.,-8.13366539810525,0.757700310523095));
#44818=CARTESIAN_POINT('Ctrl Pts',(-50.,-8.25245284713798,0.765907999193168));
#44819=CARTESIAN_POINT('Ctrl Pts',(-50.,-8.37136168323973,0.773305799751092));
#44820=CARTESIAN_POINT('Ctrl Pts',(-50.,-8.49016832489629,0.781278580568713));
#44821=CARTESIAN_POINT('Ctrl Pts',(-50.,-8.60859985083163,0.791601524257944));
#44822=CARTESIAN_POINT('Ctrl Pts',(-50.,-8.72638717702053,0.80622268656513));
#44823=CARTESIAN_POINT('Ctrl Pts',(-50.,-8.84331035406979,0.8270560355778));
#44824=CARTESIAN_POINT('Ctrl Pts',(-50.,-8.9592587823094,0.855777148432806));
#44825=CARTESIAN_POINT('Ctrl Pts',(-50.,-9.07419455050615,0.893519132818963));
#44826=CARTESIAN_POINT('Ctrl Pts',(-50.,-9.18808826379209,0.940486683861864));
#44827=CARTESIAN_POINT('Ctrl Pts',(-50.,-9.30087338143967,0.995690646749764));
#44828=CARTESIAN_POINT('Ctrl Pts',(-50.,-9.41237093241568,1.05638393958167));
#44829=CARTESIAN_POINT('Ctrl Pts',(-50.,-9.5223457393261,1.11893544879958));
#44830=CARTESIAN_POINT('Ctrl Pts',(-50.,-9.6306368085439,1.18054610024187));
#44831=CARTESIAN_POINT('Ctrl Pts',(-50.,-9.73724351312182,1.24043599038436));
#44832=CARTESIAN_POINT('Ctrl Pts',(-50.,-9.83676426393003,1.29854345762933));
#44833=CARTESIAN_POINT('Ctrl Pts',(-50.,-9.91468044888801,1.35006780516087));
#44834=CARTESIAN_POINT('Ctrl Pts',(-50.,-9.9715711066013,1.39292748043396));
#44835=CARTESIAN_POINT('Ctrl Pts',(-50.,-10.0075805937231,1.42243692144956));
#44836=CARTESIAN_POINT('Ctrl Pts',(-50.,-10.0227511096935,1.43529968756957));
#44837=CARTESIAN_POINT('',(-50.5,-10.4583906644234,1.87421709262873));
#44838=CARTESIAN_POINT('Ctrl Pts',(-50.5,-10.4583906644234,1.87421709262874));
#44839=CARTESIAN_POINT('Ctrl Pts',(-50.4735369152344,-10.4348317575466,
1.85565893091618));
#44840=CARTESIAN_POINT('Ctrl Pts',(-50.4463054701399,-10.4110560430942,
1.83378829126636));
#44841=CARTESIAN_POINT('Ctrl Pts',(-50.2958361627283,-10.280846856736,1.70451692542734));
#44842=CARTESIAN_POINT('Ctrl Pts',(-50.1659505682738,-10.1722433304901,
1.5620510437276));
#44843=CARTESIAN_POINT('Ctrl Pts',(-50.,-10.0227511096935,1.43529968756958));
#44844=CARTESIAN_POINT('Ctrl Pts',(-65.5,-10.4583906644234,1.87421709262873));
#44845=CARTESIAN_POINT('Ctrl Pts',(-60.5,-10.4583906644234,1.87421709262873));
#44846=CARTESIAN_POINT('Ctrl Pts',(-55.5,-10.4583906644234,1.87421709262873));
#44847=CARTESIAN_POINT('Ctrl Pts',(-50.5,-10.4583906644234,1.87421709262873));
#44848=CARTESIAN_POINT('Origin',(-66.,0.,0.));
#44849=CARTESIAN_POINT('',(-50.,-7.77911393348366,-0.72148642390575));
#44850=CARTESIAN_POINT('',(-66.,-7.77911393348366,-0.72148642390575));
#44851=CARTESIAN_POINT('Origin',(-50.,0.,0.));
#44852=CARTESIAN_POINT('Ctrl Pts',(-66.,-10.9695968782856,-2.3808757481032));
#44853=CARTESIAN_POINT('Ctrl Pts',(-50.,-10.9695968782856,-2.3808757481032));
#44854=CARTESIAN_POINT('Ctrl Pts',(-66.,-10.9545320670164,-2.36259298774431));
#44855=CARTESIAN_POINT('Ctrl Pts',(-50.,-10.9545320670164,-2.36259298774431));
#44856=CARTESIAN_POINT('Ctrl Pts',(-66.,-10.924297577215,-2.32621343870963));
#44857=CARTESIAN_POINT('Ctrl Pts',(-50.,-10.924297577215,-2.32621343870963));
#44858=CARTESIAN_POINT('Ctrl Pts',(-66.,-10.8786312409555,-2.27220203031823));
#44859=CARTESIAN_POINT('Ctrl Pts',(-50.,-10.8786312409555,-2.27220203031823));
#44860=CARTESIAN_POINT('Ctrl Pts',(-66.,-10.8171127507393,-2.20130413232088));
#44861=CARTESIAN_POINT('Ctrl Pts',(-50.,-10.8171127507393,-2.20130413232088));
#44862=CARTESIAN_POINT('Ctrl Pts',(-66.,-10.7391601959231,-2.1145560232782));
#44863=CARTESIAN_POINT('Ctrl Pts',(-50.,-10.7391601959231,-2.1145560232782));
#44864=CARTESIAN_POINT('Ctrl Pts',(-66.,-10.6601485052333,-2.0297033976563));
#44865=CARTESIAN_POINT('Ctrl Pts',(-50.,-10.6601485052333,-2.0297033976563));
#44866=CARTESIAN_POINT('Ctrl Pts',(-66.,-10.5800747821907,-1.94677738318821));
#44867=CARTESIAN_POINT('Ctrl Pts',(-50.,-10.5800747821907,-1.94677738318821));
#44868=CARTESIAN_POINT('Ctrl Pts',(-66.,-10.4989399681134,-1.86581942273637));
#44869=CARTESIAN_POINT('Ctrl Pts',(-50.,-10.4989399681134,-1.86581942273637));
#44870=CARTESIAN_POINT('Ctrl Pts',(-66.,-10.4167514271206,-1.78688215927222));
#44871=CARTESIAN_POINT('Ctrl Pts',(-50.,-10.4167514271206,-1.78688215927222));
#44872=CARTESIAN_POINT('Ctrl Pts',(-66.,-10.3335226870247,-1.71002640579114));
#44873=CARTESIAN_POINT('Ctrl Pts',(-50.,-10.3335226870247,-1.71002640579114));
#44874=CARTESIAN_POINT('Ctrl Pts',(-66.,-10.2492724796178,-1.63531722992632));
#44875=CARTESIAN_POINT('Ctrl Pts',(-50.,-10.2492724796178,-1.63531722992632));
#44876=CARTESIAN_POINT('Ctrl Pts',(-66.,-10.164024271374,-1.56281974846243));
#44877=CARTESIAN_POINT('Ctrl Pts',(-50.,-10.164024271374,-1.56281974846243));
#44878=CARTESIAN_POINT('Ctrl Pts',(-66.,-10.0778054970205,-1.49259567218985));
#44879=CARTESIAN_POINT('Ctrl Pts',(-50.,-10.0778054970205,-1.49259567218985));
#44880=CARTESIAN_POINT('Ctrl Pts',(-66.,-9.99064766772184,-1.42469705463002));
#44881=CARTESIAN_POINT('Ctrl Pts',(-50.,-9.99064766772184,-1.42469705463002));
#44882=CARTESIAN_POINT('Ctrl Pts',(-66.,-9.90258325548514,-1.35917208121676));
#44883=CARTESIAN_POINT('Ctrl Pts',(-50.,-9.90258325548514,-1.35917208121676));
#44884=CARTESIAN_POINT('Ctrl Pts',(-66.,-9.81364115980824,-1.29607707170225));
#44885=CARTESIAN_POINT('Ctrl Pts',(-50.,-9.81364115980824,-1.29607707170225));
#44886=CARTESIAN_POINT('Ctrl Pts',(-66.,-9.7238423681631,-1.23548625191189));
#44887=CARTESIAN_POINT('Ctrl Pts',(-50.,-9.7238423681631,-1.23548625191189));
#44888=CARTESIAN_POINT('Ctrl Pts',(-66.,-9.63319634553357,-1.17750238543874));
#44889=CARTESIAN_POINT('Ctrl Pts',(-50.,-9.63319634553357,-1.17750238543874));
#44890=CARTESIAN_POINT('Ctrl Pts',(-66.,-9.54169530869912,-1.12226657296063));
#44891=CARTESIAN_POINT('Ctrl Pts',(-50.,-9.54169530869912,-1.12226657296063));
#44892=CARTESIAN_POINT('Ctrl Pts',(-66.,-9.44931776451354,-1.0699690987417));
#44893=CARTESIAN_POINT('Ctrl Pts',(-50.,-9.44931776451354,-1.0699690987417));
#44894=CARTESIAN_POINT('Ctrl Pts',(-66.,-9.35603816010254,-1.02085843555253));
#44895=CARTESIAN_POINT('Ctrl Pts',(-50.,-9.35603816010254,-1.02085843555253));
#44896=CARTESIAN_POINT('Ctrl Pts',(-66.,-9.2618350217977,-0.975254533175137));
#44897=CARTESIAN_POINT('Ctrl Pts',(-50.,-9.2618350217977,-0.975254533175137));
#44898=CARTESIAN_POINT('Ctrl Pts',(-66.,-9.16669928303964,-0.933552070120681));
#44899=CARTESIAN_POINT('Ctrl Pts',(-50.,-9.16669928303964,-0.933552070120681));
#44900=CARTESIAN_POINT('Ctrl Pts',(-66.,-9.07064407076881,-0.896248638581227));
#44901=CARTESIAN_POINT('Ctrl Pts',(-50.,-9.07064407076881,-0.896248638581227));
#44902=CARTESIAN_POINT('Ctrl Pts',(-66.,-8.97370754082197,-0.86386632514724));
#44903=CARTESIAN_POINT('Ctrl Pts',(-50.,-8.97370754082197,-0.86386632514724));
#44904=CARTESIAN_POINT('Ctrl Pts',(-66.,-8.8759512247709,-0.836813013320223));
#44905=CARTESIAN_POINT('Ctrl Pts',(-50.,-8.8759512247709,-0.836813013320223));
#44906=CARTESIAN_POINT('Ctrl Pts',(-66.,-8.77746026893294,-0.81525320859497));
#44907=CARTESIAN_POINT('Ctrl Pts',(-50.,-8.77746026893294,-0.81525320859497));
#44908=CARTESIAN_POINT('Ctrl Pts',(-66.,-8.67834244910087,-0.798990504610031));
#44909=CARTESIAN_POINT('Ctrl Pts',(-50.,-8.67834244910087,-0.798990504610031));
#44910=CARTESIAN_POINT('Ctrl Pts',(-66.,-8.57872964077182,-0.787298396323681));
#44911=CARTESIAN_POINT('Ctrl Pts',(-50.,-8.57872964077182,-0.787298396323681));
#44912=CARTESIAN_POINT('Ctrl Pts',(-66.,-8.4787682268314,-0.77903497093039));
#44913=CARTESIAN_POINT('Ctrl Pts',(-50.,-8.4787682268314,-0.77903497093039));
#44914=CARTESIAN_POINT('Ctrl Pts',(-66.,-8.37860576557482,-0.772859096585322));
#44915=CARTESIAN_POINT('Ctrl Pts',(-50.,-8.37860576557482,-0.772859096585322));
#44916=CARTESIAN_POINT('Ctrl Pts',(-66.,-8.27837864239844,-0.767415604052299));
#44917=CARTESIAN_POINT('Ctrl Pts',(-50.,-8.27837864239844,-0.767415604052299));
#44918=CARTESIAN_POINT('Ctrl Pts',(-66.,-8.17819997799169,-0.761523645955682));
#44919=CARTESIAN_POINT('Ctrl Pts',(-50.,-8.17819997799169,-0.761523645955682));
#44920=CARTESIAN_POINT('Ctrl Pts',(-66.,-8.07814553295023,-0.75438819429077));
#44921=CARTESIAN_POINT('Ctrl Pts',(-50.,-8.07814553295023,-0.75438819429077));
#44922=CARTESIAN_POINT('Ctrl Pts',(-66.,-7.97825959982878,-0.745545432905555));
#44923=CARTESIAN_POINT('Ctrl Pts',(-50.,-7.97825959982878,-0.745545432905555));
#44924=CARTESIAN_POINT('Ctrl Pts',(-66.,-7.89850297873842,-0.736923545827707));
#44925=CARTESIAN_POINT('Ctrl Pts',(-50.,-7.89850297873842,-0.736923545827707));
#44926=CARTESIAN_POINT('Ctrl Pts',(-66.,-7.83877406317074,-0.72955527454762));
#44927=CARTESIAN_POINT('Ctrl Pts',(-50.,-7.83877406317074,-0.72955527454762));
#44928=CARTESIAN_POINT('Ctrl Pts',(-66.,-7.79899409244038,-0.724242761304609));
#44929=CARTESIAN_POINT('Ctrl Pts',(-50.,-7.79899409244038,-0.724242761304609));
#44930=CARTESIAN_POINT('Ctrl Pts',(-66.,-7.77911393348366,-0.721486423905757));
#44931=CARTESIAN_POINT('Ctrl Pts',(-50.,-7.77911393348366,-0.721486423905757));
#44932=CARTESIAN_POINT('Ctrl Pts',(-50.,-10.0208328064459,-1.44863206690262));
#44933=CARTESIAN_POINT('Ctrl Pts',(-50.,-10.0147615020311,-1.4439351813616));
#44934=CARTESIAN_POINT('Ctrl Pts',(-50.,-9.99121044269398,-1.42578748466017));
#44935=CARTESIAN_POINT('Ctrl Pts',(-50.,-9.95004051704177,-1.39454858355971));
#44936=CARTESIAN_POINT('Ctrl Pts',(-50.,-9.8909809640799,-1.35094148263425));
#44937=CARTESIAN_POINT('Ctrl Pts',(-50.,-9.81364115980824,-1.29607707170225));
#44938=CARTESIAN_POINT('Ctrl Pts',(-50.,-9.7238423681631,-1.23548625191189));
#44939=CARTESIAN_POINT('Ctrl Pts',(-50.,-9.63319634553357,-1.17750238543874));
#44940=CARTESIAN_POINT('Ctrl Pts',(-50.,-9.54169530869912,-1.12226657296063));
#44941=CARTESIAN_POINT('Ctrl Pts',(-50.,-9.44931776451354,-1.0699690987417));
#44942=CARTESIAN_POINT('Ctrl Pts',(-50.,-9.35603816010254,-1.02085843555253));
#44943=CARTESIAN_POINT('Ctrl Pts',(-50.,-9.2618350217977,-0.975254533175137));
#44944=CARTESIAN_POINT('Ctrl Pts',(-50.,-9.16669928303964,-0.933552070120681));
#44945=CARTESIAN_POINT('Ctrl Pts',(-50.,-9.07064407076881,-0.896248638581227));
#44946=CARTESIAN_POINT('Ctrl Pts',(-50.,-8.97370754082197,-0.86386632514724));
#44947=CARTESIAN_POINT('Ctrl Pts',(-50.,-8.8759512247709,-0.836813013320223));
#44948=CARTESIAN_POINT('Ctrl Pts',(-50.,-8.77746026893294,-0.81525320859497));
#44949=CARTESIAN_POINT('Ctrl Pts',(-50.,-8.67834244910087,-0.798990504610031));
#44950=CARTESIAN_POINT('Ctrl Pts',(-50.,-8.57872964077182,-0.787298396323681));
#44951=CARTESIAN_POINT('Ctrl Pts',(-50.,-8.4787682268314,-0.77903497093039));
#44952=CARTESIAN_POINT('Ctrl Pts',(-50.,-8.37860576557482,-0.772859096585322));
#44953=CARTESIAN_POINT('Ctrl Pts',(-50.,-8.27837864239844,-0.767415604052299));
#44954=CARTESIAN_POINT('Ctrl Pts',(-50.,-8.17819997799169,-0.761523645955682));
#44955=CARTESIAN_POINT('Ctrl Pts',(-50.,-8.07814553295023,-0.75438819429077));
#44956=CARTESIAN_POINT('Ctrl Pts',(-50.,-7.97825959982878,-0.745545432905555));
#44957=CARTESIAN_POINT('Ctrl Pts',(-50.,-7.89850297873842,-0.736923545827707));
#44958=CARTESIAN_POINT('Ctrl Pts',(-50.,-7.83877406317074,-0.72955527454762));
#44959=CARTESIAN_POINT('Ctrl Pts',(-50.,-7.79899409244038,-0.724242761304609));
#44960=CARTESIAN_POINT('Ctrl Pts',(-50.,-7.77911393348366,-0.721486423905757));
#44961=CARTESIAN_POINT('Origin',(-50.,-9.49333381220606,-0.489132040720954));
#44962=CARTESIAN_POINT('',(-50.,-10.125,-1.2399548841367E-15));
#44963=CARTESIAN_POINT('Origin',(-50.,0.,0.));
#44964=CARTESIAN_POINT('Origin',(-50.,0.,0.));
#44965=CARTESIAN_POINT('Origin',(-65.75,0.,0.));
#44966=CARTESIAN_POINT('',(-65.5,-10.3067057020436,2.58117077533865));
#44967=CARTESIAN_POINT('Origin',(-65.5,0.,0.));
#44968=CARTESIAN_POINT('',(-66.,-9.74369803606849,2.75244865200334));
#44969=CARTESIAN_POINT('Ctrl Pts',(-65.5,-10.3067057020436,2.58117077533865));
#44970=CARTESIAN_POINT('Ctrl Pts',(-65.66413580978,-10.1205863175662,2.64871173156175));
#44971=CARTESIAN_POINT('Ctrl Pts',(-65.8308421033592,-9.93250310566509,
2.70633121317366));
#44972=CARTESIAN_POINT('Ctrl Pts',(-66.,-9.74369803606849,2.75244865200334));
#44973=CARTESIAN_POINT('Origin',(-66.,0.,0.));
#44974=CARTESIAN_POINT('Origin',(-58.,0.,0.));
#44975=CARTESIAN_POINT('',(-50.5,-10.3067057020436,2.58117077533865));
#44976=CARTESIAN_POINT('Origin',(-50.5,0.,0.));
#44977=CARTESIAN_POINT('Ctrl Pts',(-50.5,-10.3067057020436,2.58117077533865));
#44978=CARTESIAN_POINT('Ctrl Pts',(-55.5,-10.3067057020436,2.58117077533865));
#44979=CARTESIAN_POINT('Ctrl Pts',(-60.5,-10.3067057020436,2.58117077533865));
#44980=CARTESIAN_POINT('Ctrl Pts',(-65.5,-10.3067057020436,2.58117077533865));
#44981=CARTESIAN_POINT('Origin',(-50.25,0.,0.));
#44982=CARTESIAN_POINT('',(-50.,-9.74369803606851,2.75244865200334));
#44983=CARTESIAN_POINT('Origin',(-50.,0.,0.));
#44984=CARTESIAN_POINT('Ctrl Pts',(-50.,-9.74369803606851,2.75244865200334));
#44985=CARTESIAN_POINT('Ctrl Pts',(-50.1691578966406,-9.93250310566499,
2.70633121317368));
#44986=CARTESIAN_POINT('Ctrl Pts',(-50.3358641902207,-10.120586317567,2.64871173156144));
#44987=CARTESIAN_POINT('Ctrl Pts',(-50.5,-10.3067057020436,2.58117077533865));
#44988=CARTESIAN_POINT('Origin',(-66.,-8.87153990628942,3.4144423723866));
#44989=CARTESIAN_POINT('',(-66.,-8.57244977261306,5.38783165067601));
#44990=CARTESIAN_POINT('Origin',(-66.,0.,0.));
#44991=CARTESIAN_POINT('',(-66.,-7.40002916450246,2.50494004209942));
#44992=CARTESIAN_POINT('Ctrl Pts',(-66.,-7.40002916450246,2.50494004209942));
#44993=CARTESIAN_POINT('Ctrl Pts',(-66.,-7.41931169683537,2.51050799170683));
#44994=CARTESIAN_POINT('Ctrl Pts',(-66.,-7.45781330220401,2.52183474112154));
#44995=CARTESIAN_POINT('Ctrl Pts',(-66.,-7.51537532763652,2.53939742897549));
#44996=CARTESIAN_POINT('Ctrl Pts',(-66.,-7.59174346395756,2.56396088352458));
#44997=CARTESIAN_POINT('Ctrl Pts',(-66.,-7.68659047952439,2.59650988815641));
#44998=CARTESIAN_POINT('Ctrl Pts',(-66.,-7.78089701296599,2.63068713780068));
#44999=CARTESIAN_POINT('Ctrl Pts',(-66.,-7.87481125204483,2.66605089991351));
#45000=CARTESIAN_POINT('Ctrl Pts',(-66.,-7.96858735303469,2.70184406566216));
#45001=CARTESIAN_POINT('Ctrl Pts',(-66.,-8.06260226894112,2.73694186696096));
#45002=CARTESIAN_POINT('Ctrl Pts',(-66.,-8.15728260249069,2.77005082217159));
#45003=CARTESIAN_POINT('Ctrl Pts',(-66.,-8.25303903993759,2.79988572902344));
#45004=CARTESIAN_POINT('Ctrl Pts',(-66.,-8.35020231164278,2.8253438589765));
#45005=CARTESIAN_POINT('Ctrl Pts',(-66.,-8.44894743956675,2.84570787805295));
#45006=CARTESIAN_POINT('Ctrl Pts',(-66.,-8.54925585128769,2.86075452374925));
#45007=CARTESIAN_POINT('Ctrl Pts',(-66.,-8.65098285136142,2.87059944718567));
#45008=CARTESIAN_POINT('Ctrl Pts',(-66.,-8.7539063267339,2.87559024133729));
#45009=CARTESIAN_POINT('Ctrl Pts',(-66.,-8.85777906856656,2.87618833666037));
#45010=CARTESIAN_POINT('Ctrl Pts',(-66.,-8.96238669582476,2.87284296703405));
#45011=CARTESIAN_POINT('Ctrl Pts',(-66.,-9.06757696100992,2.86591837692133));
#45012=CARTESIAN_POINT('Ctrl Pts',(-66.,-9.17323934599399,2.85571558912008));
#45013=CARTESIAN_POINT('Ctrl Pts',(-66.,-9.27929613150859,2.8424719880915));
#45014=CARTESIAN_POINT('Ctrl Pts',(-66.,-9.38568955693702,2.82637014921091));
#45015=CARTESIAN_POINT('Ctrl Pts',(-66.,-9.49236934178897,2.80754214008259));
#45016=CARTESIAN_POINT('Ctrl Pts',(-66.,-9.58533813500313,2.78887793905502));
#45017=CARTESIAN_POINT('Ctrl Pts',(-66.,-9.65702832718653,2.77306255439687));
#45018=CARTESIAN_POINT('Ctrl Pts',(-66.,-9.70734493152456,2.76126971555027));
#45019=CARTESIAN_POINT('Ctrl Pts',(-66.,-9.73624122804054,2.75427004847764));
#45020=CARTESIAN_POINT('Ctrl Pts',(-66.,-9.74369803606849,2.75244865200334));
#45021=CARTESIAN_POINT('',(-66.,-6.81311923233407,3.82316133271924));
#45022=CARTESIAN_POINT('Origin',(-66.,0.,0.));
#45023=CARTESIAN_POINT('Ctrl Pts',(-66.,-8.57244977261306,5.38783165067601));
#45024=CARTESIAN_POINT('Ctrl Pts',(-66.,-8.56382257497052,5.36991052437482));
#45025=CARTESIAN_POINT('Ctrl Pts',(-66.,-8.54292884255608,5.32830593066664));
#45026=CARTESIAN_POINT('Ctrl Pts',(-66.,-8.5083892410637,5.2660121538642));
#45027=CARTESIAN_POINT('Ctrl Pts',(-66.,-8.45816610437014,5.18725095270768));
#45028=CARTESIAN_POINT('Ctrl Pts',(-66.,-8.39088381069298,5.09368840385081));
#45029=CARTESIAN_POINT('Ctrl Pts',(-66.,-8.31785315284231,4.99561541360302));
#45030=CARTESIAN_POINT('Ctrl Pts',(-66.,-8.24398364800048,4.89528533686678));
#45031=CARTESIAN_POINT('Ctrl Pts',(-66.,-8.16895865357096,4.79341090596642));
#45032=CARTESIAN_POINT('Ctrl Pts',(-66.,-8.09178675852221,4.69261468439531));
#45033=CARTESIAN_POINT('Ctrl Pts',(-66.,-8.01120590115509,4.59630951471431));
#45034=CARTESIAN_POINT('Ctrl Pts',(-66.,-7.92626224077336,4.50707777519311));
#45035=CARTESIAN_POINT('Ctrl Pts',(-66.,-7.8366142398488,4.42585016826903));
#45036=CARTESIAN_POINT('Ctrl Pts',(-66.,-7.74237200893774,4.35245165160981));
#45037=CARTESIAN_POINT('Ctrl Pts',(-66.,-7.64403105809269,4.28586249972102));
#45038=CARTESIAN_POINT('Ctrl Pts',(-66.,-7.54237394375965,4.22459698165889));
#45039=CARTESIAN_POINT('Ctrl Pts',(-66.,-7.43838008066255,4.16699606204881));
#45040=CARTESIAN_POINT('Ctrl Pts',(-66.,-7.33308763494517,4.1113895497456));
#45041=CARTESIAN_POINT('Ctrl Pts',(-66.,-7.22746796441592,4.05626674182128));
#45042=CARTESIAN_POINT('Ctrl Pts',(-66.,-7.1222885976642,4.00045343685988));
#45043=CARTESIAN_POINT('Ctrl Pts',(-66.,-7.01799857910513,3.94326214747216));
#45044=CARTESIAN_POINT('Ctrl Pts',(-66.,-6.93545604316326,3.89613438608228));
#45045=CARTESIAN_POINT('Ctrl Pts',(-66.,-6.8740810318698,3.85996698713255));
#45046=CARTESIAN_POINT('Ctrl Pts',(-66.,-6.83340048002394,3.83549066847637));
#45047=CARTESIAN_POINT('Ctrl Pts',(-66.,-6.81311923233407,3.82316133271924));
#45048=CARTESIAN_POINT('Ctrl Pts',(-66.,-6.81311923233407,3.82316133271924));
#45049=CARTESIAN_POINT('Ctrl Pts',(-50.,-6.81311923233407,3.82316133271924));
#45050=CARTESIAN_POINT('Ctrl Pts',(-66.,-6.83340048002394,3.83549066847637));
#45051=CARTESIAN_POINT('Ctrl Pts',(-50.,-6.83340048002394,3.83549066847637));
#45052=CARTESIAN_POINT('Ctrl Pts',(-66.,-6.8740810318698,3.85996698713255));
#45053=CARTESIAN_POINT('Ctrl Pts',(-50.,-6.8740810318698,3.85996698713255));
#45054=CARTESIAN_POINT('Ctrl Pts',(-66.,-6.93545604316326,3.89613438608228));
#45055=CARTESIAN_POINT('Ctrl Pts',(-50.,-6.93545604316326,3.89613438608228));
#45056=CARTESIAN_POINT('Ctrl Pts',(-66.,-7.01799857910513,3.94326214747216));
#45057=CARTESIAN_POINT('Ctrl Pts',(-50.,-7.01799857910513,3.94326214747216));
#45058=CARTESIAN_POINT('Ctrl Pts',(-66.,-7.1222885976642,4.00045343685988));
#45059=CARTESIAN_POINT('Ctrl Pts',(-50.,-7.1222885976642,4.00045343685988));
#45060=CARTESIAN_POINT('Ctrl Pts',(-66.,-7.22746796441592,4.05626674182128));
#45061=CARTESIAN_POINT('Ctrl Pts',(-50.,-7.22746796441592,4.05626674182128));
#45062=CARTESIAN_POINT('Ctrl Pts',(-66.,-7.33308763494517,4.1113895497456));
#45063=CARTESIAN_POINT('Ctrl Pts',(-50.,-7.33308763494517,4.1113895497456));
#45064=CARTESIAN_POINT('Ctrl Pts',(-66.,-7.43838008066255,4.16699606204881));
#45065=CARTESIAN_POINT('Ctrl Pts',(-50.,-7.43838008066255,4.16699606204881));
#45066=CARTESIAN_POINT('Ctrl Pts',(-66.,-7.54237394375965,4.22459698165889));
#45067=CARTESIAN_POINT('Ctrl Pts',(-50.,-7.54237394375965,4.22459698165889));
#45068=CARTESIAN_POINT('Ctrl Pts',(-66.,-7.64403105809269,4.28586249972102));
#45069=CARTESIAN_POINT('Ctrl Pts',(-50.,-7.64403105809269,4.28586249972102));
#45070=CARTESIAN_POINT('Ctrl Pts',(-66.,-7.74237200893774,4.35245165160981));
#45071=CARTESIAN_POINT('Ctrl Pts',(-50.,-7.74237200893774,4.35245165160981));
#45072=CARTESIAN_POINT('Ctrl Pts',(-66.,-7.8366142398488,4.42585016826903));
#45073=CARTESIAN_POINT('Ctrl Pts',(-50.,-7.8366142398488,4.42585016826903));
#45074=CARTESIAN_POINT('Ctrl Pts',(-66.,-7.92626224077336,4.50707777519311));
#45075=CARTESIAN_POINT('Ctrl Pts',(-50.,-7.92626224077336,4.50707777519311));
#45076=CARTESIAN_POINT('Ctrl Pts',(-66.,-8.01120590115509,4.59630951471431));
#45077=CARTESIAN_POINT('Ctrl Pts',(-50.,-8.01120590115509,4.59630951471431));
#45078=CARTESIAN_POINT('Ctrl Pts',(-66.,-8.09178675852221,4.69261468439531));
#45079=CARTESIAN_POINT('Ctrl Pts',(-50.,-8.09178675852221,4.69261468439531));
#45080=CARTESIAN_POINT('Ctrl Pts',(-66.,-8.16895865357096,4.79341090596642));
#45081=CARTESIAN_POINT('Ctrl Pts',(-50.,-8.16895865357096,4.79341090596642));
#45082=CARTESIAN_POINT('Ctrl Pts',(-66.,-8.24398364800048,4.89528533686678));
#45083=CARTESIAN_POINT('Ctrl Pts',(-50.,-8.24398364800048,4.89528533686678));
#45084=CARTESIAN_POINT('Ctrl Pts',(-66.,-8.31785315284231,4.99561541360302));
#45085=CARTESIAN_POINT('Ctrl Pts',(-50.,-8.31785315284231,4.99561541360302));
#45086=CARTESIAN_POINT('Ctrl Pts',(-66.,-8.39088381069298,5.09368840385081));
#45087=CARTESIAN_POINT('Ctrl Pts',(-50.,-8.39088381069298,5.09368840385081));
#45088=CARTESIAN_POINT('Ctrl Pts',(-66.,-8.46203086798835,5.19262528100548));
#45089=CARTESIAN_POINT('Ctrl Pts',(-50.,-8.46203086798835,5.19262528100548));
#45090=CARTESIAN_POINT('Ctrl Pts',(-66.,-8.52910662358075,5.29873581494822));
#45091=CARTESIAN_POINT('Ctrl Pts',(-50.,-8.52910662358075,5.29873581494822));
#45092=CARTESIAN_POINT('Ctrl Pts',(-66.,-8.59004990429128,5.41789037245987));
#45093=CARTESIAN_POINT('Ctrl Pts',(-50.,-8.59004990429128,5.41789037245987));
#45094=CARTESIAN_POINT('Ctrl Pts',(-66.,-8.64386090104433,5.55284399091502));
#45095=CARTESIAN_POINT('Ctrl Pts',(-50.,-8.64386090104433,5.55284399091502));
#45096=CARTESIAN_POINT('Ctrl Pts',(-66.,-8.69181195387006,5.6997708284895));
#45097=CARTESIAN_POINT('Ctrl Pts',(-50.,-8.69181195387006,5.6997708284895));
#45098=CARTESIAN_POINT('Ctrl Pts',(-66.,-8.73814647121154,5.8462701562578));
#45099=CARTESIAN_POINT('Ctrl Pts',(-50.,-8.73814647121154,5.8462701562578));
#45100=CARTESIAN_POINT('Ctrl Pts',(-66.,-8.78885790167157,5.97489878611032));
#45101=CARTESIAN_POINT('Ctrl Pts',(-50.,-8.78885790167157,5.97489878611032));
#45102=CARTESIAN_POINT('Ctrl Pts',(-66.,-8.85073384792934,6.06594096807997));
#45103=CARTESIAN_POINT('Ctrl Pts',(-50.,-8.85073384792934,6.06594096807997));
#45104=CARTESIAN_POINT('Ctrl Pts',(-66.,-8.93034007876537,6.10035075259139));
#45105=CARTESIAN_POINT('Ctrl Pts',(-50.,-8.93034007876537,6.10035075259139));
#45106=CARTESIAN_POINT('Ctrl Pts',(-66.,-9.03293161543166,6.06290773317823));
#45107=CARTESIAN_POINT('Ctrl Pts',(-50.,-9.03293161543166,6.06290773317823));
#45108=CARTESIAN_POINT('Ctrl Pts',(-66.,-9.1625061724433,5.9420559998861));
#45109=CARTESIAN_POINT('Ctrl Pts',(-50.,-9.1625061724433,5.9420559998861));
#45110=CARTESIAN_POINT('Ctrl Pts',(-66.,-9.32201962027199,5.72927334958384));
#45111=CARTESIAN_POINT('Ctrl Pts',(-50.,-9.32201962027199,5.72927334958384));
#45112=CARTESIAN_POINT('Ctrl Pts',(-66.,-9.51353468950136,5.41863469758916));
#45113=CARTESIAN_POINT('Ctrl Pts',(-50.,-9.51353468950136,5.41863469758916));
#45114=CARTESIAN_POINT('Ctrl Pts',(-66.,-9.7383890962382,5.00631957015997));
#45115=CARTESIAN_POINT('Ctrl Pts',(-50.,-9.7383890962382,5.00631957015997));
#45116=CARTESIAN_POINT('Ctrl Pts',(-66.,-9.99734717600606,4.4901678734951));
#45117=CARTESIAN_POINT('Ctrl Pts',(-50.,-9.99734717600606,4.4901678734951));
#45118=CARTESIAN_POINT('Ctrl Pts',(-66.,-10.2907511765059,3.86923704869354));
#45119=CARTESIAN_POINT('Ctrl Pts',(-50.,-10.2907511765059,3.86923704869354));
#45120=CARTESIAN_POINT('Ctrl Pts',(-66.,-10.553083029885,3.28855031576864));
#45121=CARTESIAN_POINT('Ctrl Pts',(-50.,-10.553083029885,3.28855031576864));
#45122=CARTESIAN_POINT('Ctrl Pts',(-66.,-10.765329928439,2.80592201479919));
#45123=CARTESIAN_POINT('Ctrl Pts',(-50.,-10.765329928439,2.80592201479919));
#45124=CARTESIAN_POINT('Ctrl Pts',(-66.,-10.9137067077809,2.46325842726184));
#45125=CARTESIAN_POINT('Ctrl Pts',(-50.,-10.9137067077809,2.46325842726184));
#45126=CARTESIAN_POINT('Ctrl Pts',(-66.,-10.9896148096924,2.28669878527756));
#45127=CARTESIAN_POINT('Ctrl Pts',(-50.,-10.9896148096924,2.28669878527756));
#45128=CARTESIAN_POINT('',(-65.5,-8.79190251708467,5.96599322242996));
#45129=CARTESIAN_POINT('Ctrl Pts',(-66.,-8.57244977261307,5.38783165067601));
#45130=CARTESIAN_POINT('Ctrl Pts',(-65.7982417703062,-8.67580691746,5.60253363429554));
#45131=CARTESIAN_POINT('Ctrl Pts',(-65.6331946192803,-8.72156901755385,
5.83243162948398));
#45132=CARTESIAN_POINT('Ctrl Pts',(-65.5,-8.79190251708467,5.96599322242995));
#45133=CARTESIAN_POINT('',(-50.,-6.81311923233407,3.82316133271924));
#45134=CARTESIAN_POINT('',(-66.,-6.81311923233407,3.82316133271924));
#45135=CARTESIAN_POINT('',(-50.,-8.57244977261307,5.38783165067603));
#45136=CARTESIAN_POINT('Ctrl Pts',(-50.,-6.81311923233407,3.82316133271924));
#45137=CARTESIAN_POINT('Ctrl Pts',(-50.,-6.83340048002394,3.83549066847637));
#45138=CARTESIAN_POINT('Ctrl Pts',(-50.,-6.8740810318698,3.85996698713255));
#45139=CARTESIAN_POINT('Ctrl Pts',(-50.,-6.93545604316326,3.89613438608228));
#45140=CARTESIAN_POINT('Ctrl Pts',(-50.,-7.01799857910513,3.94326214747216));
#45141=CARTESIAN_POINT('Ctrl Pts',(-50.,-7.1222885976642,4.00045343685988));
#45142=CARTESIAN_POINT('Ctrl Pts',(-50.,-7.22746796441592,4.05626674182128));
#45143=CARTESIAN_POINT('Ctrl Pts',(-50.,-7.33308763494517,4.1113895497456));
#45144=CARTESIAN_POINT('Ctrl Pts',(-50.,-7.43838008066255,4.16699606204881));
#45145=CARTESIAN_POINT('Ctrl Pts',(-50.,-7.54237394375965,4.22459698165889));
#45146=CARTESIAN_POINT('Ctrl Pts',(-50.,-7.64403105809269,4.28586249972102));
#45147=CARTESIAN_POINT('Ctrl Pts',(-50.,-7.74237200893774,4.35245165160981));
#45148=CARTESIAN_POINT('Ctrl Pts',(-50.,-7.8366142398488,4.42585016826903));
#45149=CARTESIAN_POINT('Ctrl Pts',(-50.,-7.92626224077336,4.50707777519311));
#45150=CARTESIAN_POINT('Ctrl Pts',(-50.,-8.01120590115509,4.59630951471431));
#45151=CARTESIAN_POINT('Ctrl Pts',(-50.,-8.09178675852221,4.69261468439531));
#45152=CARTESIAN_POINT('Ctrl Pts',(-50.,-8.16895865357096,4.79341090596642));
#45153=CARTESIAN_POINT('Ctrl Pts',(-50.,-8.24398364800048,4.89528533686678));
#45154=CARTESIAN_POINT('Ctrl Pts',(-50.,-8.31785315284231,4.99561541360302));
#45155=CARTESIAN_POINT('Ctrl Pts',(-50.,-8.39088381069298,5.09368840385081));
#45156=CARTESIAN_POINT('Ctrl Pts',(-50.,-8.45816610437014,5.18725095270769));
#45157=CARTESIAN_POINT('Ctrl Pts',(-50.,-8.5083892410637,5.26601215386421));
#45158=CARTESIAN_POINT('Ctrl Pts',(-50.,-8.54292884255608,5.32830593066665));
#45159=CARTESIAN_POINT('Ctrl Pts',(-50.,-8.56382257497053,5.36991052437484));
#45160=CARTESIAN_POINT('Ctrl Pts',(-50.,-8.57244977261307,5.38783165067603));
#45161=CARTESIAN_POINT('',(-50.5,-8.79190251708467,5.96599322242996));
#45162=CARTESIAN_POINT('Ctrl Pts',(-50.5,-8.79190251708468,5.96599322242997));
#45163=CARTESIAN_POINT('Ctrl Pts',(-50.4513355279182,-8.76620521307325,
5.91719467151072));
#45164=CARTESIAN_POINT('Ctrl Pts',(-50.3988319785486,-8.74374680112151,
5.85659632440327));
#45165=CARTESIAN_POINT('Ctrl Pts',(-50.2385977000686,-8.67884981036978,
5.66466221597345));
#45166=CARTESIAN_POINT('Ctrl Pts',(-50.1319260151113,-8.64003311864876,
5.52822134966582));
#45167=CARTESIAN_POINT('Ctrl Pts',(-50.,-8.57244977261307,5.38783165067603));
#45168=CARTESIAN_POINT('Ctrl Pts',(-65.5,-8.79190251708467,5.96599322242996));
#45169=CARTESIAN_POINT('Ctrl Pts',(-60.5,-8.79190251708467,5.96599322242996));
#45170=CARTESIAN_POINT('Ctrl Pts',(-55.5,-8.79190251708467,5.96599322242996));
#45171=CARTESIAN_POINT('Ctrl Pts',(-50.5,-8.79190251708467,5.96599322242996));
#45172=CARTESIAN_POINT('Origin',(-66.,0.,0.));
#45173=CARTESIAN_POINT('',(-50.,-7.40002916450246,2.50494004209942));
#45174=CARTESIAN_POINT('',(-66.,-7.40002916450246,2.50494004209942));
#45175=CARTESIAN_POINT('Origin',(-50.,0.,0.));
#45176=CARTESIAN_POINT('Ctrl Pts',(-66.,-10.9896148096924,2.28669878527756));
#45177=CARTESIAN_POINT('Ctrl Pts',(-50.,-10.9896148096924,2.28669878527756));
#45178=CARTESIAN_POINT('Ctrl Pts',(-66.,-10.9684161512126,2.29727350719238));
#45179=CARTESIAN_POINT('Ctrl Pts',(-50.,-10.9684161512126,2.29727350719238));
#45180=CARTESIAN_POINT('Ctrl Pts',(-66.,-10.9259986747394,2.31821040407718));
#45181=CARTESIAN_POINT('Ctrl Pts',(-50.,-10.9259986747394,2.31821040407718));
#45182=CARTESIAN_POINT('Ctrl Pts',(-66.,-10.8623119817454,2.34897810856224));
#45183=CARTESIAN_POINT('Ctrl Pts',(-50.,-10.8623119817454,2.34897810856224));
#45184=CARTESIAN_POINT('Ctrl Pts',(-66.,-10.7772752714148,2.3887247370365));
#45185=CARTESIAN_POINT('Ctrl Pts',(-50.,-10.7772752714148,2.3887247370365));
#45186=CARTESIAN_POINT('Ctrl Pts',(-66.,-10.6707784343856,2.4362669175464));
#45187=CARTESIAN_POINT('Ctrl Pts',(-50.,-10.6707784343856,2.4362669175464));
#45188=CARTESIAN_POINT('Ctrl Pts',(-66.,-10.5640849911537,2.48164669841744));
#45189=CARTESIAN_POINT('Ctrl Pts',(-50.,-10.5640849911537,2.48164669841744));
#45190=CARTESIAN_POINT('Ctrl Pts',(-66.,-10.4572049564432,2.52483446494625));
#45191=CARTESIAN_POINT('Ctrl Pts',(-50.,-10.4572049564432,2.52483446494625));
#45192=CARTESIAN_POINT('Ctrl Pts',(-66.,-10.3501560465217,2.56579274006262));
#45193=CARTESIAN_POINT('Ctrl Pts',(-50.,-10.3501560465217,2.56579274006262));
#45194=CARTESIAN_POINT('Ctrl Pts',(-66.,-10.2429664006725,2.60447642727633));
#45195=CARTESIAN_POINT('Ctrl Pts',(-50.,-10.2429664006725,2.60447642727633));
#45196=CARTESIAN_POINT('Ctrl Pts',(-66.,-10.1356731120406,2.64083547340864));
#45197=CARTESIAN_POINT('Ctrl Pts',(-50.,-10.1356731120406,2.64083547340864));
#45198=CARTESIAN_POINT('Ctrl Pts',(-66.,-10.0283197583604,2.67481805512507));
#45199=CARTESIAN_POINT('Ctrl Pts',(-50.,-10.0283197583604,2.67481805512507));
#45200=CARTESIAN_POINT('Ctrl Pts',(-66.,-9.92095426270504,2.70637422995761));
#45201=CARTESIAN_POINT('Ctrl Pts',(-50.,-9.92095426270504,2.70637422995761));
#45202=CARTESIAN_POINT('Ctrl Pts',(-66.,-9.8136267879847,2.73545878100293));
#45203=CARTESIAN_POINT('Ctrl Pts',(-50.,-9.8136267879847,2.73545878100293));
#45204=CARTESIAN_POINT('Ctrl Pts',(-66.,-9.70638729315513,2.7620369717482));
#45205=CARTESIAN_POINT('Ctrl Pts',(-50.,-9.70638729315513,2.7620369717482));
#45206=CARTESIAN_POINT('Ctrl Pts',(-66.,-9.59928504165258,2.78607799016444));
#45207=CARTESIAN_POINT('Ctrl Pts',(-50.,-9.59928504165258,2.78607799016444));
#45208=CARTESIAN_POINT('Ctrl Pts',(-66.,-9.49236934178897,2.80754214008259));
#45209=CARTESIAN_POINT('Ctrl Pts',(-50.,-9.49236934178897,2.80754214008259));
#45210=CARTESIAN_POINT('Ctrl Pts',(-66.,-9.38568955693702,2.82637014921091));
#45211=CARTESIAN_POINT('Ctrl Pts',(-50.,-9.38568955693702,2.82637014921091));
#45212=CARTESIAN_POINT('Ctrl Pts',(-66.,-9.27929613150859,2.8424719880915));
#45213=CARTESIAN_POINT('Ctrl Pts',(-50.,-9.27929613150859,2.8424719880915));
#45214=CARTESIAN_POINT('Ctrl Pts',(-66.,-9.17323934599399,2.85571558912008));
#45215=CARTESIAN_POINT('Ctrl Pts',(-50.,-9.17323934599399,2.85571558912008));
#45216=CARTESIAN_POINT('Ctrl Pts',(-66.,-9.06757696100992,2.86591837692133));
#45217=CARTESIAN_POINT('Ctrl Pts',(-50.,-9.06757696100992,2.86591837692133));
#45218=CARTESIAN_POINT('Ctrl Pts',(-66.,-8.96238669582476,2.87284296703405));
#45219=CARTESIAN_POINT('Ctrl Pts',(-50.,-8.96238669582476,2.87284296703405));
#45220=CARTESIAN_POINT('Ctrl Pts',(-66.,-8.85777906856656,2.87618833666037));
#45221=CARTESIAN_POINT('Ctrl Pts',(-50.,-8.85777906856656,2.87618833666037));
#45222=CARTESIAN_POINT('Ctrl Pts',(-66.,-8.7539063267339,2.87559024133729));
#45223=CARTESIAN_POINT('Ctrl Pts',(-50.,-8.7539063267339,2.87559024133729));
#45224=CARTESIAN_POINT('Ctrl Pts',(-66.,-8.65098285136142,2.87059944718567));
#45225=CARTESIAN_POINT('Ctrl Pts',(-50.,-8.65098285136142,2.87059944718567));
#45226=CARTESIAN_POINT('Ctrl Pts',(-66.,-8.54925585128769,2.86075452374925));
#45227=CARTESIAN_POINT('Ctrl Pts',(-50.,-8.54925585128769,2.86075452374925));
#45228=CARTESIAN_POINT('Ctrl Pts',(-66.,-8.44894743956675,2.84570787805295));
#45229=CARTESIAN_POINT('Ctrl Pts',(-50.,-8.44894743956675,2.84570787805295));
#45230=CARTESIAN_POINT('Ctrl Pts',(-66.,-8.35020231164278,2.8253438589765));
#45231=CARTESIAN_POINT('Ctrl Pts',(-50.,-8.35020231164278,2.8253438589765));
#45232=CARTESIAN_POINT('Ctrl Pts',(-66.,-8.25303903993759,2.79988572902344));
#45233=CARTESIAN_POINT('Ctrl Pts',(-50.,-8.25303903993759,2.79988572902344));
#45234=CARTESIAN_POINT('Ctrl Pts',(-66.,-8.15728260249069,2.77005082217159));
#45235=CARTESIAN_POINT('Ctrl Pts',(-50.,-8.15728260249069,2.77005082217159));
#45236=CARTESIAN_POINT('Ctrl Pts',(-66.,-8.06260226894112,2.73694186696096));
#45237=CARTESIAN_POINT('Ctrl Pts',(-50.,-8.06260226894112,2.73694186696096));
#45238=CARTESIAN_POINT('Ctrl Pts',(-66.,-7.96858735303469,2.70184406566216));
#45239=CARTESIAN_POINT('Ctrl Pts',(-50.,-7.96858735303469,2.70184406566216));
#45240=CARTESIAN_POINT('Ctrl Pts',(-66.,-7.87481125204483,2.66605089991351));
#45241=CARTESIAN_POINT('Ctrl Pts',(-50.,-7.87481125204483,2.66605089991351));
#45242=CARTESIAN_POINT('Ctrl Pts',(-66.,-7.78089701296599,2.63068713780068));
#45243=CARTESIAN_POINT('Ctrl Pts',(-50.,-7.78089701296599,2.63068713780068));
#45244=CARTESIAN_POINT('Ctrl Pts',(-66.,-7.68659047952439,2.59650988815641));
#45245=CARTESIAN_POINT('Ctrl Pts',(-50.,-7.68659047952439,2.59650988815641));
#45246=CARTESIAN_POINT('Ctrl Pts',(-66.,-7.59174346395756,2.56396088352458));
#45247=CARTESIAN_POINT('Ctrl Pts',(-50.,-7.59174346395756,2.56396088352458));
#45248=CARTESIAN_POINT('Ctrl Pts',(-66.,-7.51537532763652,2.53939742897549));
#45249=CARTESIAN_POINT('Ctrl Pts',(-50.,-7.51537532763652,2.53939742897549));
#45250=CARTESIAN_POINT('Ctrl Pts',(-66.,-7.45781330220401,2.52183474112154));
#45251=CARTESIAN_POINT('Ctrl Pts',(-50.,-7.45781330220401,2.52183474112154));
#45252=CARTESIAN_POINT('Ctrl Pts',(-66.,-7.41931169683537,2.51050799170683));
#45253=CARTESIAN_POINT('Ctrl Pts',(-50.,-7.41931169683537,2.51050799170683));
#45254=CARTESIAN_POINT('Ctrl Pts',(-66.,-7.40002916450246,2.50494004209942));
#45255=CARTESIAN_POINT('Ctrl Pts',(-50.,-7.40002916450246,2.50494004209942));
#45256=CARTESIAN_POINT('Ctrl Pts',(-50.,-9.74369803606851,2.75244865200334));
#45257=CARTESIAN_POINT('Ctrl Pts',(-50.,-9.73624122804056,2.75427004847764));
#45258=CARTESIAN_POINT('Ctrl Pts',(-50.,-9.70734493152457,2.76126971555026));
#45259=CARTESIAN_POINT('Ctrl Pts',(-50.,-9.65702832718653,2.77306255439687));
#45260=CARTESIAN_POINT('Ctrl Pts',(-50.,-9.58533813500313,2.78887793905502));
#45261=CARTESIAN_POINT('Ctrl Pts',(-50.,-9.49236934178897,2.80754214008259));
#45262=CARTESIAN_POINT('Ctrl Pts',(-50.,-9.38568955693702,2.82637014921091));
#45263=CARTESIAN_POINT('Ctrl Pts',(-50.,-9.27929613150859,2.8424719880915));
#45264=CARTESIAN_POINT('Ctrl Pts',(-50.,-9.17323934599399,2.85571558912008));
#45265=CARTESIAN_POINT('Ctrl Pts',(-50.,-9.06757696100992,2.86591837692133));
#45266=CARTESIAN_POINT('Ctrl Pts',(-50.,-8.96238669582476,2.87284296703405));
#45267=CARTESIAN_POINT('Ctrl Pts',(-50.,-8.85777906856656,2.87618833666037));
#45268=CARTESIAN_POINT('Ctrl Pts',(-50.,-8.7539063267339,2.87559024133729));
#45269=CARTESIAN_POINT('Ctrl Pts',(-50.,-8.65098285136142,2.87059944718567));
#45270=CARTESIAN_POINT('Ctrl Pts',(-50.,-8.54925585128769,2.86075452374925));
#45271=CARTESIAN_POINT('Ctrl Pts',(-50.,-8.44894743956675,2.84570787805295));
#45272=CARTESIAN_POINT('Ctrl Pts',(-50.,-8.35020231164278,2.8253438589765));
#45273=CARTESIAN_POINT('Ctrl Pts',(-50.,-8.25303903993759,2.79988572902344));
#45274=CARTESIAN_POINT('Ctrl Pts',(-50.,-8.15728260249069,2.77005082217159));
#45275=CARTESIAN_POINT('Ctrl Pts',(-50.,-8.06260226894112,2.73694186696096));
#45276=CARTESIAN_POINT('Ctrl Pts',(-50.,-7.96858735303469,2.70184406566216));
#45277=CARTESIAN_POINT('Ctrl Pts',(-50.,-7.87481125204483,2.66605089991351));
#45278=CARTESIAN_POINT('Ctrl Pts',(-50.,-7.78089701296599,2.63068713780068));
#45279=CARTESIAN_POINT('Ctrl Pts',(-50.,-7.68659047952439,2.59650988815641));
#45280=CARTESIAN_POINT('Ctrl Pts',(-50.,-7.59174346395756,2.56396088352458));
#45281=CARTESIAN_POINT('Ctrl Pts',(-50.,-7.51537532763652,2.53939742897549));
#45282=CARTESIAN_POINT('Ctrl Pts',(-50.,-7.45781330220401,2.52183474112154));
#45283=CARTESIAN_POINT('Ctrl Pts',(-50.,-7.41931169683537,2.51050799170683));
#45284=CARTESIAN_POINT('Ctrl Pts',(-50.,-7.40002916450246,2.50494004209942));
#45285=CARTESIAN_POINT('Origin',(-50.,-8.87153990628942,3.4144423723866));
#45286=CARTESIAN_POINT('Origin',(-50.,0.,0.));
#45287=CARTESIAN_POINT('Origin',(-65.75,0.,0.));
#45288=CARTESIAN_POINT('',(-65.5,-8.3657874409944,6.55013171562987));
#45289=CARTESIAN_POINT('Origin',(-65.5,0.,0.));
#45290=CARTESIAN_POINT('',(-66.,-7.78178935653715,6.47760599376692));
#45291=CARTESIAN_POINT('Ctrl Pts',(-65.5,-8.36578744099439,6.55013171562987));
#45292=CARTESIAN_POINT('Ctrl Pts',(-65.6642917360002,-8.16809991938447,
6.5361185761295));
#45293=CARTESIAN_POINT('Ctrl Pts',(-65.831118235484,-7.97271684425891,6.51221297265958));
#45294=CARTESIAN_POINT('Ctrl Pts',(-66.,-7.78178935653715,6.47760599376692));
#45295=CARTESIAN_POINT('Origin',(-66.,0.,0.));
#45296=CARTESIAN_POINT('Origin',(-58.,0.,0.));
#45297=CARTESIAN_POINT('',(-50.5,-8.3657874409944,6.55013171562987));
#45298=CARTESIAN_POINT('Origin',(-50.5,0.,0.));
#45299=CARTESIAN_POINT('Ctrl Pts',(-50.5,-8.3657874409944,6.55013171562987));
#45300=CARTESIAN_POINT('Ctrl Pts',(-55.5,-8.3657874409944,6.55013171562987));
#45301=CARTESIAN_POINT('Ctrl Pts',(-60.5,-8.3657874409944,6.55013171562987));
#45302=CARTESIAN_POINT('Ctrl Pts',(-65.5,-8.3657874409944,6.55013171562987));
#45303=CARTESIAN_POINT('Origin',(-50.25,0.,0.));
#45304=CARTESIAN_POINT('',(-50.,-7.78178935653717,6.47760599376692));
#45305=CARTESIAN_POINT('Origin',(-50.,0.,0.));
#45306=CARTESIAN_POINT('Ctrl Pts',(-50.,-7.78178935653716,6.47760599376692));
#45307=CARTESIAN_POINT('Ctrl Pts',(-50.1688817645156,-7.97271684425845,
6.5122129726595));
#45308=CARTESIAN_POINT('Ctrl Pts',(-50.3357082639993,-8.16809991938399,
6.53611857612945));
#45309=CARTESIAN_POINT('Ctrl Pts',(-50.5,-8.36578744099441,6.55013171562987));
#45310=CARTESIAN_POINT('Origin',(-66.,-6.71577615516547,6.72762868007336));
#45311=CARTESIAN_POINT('',(-66.,-5.63989399158651,8.40875857446665));
#45312=CARTESIAN_POINT('Origin',(-66.,0.,0.));
#45313=CARTESIAN_POINT('',(-66.,-5.74141212582432,5.29823961815974));
#45314=CARTESIAN_POINT('Ctrl Pts',(-66.,-5.74141212582432,5.29823961815974));
#45315=CARTESIAN_POINT('Ctrl Pts',(-66.,-5.75676290651676,5.31116910570307));
#45316=CARTESIAN_POINT('Ctrl Pts',(-66.,-5.78732886917933,5.33717661990139));
#45317=CARTESIAN_POINT('Ctrl Pts',(-66.,-5.8327710073448,5.37663351860743));
#45318=CARTESIAN_POINT('Ctrl Pts',(-66.,-5.89254591434388,5.43013507033993));
#45319=CARTESIAN_POINT('Ctrl Pts',(-66.,-5.96595410170651,5.49844782238954));
#45320=CARTESIAN_POINT('Ctrl Pts',(-66.,-6.03820626716823,5.56802821638893));
#45321=CARTESIAN_POINT('Ctrl Pts',(-66.,-6.10961745579836,5.63853298297221));
#45322=CARTESIAN_POINT('Ctrl Pts',(-66.,-6.18072779481142,5.70937384347389));
#45323=CARTESIAN_POINT('Ctrl Pts',(-66.,-6.25233913230877,5.77967659171849));
#45324=CARTESIAN_POINT('Ctrl Pts',(-66.,-6.32536729565295,5.8484330883917));
#45325=CARTESIAN_POINT('Ctrl Pts',(-66.,-6.4007102042632,5.91463628394544));
#45326=CARTESIAN_POINT('Ctrl Pts',(-66.,-6.47911851546308,5.97741330588777));
#45327=CARTESIAN_POINT('Ctrl Pts',(-66.,-6.56104388578368,6.03618002486629));
#45328=CARTESIAN_POINT('Ctrl Pts',(-66.,-6.64656015751461,6.09072492635055));
#45329=CARTESIAN_POINT('Ctrl Pts',(-66.,-6.73548810524172,6.14109480995689));
#45330=CARTESIAN_POINT('Ctrl Pts',(-66.,-6.82748343979352,6.18751687615083));
#45331=CARTESIAN_POINT('Ctrl Pts',(-66.,-6.92213264398368,6.23031211373657));
#45332=CARTESIAN_POINT('Ctrl Pts',(-66.,-7.01905715111184,6.26980372166142));
#45333=CARTESIAN_POINT('Ctrl Pts',(-66.,-7.11796972459708,6.30626252916358));
#45334=CARTESIAN_POINT('Ctrl Pts',(-66.,-7.21864696410326,6.33991858248025));
#45335=CARTESIAN_POINT('Ctrl Pts',(-66.,-7.3209213165869,6.37095713183339));
#45336=CARTESIAN_POINT('Ctrl Pts',(-66.,-7.42466575500371,6.39952147476842));
#45337=CARTESIAN_POINT('Ctrl Pts',(-66.,-7.52978062910616,6.42571181012752));
#45338=CARTESIAN_POINT('Ctrl Pts',(-66.,-7.62230326232111,6.44647502892099));
#45339=CARTESIAN_POINT('Ctrl Pts',(-66.,-7.69422820821259,6.46118598421581));
#45340=CARTESIAN_POINT('Ctrl Pts',(-66.,-7.7449912932344,6.47087829659421));
#45341=CARTESIAN_POINT('Ctrl Pts',(-66.,-7.77423639474703,6.47623696517724));
#45342=CARTESIAN_POINT('Ctrl Pts',(-66.,-7.78178935653715,6.47760599376692));
#45343=CARTESIAN_POINT('',(-66.,-4.66907432066881,6.26377691477523));
#45344=CARTESIAN_POINT('Origin',(-66.,0.,0.));
#45345=CARTESIAN_POINT('Ctrl Pts',(-66.,-5.63989399158651,8.40875857446665));
#45346=CARTESIAN_POINT('Ctrl Pts',(-66.,-5.63930183311986,8.38887781353008));
#45347=CARTESIAN_POINT('Ctrl Pts',(-66.,-5.63713657156084,8.34237187934733));
#45348=CARTESIAN_POINT('Ctrl Pts',(-66.,-5.63092023716983,8.27141516094587));
#45349=CARTESIAN_POINT('Ctrl Pts',(-66.,-5.61707418533788,8.17903563336739));
#45350=CARTESIAN_POINT('Ctrl Pts',(-66.,-5.593664068609,8.06619581758504));
#45351=CARTESIAN_POINT('Ctrl Pts',(-66.,-5.56683712169066,7.94689743821095));
#45352=CARTESIAN_POINT('Ctrl Pts',(-66.,-5.54016188969533,7.82519591791858));
#45353=CARTESIAN_POINT('Ctrl Pts',(-66.,-5.51305921086426,7.70161357993859));
#45354=CARTESIAN_POINT('Ctrl Pts',(-66.,-5.48355669348136,7.57814301204284));
#45355=CARTESIAN_POINT('Ctrl Pts',(-66.,-5.44911325868757,7.45738867431159));
#45356=CARTESIAN_POINT('Ctrl Pts',(-66.,-5.40780718177897,7.34132172472021));
#45357=CARTESIAN_POINT('Ctrl Pts',(-66.,-5.35894790191298,7.23065348642503));
#45358=CARTESIAN_POINT('Ctrl Pts',(-66.,-5.3027072062188,7.12526883629655));
#45359=CARTESIAN_POINT('Ctrl Pts',(-66.,-5.23995252537855,7.02443775083668));
#45360=CARTESIAN_POINT('Ctrl Pts',(-66.,-5.17200306149544,6.92712124167231));
#45361=CARTESIAN_POINT('Ctrl Pts',(-66.,-5.10042834492066,6.83220206842988));
#45362=CARTESIAN_POINT('Ctrl Pts',(-66.,-5.02685611555883,6.7385766957876));
#45363=CARTESIAN_POINT('Ctrl Pts',(-66.,-4.95278821116117,6.645260114762));
#45364=CARTESIAN_POINT('Ctrl Pts',(-66.,-4.87940339472638,6.55149182098506));
#45365=CARTESIAN_POINT('Ctrl Pts',(-66.,-4.80739151505302,6.45682640629315));
#45366=CARTESIAN_POINT('Ctrl Pts',(-66.,-4.75115374374443,6.3801999799666));
#45367=CARTESIAN_POINT('Ctrl Pts',(-66.,-4.70979548740211,6.32219595087909));
#45368=CARTESIAN_POINT('Ctrl Pts',(-66.,-4.68258736973401,6.28328945005467));
#45369=CARTESIAN_POINT('Ctrl Pts',(-66.,-4.66907432066881,6.26377691477523));
#45370=CARTESIAN_POINT('Ctrl Pts',(-66.,-4.66907432066881,6.26377691477523));
#45371=CARTESIAN_POINT('Ctrl Pts',(-50.,-4.66907432066881,6.26377691477523));
#45372=CARTESIAN_POINT('Ctrl Pts',(-66.,-4.68258736973401,6.28328945005467));
#45373=CARTESIAN_POINT('Ctrl Pts',(-50.,-4.68258736973401,6.28328945005467));
#45374=CARTESIAN_POINT('Ctrl Pts',(-66.,-4.70979548740211,6.32219595087909));
#45375=CARTESIAN_POINT('Ctrl Pts',(-50.,-4.70979548740211,6.32219595087909));
#45376=CARTESIAN_POINT('Ctrl Pts',(-66.,-4.75115374374443,6.3801999799666));
#45377=CARTESIAN_POINT('Ctrl Pts',(-50.,-4.75115374374443,6.3801999799666));
#45378=CARTESIAN_POINT('Ctrl Pts',(-66.,-4.80739151505302,6.45682640629315));
#45379=CARTESIAN_POINT('Ctrl Pts',(-50.,-4.80739151505302,6.45682640629315));
#45380=CARTESIAN_POINT('Ctrl Pts',(-66.,-4.87940339472638,6.55149182098506));
#45381=CARTESIAN_POINT('Ctrl Pts',(-50.,-4.87940339472638,6.55149182098506));
#45382=CARTESIAN_POINT('Ctrl Pts',(-66.,-4.95278821116117,6.645260114762));
#45383=CARTESIAN_POINT('Ctrl Pts',(-50.,-4.95278821116117,6.645260114762));
#45384=CARTESIAN_POINT('Ctrl Pts',(-66.,-5.02685611555883,6.7385766957876));
#45385=CARTESIAN_POINT('Ctrl Pts',(-50.,-5.02685611555883,6.7385766957876));
#45386=CARTESIAN_POINT('Ctrl Pts',(-66.,-5.10042834492066,6.83220206842988));
#45387=CARTESIAN_POINT('Ctrl Pts',(-50.,-5.10042834492066,6.83220206842988));
#45388=CARTESIAN_POINT('Ctrl Pts',(-66.,-5.17200306149544,6.92712124167231));
#45389=CARTESIAN_POINT('Ctrl Pts',(-50.,-5.17200306149544,6.92712124167231));
#45390=CARTESIAN_POINT('Ctrl Pts',(-66.,-5.23995252537855,7.02443775083668));
#45391=CARTESIAN_POINT('Ctrl Pts',(-50.,-5.23995252537855,7.02443775083668));
#45392=CARTESIAN_POINT('Ctrl Pts',(-66.,-5.3027072062188,7.12526883629655));
#45393=CARTESIAN_POINT('Ctrl Pts',(-50.,-5.3027072062188,7.12526883629655));
#45394=CARTESIAN_POINT('Ctrl Pts',(-66.,-5.35894790191298,7.23065348642503));
#45395=CARTESIAN_POINT('Ctrl Pts',(-50.,-5.35894790191298,7.23065348642503));
#45396=CARTESIAN_POINT('Ctrl Pts',(-66.,-5.40780718177897,7.34132172472021));
#45397=CARTESIAN_POINT('Ctrl Pts',(-50.,-5.40780718177897,7.34132172472021));
#45398=CARTESIAN_POINT('Ctrl Pts',(-66.,-5.44911325868757,7.45738867431159));
#45399=CARTESIAN_POINT('Ctrl Pts',(-50.,-5.44911325868757,7.45738867431159));
#45400=CARTESIAN_POINT('Ctrl Pts',(-66.,-5.48355669348136,7.57814301204284));
#45401=CARTESIAN_POINT('Ctrl Pts',(-50.,-5.48355669348136,7.57814301204284));
#45402=CARTESIAN_POINT('Ctrl Pts',(-66.,-5.51305921086426,7.70161357993859));
#45403=CARTESIAN_POINT('Ctrl Pts',(-50.,-5.51305921086426,7.70161357993859));
#45404=CARTESIAN_POINT('Ctrl Pts',(-66.,-5.54016188969533,7.82519591791858));
#45405=CARTESIAN_POINT('Ctrl Pts',(-50.,-5.54016188969533,7.82519591791858));
#45406=CARTESIAN_POINT('Ctrl Pts',(-66.,-5.56683712169066,7.94689743821095));
#45407=CARTESIAN_POINT('Ctrl Pts',(-50.,-5.56683712169066,7.94689743821095));
#45408=CARTESIAN_POINT('Ctrl Pts',(-66.,-5.593664068609,8.06619581758504));
#45409=CARTESIAN_POINT('Ctrl Pts',(-50.,-5.593664068609,8.06619581758504));
#45410=CARTESIAN_POINT('Ctrl Pts',(-66.,-5.61841888633553,8.18551726755207));
#45411=CARTESIAN_POINT('Ctrl Pts',(-50.,-5.61841888633553,8.18551726755207));
#45412=CARTESIAN_POINT('Ctrl Pts',(-66.,-5.63653659580406,8.30973623150492));
#45413=CARTESIAN_POINT('Ctrl Pts',(-50.,-5.63653659580406,8.30973623150492));
#45414=CARTESIAN_POINT('Ctrl Pts',(-66.,-5.64374652834153,8.44337720169133));
#45415=CARTESIAN_POINT('Ctrl Pts',(-50.,-5.64374652834153,8.44337720169133));
#45416=CARTESIAN_POINT('Ctrl Pts',(-66.,-5.63801473825513,8.58855037100336));
#45417=CARTESIAN_POINT('Ctrl Pts',(-50.,-5.63801473825513,8.58855037100336));
#45418=CARTESIAN_POINT('Ctrl Pts',(-66.,-5.62205967606046,8.74227816633361));
#45419=CARTESIAN_POINT('Ctrl Pts',(-50.,-5.62205967606046,8.74227816633361));
#45420=CARTESIAN_POINT('Ctrl Pts',(-66.,-5.60480171912049,8.89495790780604));
#45421=CARTESIAN_POINT('Ctrl Pts',(-50.,-5.60480171912049,8.89495790780604));
#45422=CARTESIAN_POINT('Ctrl Pts',(-66.,-5.59881093895816,9.0330922053215));
#45423=CARTESIAN_POINT('Ctrl Pts',(-50.,-5.59881093895816,9.0330922053215));
#45424=CARTESIAN_POINT('Ctrl Pts',(-66.,-5.61830723712665,9.14143059178176));
#45425=CARTESIAN_POINT('Ctrl Pts',(-50.,-5.61830723712665,9.14143059178176));
#45426=CARTESIAN_POINT('Ctrl Pts',(-66.,-5.67703542746581,9.20524426521879));
#45427=CARTESIAN_POINT('Ctrl Pts',(-50.,-5.67703542746581,9.20524426521879));
#45428=CARTESIAN_POINT('Ctrl Pts',(-66.,-5.78598690780261,9.21276610214511));
#45429=CARTESIAN_POINT('Ctrl Pts',(-50.,-5.78598690780261,9.21276610214511));
#45430=CARTESIAN_POINT('Ctrl Pts',(-66.,-5.95351398409578,9.1550652704948));
#45431=CARTESIAN_POINT('Ctrl Pts',(-50.,-5.95351398409578,9.1550652704948));
#45432=CARTESIAN_POINT('Ctrl Pts',(-66.,-6.1857832706813,9.0255586111413));
#45433=CARTESIAN_POINT('Ctrl Pts',(-50.,-6.1857832706813,9.0255586111413));
#45434=CARTESIAN_POINT('Ctrl Pts',(-66.,-6.4870891147678,8.81967227800013));
#45435=CARTESIAN_POINT('Ctrl Pts',(-50.,-6.4870891147678,8.81967227800013));
#45436=CARTESIAN_POINT('Ctrl Pts',(-66.,-6.86020750749309,8.5344601927968));
#45437=CARTESIAN_POINT('Ctrl Pts',(-50.,-6.86020750749309,8.5344601927968));
#45438=CARTESIAN_POINT('Ctrl Pts',(-66.,-7.30671529340422,8.16825989491623));
#45439=CARTESIAN_POINT('Ctrl Pts',(-50.,-7.30671529340422,8.16825989491623));
#45440=CARTESIAN_POINT('Ctrl Pts',(-66.,-7.8273085045771,7.72034951863681));
#45441=CARTESIAN_POINT('Ctrl Pts',(-50.,-7.8273085045771,7.72034951863681));
#45442=CARTESIAN_POINT('Ctrl Pts',(-66.,-8.30314715005506,7.2965657688752));
#45443=CARTESIAN_POINT('Ctrl Pts',(-50.,-8.30314715005506,7.2965657688752));
#45444=CARTESIAN_POINT('Ctrl Pts',(-66.,-8.69334695511751,6.9419914678159));
#45445=CARTESIAN_POINT('Ctrl Pts',(-50.,-8.69334695511751,6.9419914678159));
#45446=CARTESIAN_POINT('Ctrl Pts',(-66.,-8.96826972520416,6.68930297706156));
#45447=CARTESIAN_POINT('Ctrl Pts',(-50.,-8.96826972520416,6.68930297706156));
#45448=CARTESIAN_POINT('Ctrl Pts',(-66.,-9.10942850298702,6.55888232467755));
#45449=CARTESIAN_POINT('Ctrl Pts',(-50.,-9.10942850298702,6.55888232467755));
#45450=CARTESIAN_POINT('',(-65.5,-5.60521455261512,9.02619492472613));
#45451=CARTESIAN_POINT('Ctrl Pts',(-66.,-5.63989399158651,8.40875857446665));
#45452=CARTESIAN_POINT('Ctrl Pts',(-65.7982417703062,-5.64698827769721,
8.64693773448211));
#45453=CARTESIAN_POINT('Ctrl Pts',(-65.6331946192802,-5.59528609755734,
8.87557312667991));
#45454=CARTESIAN_POINT('Ctrl Pts',(-65.5,-5.60521455261512,9.02619492472612));
#45455=CARTESIAN_POINT('',(-50.,-4.66907432066881,6.26377691477523));
#45456=CARTESIAN_POINT('',(-66.,-4.66907432066881,6.26377691477523));
#45457=CARTESIAN_POINT('',(-50.,-5.63989399158651,8.40875857446667));
#45458=CARTESIAN_POINT('Ctrl Pts',(-50.,-4.66907432066881,6.26377691477523));
#45459=CARTESIAN_POINT('Ctrl Pts',(-50.,-4.68258736973401,6.28328945005467));
#45460=CARTESIAN_POINT('Ctrl Pts',(-50.,-4.70979548740211,6.32219595087909));
#45461=CARTESIAN_POINT('Ctrl Pts',(-50.,-4.75115374374443,6.3801999799666));
#45462=CARTESIAN_POINT('Ctrl Pts',(-50.,-4.80739151505302,6.45682640629315));
#45463=CARTESIAN_POINT('Ctrl Pts',(-50.,-4.87940339472638,6.55149182098506));
#45464=CARTESIAN_POINT('Ctrl Pts',(-50.,-4.95278821116117,6.645260114762));
#45465=CARTESIAN_POINT('Ctrl Pts',(-50.,-5.02685611555883,6.7385766957876));
#45466=CARTESIAN_POINT('Ctrl Pts',(-50.,-5.10042834492066,6.83220206842988));
#45467=CARTESIAN_POINT('Ctrl Pts',(-50.,-5.17200306149544,6.92712124167231));
#45468=CARTESIAN_POINT('Ctrl Pts',(-50.,-5.23995252537855,7.02443775083668));
#45469=CARTESIAN_POINT('Ctrl Pts',(-50.,-5.3027072062188,7.12526883629655));
#45470=CARTESIAN_POINT('Ctrl Pts',(-50.,-5.35894790191298,7.23065348642503));
#45471=CARTESIAN_POINT('Ctrl Pts',(-50.,-5.40780718177897,7.34132172472021));
#45472=CARTESIAN_POINT('Ctrl Pts',(-50.,-5.44911325868757,7.45738867431159));
#45473=CARTESIAN_POINT('Ctrl Pts',(-50.,-5.48355669348136,7.57814301204284));
#45474=CARTESIAN_POINT('Ctrl Pts',(-50.,-5.51305921086426,7.70161357993859));
#45475=CARTESIAN_POINT('Ctrl Pts',(-50.,-5.54016188969533,7.82519591791858));
#45476=CARTESIAN_POINT('Ctrl Pts',(-50.,-5.56683712169066,7.94689743821095));
#45477=CARTESIAN_POINT('Ctrl Pts',(-50.,-5.593664068609,8.06619581758504));
#45478=CARTESIAN_POINT('Ctrl Pts',(-50.,-5.61707418533788,8.17903563336739));
#45479=CARTESIAN_POINT('Ctrl Pts',(-50.,-5.63092023716983,8.27141516094588));
#45480=CARTESIAN_POINT('Ctrl Pts',(-50.,-5.63713657156084,8.34237187934735));
#45481=CARTESIAN_POINT('Ctrl Pts',(-50.,-5.63930183311986,8.3888778135301));
#45482=CARTESIAN_POINT('Ctrl Pts',(-50.,-5.63989399158651,8.40875857446667));
#45483=CARTESIAN_POINT('',(-50.5,-5.60521455261512,9.02619492472613));
#45484=CARTESIAN_POINT('Ctrl Pts',(-50.5,-5.60521455261512,9.02619492472614));
#45485=CARTESIAN_POINT('Ctrl Pts',(-50.4982567069803,-5.60508460587634,
9.02422353931612));
#45486=CARTESIAN_POINT('Ctrl Pts',(-50.4965113438768,-5.60496484245642,
9.02224324973366));
#45487=CARTESIAN_POINT('Ctrl Pts',(-50.3581212730784,-5.59625809416611,
8.86472332078281));
#45488=CARTESIAN_POINT('Ctrl Pts',(-50.2022201285465,-5.64700451912944,
8.64748301425043));
#45489=CARTESIAN_POINT('Ctrl Pts',(-50.,-5.63989399158651,8.40875857446667));
#45490=CARTESIAN_POINT('Ctrl Pts',(-65.5,-5.60521455261512,9.02619492472613));
#45491=CARTESIAN_POINT('Ctrl Pts',(-60.5,-5.60521455261512,9.02619492472613));
#45492=CARTESIAN_POINT('Ctrl Pts',(-55.5,-5.60521455261512,9.02619492472613));
#45493=CARTESIAN_POINT('Ctrl Pts',(-50.5,-5.60521455261512,9.02619492472613));
#45494=CARTESIAN_POINT('Origin',(-66.,0.,0.));
#45495=CARTESIAN_POINT('',(-50.,-5.74141212582432,5.29823961815974));
#45496=CARTESIAN_POINT('',(-66.,-5.74141212582432,5.29823961815974));
#45497=CARTESIAN_POINT('Origin',(-50.,0.,0.));
#45498=CARTESIAN_POINT('Ctrl Pts',(-66.,-9.10942850298702,6.55888232467755));
#45499=CARTESIAN_POINT('Ctrl Pts',(-50.,-9.10942850298702,6.55888232467755));
#45500=CARTESIAN_POINT('Ctrl Pts',(-66.,-9.08576143793161,6.55992054266089));
#45501=CARTESIAN_POINT('Ctrl Pts',(-50.,-9.08576143793161,6.55992054266089));
#45502=CARTESIAN_POINT('Ctrl Pts',(-66.,-9.03849534181953,6.56179460771868));
#45503=CARTESIAN_POINT('Ctrl Pts',(-50.,-9.03849534181953,6.56179460771868));
#45504=CARTESIAN_POINT('Ctrl Pts',(-66.,-8.96780029988517,6.56399859267612));
#45505=CARTESIAN_POINT('Ctrl Pts',(-50.,-8.96780029988517,6.56399859267612));
#45506=CARTESIAN_POINT('Ctrl Pts',(-66.,-8.87394898919059,6.56572139847731));
#45507=CARTESIAN_POINT('Ctrl Pts',(-50.,-8.87394898919059,6.56572139847731));
#45508=CARTESIAN_POINT('Ctrl Pts',(-66.,-8.75732214056418,6.56583717553711));
#45509=CARTESIAN_POINT('Ctrl Pts',(-50.,-8.75732214056418,6.56583717553711));
#45510=CARTESIAN_POINT('Ctrl Pts',(-66.,-8.64139521040441,6.56389753528232));
#45511=CARTESIAN_POINT('Ctrl Pts',(-50.,-8.64139521040441,6.56389753528232));
#45512=CARTESIAN_POINT('Ctrl Pts',(-66.,-8.5261893930021,6.55987949669048));
#45513=CARTESIAN_POINT('Ctrl Pts',(-50.,-8.5261893930021,6.55987949669048));
#45514=CARTESIAN_POINT('Ctrl Pts',(-66.,-8.41173611627071,6.55375602860952));
#45515=CARTESIAN_POINT('Ctrl Pts',(-50.,-8.41173611627071,6.55375602860952));
#45516=CARTESIAN_POINT('Ctrl Pts',(-66.,-8.29807942911973,6.54549737862328));
#45517=CARTESIAN_POINT('Ctrl Pts',(-50.,-8.29807942911973,6.54549737862328));
#45518=CARTESIAN_POINT('Ctrl Pts',(-66.,-8.18527357628522,6.53507290801895));
#45519=CARTESIAN_POINT('Ctrl Pts',(-50.,-8.18527357628522,6.53507290801895));
#45520=CARTESIAN_POINT('Ctrl Pts',(-66.,-8.07337944645762,6.52245299848617));
#45521=CARTESIAN_POINT('Ctrl Pts',(-50.,-8.07337944645762,6.52245299848617));
#45522=CARTESIAN_POINT('Ctrl Pts',(-66.,-7.96246113297438,6.50761151737996));
#45523=CARTESIAN_POINT('Ctrl Pts',(-50.,-7.96246113297438,6.50761151737996));
#45524=CARTESIAN_POINT('Ctrl Pts',(-66.,-7.85258285330582,6.49052756009744));
#45525=CARTESIAN_POINT('Ctrl Pts',(-50.,-7.85258285330582,6.49052756009744));
#45526=CARTESIAN_POINT('Ctrl Pts',(-66.,-7.74380437584162,6.47118971339301));
#45527=CARTESIAN_POINT('Ctrl Pts',(-50.,-7.74380437584162,6.47118971339301));
#45528=CARTESIAN_POINT('Ctrl Pts',(-66.,-7.63618323735142,6.44958986632227));
#45529=CARTESIAN_POINT('Ctrl Pts',(-50.,-7.63618323735142,6.44958986632227));
#45530=CARTESIAN_POINT('Ctrl Pts',(-66.,-7.52978062910616,6.42571181012752));
#45531=CARTESIAN_POINT('Ctrl Pts',(-50.,-7.52978062910616,6.42571181012752));
#45532=CARTESIAN_POINT('Ctrl Pts',(-66.,-7.42466575500371,6.39952147476842));
#45533=CARTESIAN_POINT('Ctrl Pts',(-50.,-7.42466575500371,6.39952147476842));
#45534=CARTESIAN_POINT('Ctrl Pts',(-66.,-7.3209213165869,6.37095713183339));
#45535=CARTESIAN_POINT('Ctrl Pts',(-50.,-7.3209213165869,6.37095713183339));
#45536=CARTESIAN_POINT('Ctrl Pts',(-66.,-7.21864696410326,6.33991858248025));
#45537=CARTESIAN_POINT('Ctrl Pts',(-50.,-7.21864696410326,6.33991858248025));
#45538=CARTESIAN_POINT('Ctrl Pts',(-66.,-7.11796972459708,6.30626252916358));
#45539=CARTESIAN_POINT('Ctrl Pts',(-50.,-7.11796972459708,6.30626252916358));
#45540=CARTESIAN_POINT('Ctrl Pts',(-66.,-7.01905715111184,6.26980372166142));
#45541=CARTESIAN_POINT('Ctrl Pts',(-50.,-7.01905715111184,6.26980372166142));
#45542=CARTESIAN_POINT('Ctrl Pts',(-66.,-6.92213264398368,6.23031211373657));
#45543=CARTESIAN_POINT('Ctrl Pts',(-50.,-6.92213264398368,6.23031211373657));
#45544=CARTESIAN_POINT('Ctrl Pts',(-66.,-6.82748343979352,6.18751687615083));
#45545=CARTESIAN_POINT('Ctrl Pts',(-50.,-6.82748343979352,6.18751687615083));
#45546=CARTESIAN_POINT('Ctrl Pts',(-66.,-6.73548810524172,6.14109480995689));
#45547=CARTESIAN_POINT('Ctrl Pts',(-50.,-6.73548810524172,6.14109480995689));
#45548=CARTESIAN_POINT('Ctrl Pts',(-66.,-6.64656015751461,6.09072492635055));
#45549=CARTESIAN_POINT('Ctrl Pts',(-50.,-6.64656015751461,6.09072492635055));
#45550=CARTESIAN_POINT('Ctrl Pts',(-66.,-6.56104388578368,6.03618002486629));
#45551=CARTESIAN_POINT('Ctrl Pts',(-50.,-6.56104388578368,6.03618002486629));
#45552=CARTESIAN_POINT('Ctrl Pts',(-66.,-6.47911851546308,5.97741330588777));
#45553=CARTESIAN_POINT('Ctrl Pts',(-50.,-6.47911851546308,5.97741330588777));
#45554=CARTESIAN_POINT('Ctrl Pts',(-66.,-6.4007102042632,5.91463628394544));
#45555=CARTESIAN_POINT('Ctrl Pts',(-50.,-6.4007102042632,5.91463628394544));
#45556=CARTESIAN_POINT('Ctrl Pts',(-66.,-6.32536729565295,5.8484330883917));
#45557=CARTESIAN_POINT('Ctrl Pts',(-50.,-6.32536729565295,5.8484330883917));
#45558=CARTESIAN_POINT('Ctrl Pts',(-66.,-6.25233913230877,5.77967659171849));
#45559=CARTESIAN_POINT('Ctrl Pts',(-50.,-6.25233913230877,5.77967659171849));
#45560=CARTESIAN_POINT('Ctrl Pts',(-66.,-6.18072779481142,5.70937384347389));
#45561=CARTESIAN_POINT('Ctrl Pts',(-50.,-6.18072779481142,5.70937384347389));
#45562=CARTESIAN_POINT('Ctrl Pts',(-66.,-6.10961745579836,5.63853298297221));
#45563=CARTESIAN_POINT('Ctrl Pts',(-50.,-6.10961745579836,5.63853298297221));
#45564=CARTESIAN_POINT('Ctrl Pts',(-66.,-6.03820626716823,5.56802821638893));
#45565=CARTESIAN_POINT('Ctrl Pts',(-50.,-6.03820626716823,5.56802821638893));
#45566=CARTESIAN_POINT('Ctrl Pts',(-66.,-5.96595410170651,5.49844782238954));
#45567=CARTESIAN_POINT('Ctrl Pts',(-50.,-5.96595410170651,5.49844782238954));
#45568=CARTESIAN_POINT('Ctrl Pts',(-66.,-5.89254591434388,5.43013507033993));
#45569=CARTESIAN_POINT('Ctrl Pts',(-50.,-5.89254591434388,5.43013507033993));
#45570=CARTESIAN_POINT('Ctrl Pts',(-66.,-5.8327710073448,5.37663351860743));
#45571=CARTESIAN_POINT('Ctrl Pts',(-50.,-5.8327710073448,5.37663351860743));
#45572=CARTESIAN_POINT('Ctrl Pts',(-66.,-5.78732886917933,5.33717661990139));
#45573=CARTESIAN_POINT('Ctrl Pts',(-50.,-5.78732886917933,5.33717661990139));
#45574=CARTESIAN_POINT('Ctrl Pts',(-66.,-5.75676290651676,5.31116910570307));
#45575=CARTESIAN_POINT('Ctrl Pts',(-50.,-5.75676290651676,5.31116910570307));
#45576=CARTESIAN_POINT('Ctrl Pts',(-66.,-5.74141212582432,5.29823961815974));
#45577=CARTESIAN_POINT('Ctrl Pts',(-50.,-5.74141212582432,5.29823961815974));
#45578=CARTESIAN_POINT('Ctrl Pts',(-50.,-7.78178935653717,6.47760599376692));
#45579=CARTESIAN_POINT('Ctrl Pts',(-50.,-7.77423639474705,6.47623696517724));
#45580=CARTESIAN_POINT('Ctrl Pts',(-50.,-7.74499129323442,6.47087829659421));
#45581=CARTESIAN_POINT('Ctrl Pts',(-50.,-7.69422820821259,6.46118598421581));
#45582=CARTESIAN_POINT('Ctrl Pts',(-50.,-7.62230326232111,6.44647502892099));
#45583=CARTESIAN_POINT('Ctrl Pts',(-50.,-7.52978062910616,6.42571181012752));
#45584=CARTESIAN_POINT('Ctrl Pts',(-50.,-7.42466575500371,6.39952147476842));
#45585=CARTESIAN_POINT('Ctrl Pts',(-50.,-7.3209213165869,6.37095713183339));
#45586=CARTESIAN_POINT('Ctrl Pts',(-50.,-7.21864696410326,6.33991858248025));
#45587=CARTESIAN_POINT('Ctrl Pts',(-50.,-7.11796972459708,6.30626252916358));
#45588=CARTESIAN_POINT('Ctrl Pts',(-50.,-7.01905715111184,6.26980372166142));
#45589=CARTESIAN_POINT('Ctrl Pts',(-50.,-6.92213264398368,6.23031211373657));
#45590=CARTESIAN_POINT('Ctrl Pts',(-50.,-6.82748343979352,6.18751687615083));
#45591=CARTESIAN_POINT('Ctrl Pts',(-50.,-6.73548810524172,6.14109480995689));
#45592=CARTESIAN_POINT('Ctrl Pts',(-50.,-6.64656015751461,6.09072492635055));
#45593=CARTESIAN_POINT('Ctrl Pts',(-50.,-6.56104388578368,6.03618002486629));
#45594=CARTESIAN_POINT('Ctrl Pts',(-50.,-6.47911851546308,5.97741330588777));
#45595=CARTESIAN_POINT('Ctrl Pts',(-50.,-6.4007102042632,5.91463628394544));
#45596=CARTESIAN_POINT('Ctrl Pts',(-50.,-6.32536729565295,5.8484330883917));
#45597=CARTESIAN_POINT('Ctrl Pts',(-50.,-6.25233913230877,5.77967659171849));
#45598=CARTESIAN_POINT('Ctrl Pts',(-50.,-6.18072779481142,5.70937384347389));
#45599=CARTESIAN_POINT('Ctrl Pts',(-50.,-6.10961745579836,5.63853298297221));
#45600=CARTESIAN_POINT('Ctrl Pts',(-50.,-6.03820626716823,5.56802821638893));
#45601=CARTESIAN_POINT('Ctrl Pts',(-50.,-5.96595410170651,5.49844782238954));
#45602=CARTESIAN_POINT('Ctrl Pts',(-50.,-5.89254591434388,5.43013507033993));
#45603=CARTESIAN_POINT('Ctrl Pts',(-50.,-5.8327710073448,5.37663351860743));
#45604=CARTESIAN_POINT('Ctrl Pts',(-50.,-5.78732886917933,5.33717661990139));
#45605=CARTESIAN_POINT('Ctrl Pts',(-50.,-5.75676290651676,5.31116910570307));
#45606=CARTESIAN_POINT('Ctrl Pts',(-50.,-5.74141212582432,5.29823961815974));
#45607=CARTESIAN_POINT('Origin',(-50.,-6.71577615516547,6.72762868007336));
#45608=CARTESIAN_POINT('Origin',(-50.,0.,0.));
#45609=CARTESIAN_POINT('Origin',(-65.75,0.,0.));
#45610=CARTESIAN_POINT('',(-65.5,-4.97834853060433,9.38651537621016));
#45611=CARTESIAN_POINT('Origin',(-65.5,0.,0.));
#45612=CARTESIAN_POINT('',(-66.,-4.47433860192361,9.08272641200517));
#45613=CARTESIAN_POINT('Ctrl Pts',(-65.5,-4.97834853060432,9.38651537621016));
#45614=CARTESIAN_POINT('Ctrl Pts',(-65.664291736,-4.80345165052451,9.29330697735479));
#45615=CARTESIAN_POINT('Ctrl Pts',(-65.831118235484,-4.63468361464914,9.19199866580212));
#45616=CARTESIAN_POINT('Ctrl Pts',(-66.,-4.47433860192361,9.08272641200516));
#45617=CARTESIAN_POINT('Origin',(-66.,0.,0.));
#45618=CARTESIAN_POINT('Origin',(-58.,0.,0.));
#45619=CARTESIAN_POINT('',(-50.5,-4.97834853060433,9.38651537621016));
#45620=CARTESIAN_POINT('Origin',(-50.5,0.,0.));
#45621=CARTESIAN_POINT('Ctrl Pts',(-50.5,-4.97834853060433,9.38651537621016));
#45622=CARTESIAN_POINT('Ctrl Pts',(-55.5,-4.97834853060433,9.38651537621016));
#45623=CARTESIAN_POINT('Ctrl Pts',(-60.5,-4.97834853060433,9.38651537621016));
#45624=CARTESIAN_POINT('Ctrl Pts',(-65.5,-4.97834853060433,9.38651537621016));
#45625=CARTESIAN_POINT('Origin',(-50.25,0.,0.));
#45626=CARTESIAN_POINT('',(-50.,-4.47433860192363,9.08272641200518));
#45627=CARTESIAN_POINT('Origin',(-50.,0.,0.));
#45628=CARTESIAN_POINT('Ctrl Pts',(-50.,-4.47433860192363,9.08272641200517));
#45629=CARTESIAN_POINT('Ctrl Pts',(-50.1688817645162,-4.6346836146493,9.19199866580223));
#45630=CARTESIAN_POINT('Ctrl Pts',(-50.3357082640001,-4.80345165052468,
9.29330697735489));
#45631=CARTESIAN_POINT('Ctrl Pts',(-50.5,-4.97834853060434,9.38651537621016));
#45632=CARTESIAN_POINT('Origin',(-66.,-3.39879369590239,8.87754687038761));
#45633=CARTESIAN_POINT('',(-66.,-1.73214930258623,9.97573474955855));
#45634=CARTESIAN_POINT('Origin',(-66.,0.,0.));
#45635=CARTESIAN_POINT('',(-66.,-3.09005277149945,7.17542543124438));
#45636=CARTESIAN_POINT('Ctrl Pts',(-66.,-3.09005277149946,7.17542543124437));
#45637=CARTESIAN_POINT('Ctrl Pts',(-66.,-3.09881751111224,7.19348083086667));
#45638=CARTESIAN_POINT('Ctrl Pts',(-66.,-3.11616269844133,7.22967217437288));
#45639=CARTESIAN_POINT('Ctrl Pts',(-66.,-3.14162759082209,7.28420082769005));
#45640=CARTESIAN_POINT('Ctrl Pts',(-66.,-3.17447364404108,7.35738957226508));
#45641=CARTESIAN_POINT('Ctrl Pts',(-66.,-3.21375006071206,7.44965417630122));
#45642=CARTESIAN_POINT('Ctrl Pts',(-66.,-3.25145480239525,7.5426066324152));
#45643=CARTESIAN_POINT('Ctrl Pts',(-66.,-3.28801529731225,7.63606148881098));
#45644=CARTESIAN_POINT('Ctrl Pts',(-66.,-3.32416425071599,7.72970101571594));
#45645=CARTESIAN_POINT('Ctrl Pts',(-66.,-3.3609897589824,7.82305272705443));
#45646=CARTESIAN_POINT('Ctrl Pts',(-66.,-3.39973851923894,7.91556814228226));
#45647=CARTESIAN_POINT('Ctrl Pts',(-66.,-3.441640425645,8.00669249258951));
#45648=CARTESIAN_POINT('Ctrl Pts',(-66.,-3.48773626701595,8.09593368911593));
#45649=CARTESIAN_POINT('Ctrl Pts',(-66.,-3.53867623893612,8.18294180840626));
#45650=CARTESIAN_POINT('Ctrl Pts',(-66.,-3.59461383040384,8.26755365668696));
#45651=CARTESIAN_POINT('Ctrl Pts',(-66.,-3.65536627573726,8.34973908999167));
#45652=CARTESIAN_POINT('Ctrl Pts',(-66.,-3.720526640373,8.42956563125176));
#45653=CARTESIAN_POINT('Ctrl Pts',(-66.,-3.78958659965516,8.50715832573905));
#45654=CARTESIAN_POINT('Ctrl Pts',(-66.,-3.86206885883931,8.58265845343488));
#45655=CARTESIAN_POINT('Ctrl Pts',(-66.,-3.93760085807652,8.65619659951692));
#45656=CARTESIAN_POINT('Ctrl Pts',(-66.,-4.01588494277018,8.72789205657743));
#45657=CARTESIAN_POINT('Ctrl Pts',(-66.,-4.09669269754511,8.79784590915275));
#45658=CARTESIAN_POINT('Ctrl Pts',(-66.,-4.17984979305941,8.86613739951103));
#45659=CARTESIAN_POINT('Ctrl Pts',(-66.,-4.26522443974139,8.93281753244224));
#45660=CARTESIAN_POINT('Ctrl Pts',(-66.,-4.34130290913253,8.98941802189943));
#45661=CARTESIAN_POINT('Ctrl Pts',(-66.,-4.40102613216983,9.03211165933191));
#45662=CARTESIAN_POINT('Ctrl Pts',(-66.,-4.443458299307,9.06161323407319));
#45663=CARTESIAN_POINT('Ctrl Pts',(-66.,-4.46799546208135,9.07840367583189));
#45664=CARTESIAN_POINT('Ctrl Pts',(-66.,-4.47433860192361,9.08272641200517));
#45665=CARTESIAN_POINT('',(-66.,-1.71770404175133,7.62132856363975));
#45666=CARTESIAN_POINT('Origin',(-66.,0.,0.));
#45667=CARTESIAN_POINT('Ctrl Pts',(-66.,-1.73214930258623,9.97573474955855));
#45668=CARTESIAN_POINT('Ctrl Pts',(-66.,-1.73969457287395,9.95733191816358));
#45669=CARTESIAN_POINT('Ctrl Pts',(-66.,-1.7566321755647,9.9139659420196));
#45670=CARTESIAN_POINT('Ctrl Pts',(-66.,-1.77981396896489,9.84661534325229));
#45671=CARTESIAN_POINT('Ctrl Pts',(-66.,-1.80473911014373,9.75659074881182));
#45672=CARTESIAN_POINT('Ctrl Pts',(-66.,-1.82924899221979,9.6439846953703));
#45673=CARTESIAN_POINT('Ctrl Pts',(-66.,-1.85326437907112,9.52408870045544));
#45674=CARTESIAN_POINT('Ctrl Pts',(-66.,-1.87839580987116,9.40205903508911));
#45675=CARTESIAN_POINT('Ctrl Pts',(-66.,-1.90390174602853,9.27813729897652));
#45676=CARTESIAN_POINT('Ctrl Pts',(-66.,-1.92716985958894,9.15334156764019));
#45677=CARTESIAN_POINT('Ctrl Pts',(-66.,-1.94481943015312,9.02901758387114));
#45678=CARTESIAN_POINT('Ctrl Pts',(-66.,-1.95429313266907,8.90618445422908));
#45679=CARTESIAN_POINT('Ctrl Pts',(-66.,-1.9546707872231,8.78521112835341));
#45680=CARTESIAN_POINT('Ctrl Pts',(-66.,-1.946156153962,8.66606230815238));
#45681=CARTESIAN_POINT('Ctrl Pts',(-66.,-1.92983859755222,8.54842389981909));
#45682=CARTESIAN_POINT('Ctrl Pts',(-66.,-1.90734586372592,8.43188330807973));
#45683=CARTESIAN_POINT('Ctrl Pts',(-66.,-1.88056621240513,8.31605826857219));
#45684=CARTESIAN_POINT('Ctrl Pts',(-66.,-1.85143550623823,8.20060271308051));
#45685=CARTESIAN_POINT('Ctrl Pts',(-66.,-1.82172638152831,8.08522764356747));
#45686=CARTESIAN_POINT('Ctrl Pts',(-66.,-1.79282501685215,7.96971775082723));
#45687=CARTESIAN_POINT('Ctrl Pts',(-66.,-1.76554278426741,7.85394672103966));
#45688=CARTESIAN_POINT('Ctrl Pts',(-66.,-1.74533379915545,7.76107103501753));
#45689=CARTESIAN_POINT('Ctrl Pts',(-66.,-1.73114351601384,7.69125979937153));
#45690=CARTESIAN_POINT('Ctrl Pts',(-66.,-1.72211236324629,7.64465040382587));
#45691=CARTESIAN_POINT('Ctrl Pts',(-66.,-1.71770404175133,7.62132856363975));
#45692=CARTESIAN_POINT('Ctrl Pts',(-66.,-1.71770404175133,7.62132856363975));
#45693=CARTESIAN_POINT('Ctrl Pts',(-50.,-1.71770404175133,7.62132856363975));
#45694=CARTESIAN_POINT('Ctrl Pts',(-66.,-1.72211236324629,7.64465040382587));
#45695=CARTESIAN_POINT('Ctrl Pts',(-50.,-1.72211236324629,7.64465040382587));
#45696=CARTESIAN_POINT('Ctrl Pts',(-66.,-1.73114351601384,7.69125979937153));
#45697=CARTESIAN_POINT('Ctrl Pts',(-50.,-1.73114351601384,7.69125979937153));
#45698=CARTESIAN_POINT('Ctrl Pts',(-66.,-1.74533379915545,7.76107103501753));
#45699=CARTESIAN_POINT('Ctrl Pts',(-50.,-1.74533379915545,7.76107103501753));
#45700=CARTESIAN_POINT('Ctrl Pts',(-66.,-1.76554278426741,7.85394672103966));
#45701=CARTESIAN_POINT('Ctrl Pts',(-50.,-1.76554278426741,7.85394672103966));
#45702=CARTESIAN_POINT('Ctrl Pts',(-66.,-1.79282501685215,7.96971775082723));
#45703=CARTESIAN_POINT('Ctrl Pts',(-50.,-1.79282501685215,7.96971775082723));
#45704=CARTESIAN_POINT('Ctrl Pts',(-66.,-1.82172638152831,8.08522764356747));
#45705=CARTESIAN_POINT('Ctrl Pts',(-50.,-1.82172638152831,8.08522764356747));
#45706=CARTESIAN_POINT('Ctrl Pts',(-66.,-1.85143550623823,8.20060271308051));
#45707=CARTESIAN_POINT('Ctrl Pts',(-50.,-1.85143550623823,8.20060271308051));
#45708=CARTESIAN_POINT('Ctrl Pts',(-66.,-1.88056621240513,8.31605826857219));
#45709=CARTESIAN_POINT('Ctrl Pts',(-50.,-1.88056621240513,8.31605826857219));
#45710=CARTESIAN_POINT('Ctrl Pts',(-66.,-1.90734586372592,8.43188330807973));
#45711=CARTESIAN_POINT('Ctrl Pts',(-50.,-1.90734586372592,8.43188330807973));
#45712=CARTESIAN_POINT('Ctrl Pts',(-66.,-1.92983859755222,8.54842389981909));
#45713=CARTESIAN_POINT('Ctrl Pts',(-50.,-1.92983859755222,8.54842389981909));
#45714=CARTESIAN_POINT('Ctrl Pts',(-66.,-1.946156153962,8.66606230815238));
#45715=CARTESIAN_POINT('Ctrl Pts',(-50.,-1.946156153962,8.66606230815238));
#45716=CARTESIAN_POINT('Ctrl Pts',(-66.,-1.9546707872231,8.78521112835341));
#45717=CARTESIAN_POINT('Ctrl Pts',(-50.,-1.9546707872231,8.78521112835341));
#45718=CARTESIAN_POINT('Ctrl Pts',(-66.,-1.95429313266907,8.90618445422908));
#45719=CARTESIAN_POINT('Ctrl Pts',(-50.,-1.95429313266907,8.90618445422908));
#45720=CARTESIAN_POINT('Ctrl Pts',(-66.,-1.94481943015312,9.02901758387114));
#45721=CARTESIAN_POINT('Ctrl Pts',(-50.,-1.94481943015312,9.02901758387114));
#45722=CARTESIAN_POINT('Ctrl Pts',(-66.,-1.92716985958894,9.15334156764019));
#45723=CARTESIAN_POINT('Ctrl Pts',(-50.,-1.92716985958894,9.15334156764019));
#45724=CARTESIAN_POINT('Ctrl Pts',(-66.,-1.90390174602853,9.27813729897652));
#45725=CARTESIAN_POINT('Ctrl Pts',(-50.,-1.90390174602853,9.27813729897652));
#45726=CARTESIAN_POINT('Ctrl Pts',(-66.,-1.87839580987116,9.40205903508911));
#45727=CARTESIAN_POINT('Ctrl Pts',(-50.,-1.87839580987116,9.40205903508911));
#45728=CARTESIAN_POINT('Ctrl Pts',(-66.,-1.85326437907112,9.52408870045544));
#45729=CARTESIAN_POINT('Ctrl Pts',(-50.,-1.85326437907112,9.52408870045544));
#45730=CARTESIAN_POINT('Ctrl Pts',(-66.,-1.82924899221979,9.6439846953703));
#45731=CARTESIAN_POINT('Ctrl Pts',(-50.,-1.82924899221979,9.6439846953703));
#45732=CARTESIAN_POINT('Ctrl Pts',(-66.,-1.8033312375021,9.76305895544906));
#45733=CARTESIAN_POINT('Ctrl Pts',(-50.,-1.8033312375021,9.76305895544906));
#45734=CARTESIAN_POINT('Ctrl Pts',(-66.,-1.76935818428543,9.88390776205071));
#45735=CARTESIAN_POINT('Ctrl Pts',(-50.,-1.76935818428543,9.88390776205071));
#45736=CARTESIAN_POINT('Ctrl Pts',(-66.,-1.72158810581393,10.0089274070765));
#45737=CARTESIAN_POINT('Ctrl Pts',(-50.,-1.72158810581393,10.0089274070765));
#45738=CARTESIAN_POINT('Ctrl Pts',(-66.,-1.65730460746568,10.1392183674146));
#45739=CARTESIAN_POINT('Ctrl Pts',(-50.,-1.65730460746568,10.1392183674146));
#45740=CARTESIAN_POINT('Ctrl Pts',(-66.,-1.58020220545128,10.2731661881148));
#45741=CARTESIAN_POINT('Ctrl Pts',(-50.,-1.58020220545128,10.2731661881148));
#45742=CARTESIAN_POINT('Ctrl Pts',(-66.,-1.5023358317684,10.4056266289389));
#45743=CARTESIAN_POINT('Ctrl Pts',(-50.,-1.5023358317684,10.4056266289389));
#45744=CARTESIAN_POINT('Ctrl Pts',(-66.,-1.44067870129829,10.5293819191661));
#45745=CARTESIAN_POINT('Ctrl Pts',(-50.,-1.44067870129829,10.5293819191661));
#45746=CARTESIAN_POINT('Ctrl Pts',(-66.,-1.41442426430587,10.6362838188747));
#45747=CARTESIAN_POINT('Ctrl Pts',(-50.,-1.41442426430587,10.6362838188747));
#45748=CARTESIAN_POINT('Ctrl Pts',(-66.,-1.44211977650966,10.7184674173711));
#45749=CARTESIAN_POINT('Ctrl Pts',(-50.,-1.44211977650966,10.7184674173711));
#45750=CARTESIAN_POINT('Ctrl Pts',(-66.,-1.53859249977361,10.7696535166986));
#45751=CARTESIAN_POINT('Ctrl Pts',(-50.,-1.53859249977361,10.7696535166986));
#45752=CARTESIAN_POINT('Ctrl Pts',(-66.,-1.71510514192151,10.785080584678));
#45753=CARTESIAN_POINT('Ctrl Pts',(-50.,-1.71510514192151,10.785080584678));
#45754=CARTESIAN_POINT('Ctrl Pts',(-66.,-1.979968797513,10.7612427942066));
#45755=CARTESIAN_POINT('Ctrl Pts',(-50.,-1.979968797513,10.7612427942066));
#45756=CARTESIAN_POINT('Ctrl Pts',(-66.,-2.33896689873642,10.6957083973376));
#45757=CARTESIAN_POINT('Ctrl Pts',(-50.,-2.33896689873642,10.6957083973376));
#45758=CARTESIAN_POINT('Ctrl Pts',(-66.,-2.79583371767377,10.5869151149623));
#45759=CARTESIAN_POINT('Ctrl Pts',(-50.,-2.79583371767377,10.5869151149623));
#45760=CARTESIAN_POINT('Ctrl Pts',(-66.,-3.35268595714823,10.4339855741948));
#45761=CARTESIAN_POINT('Ctrl Pts',(-50.,-3.35268595714823,10.4339855741948));
#45762=CARTESIAN_POINT('Ctrl Pts',(-66.,-4.0104530833415,10.2365434196342));
#45763=CARTESIAN_POINT('Ctrl Pts',(-50.,-4.0104530833415,10.2365434196342));
#45764=CARTESIAN_POINT('Ctrl Pts',(-66.,-4.61752169625681,10.0429387133242));
#45765=CARTESIAN_POINT('Ctrl Pts',(-50.,-4.61752169625681,10.0429387133242));
#45766=CARTESIAN_POINT('Ctrl Pts',(-66.,-5.11820531667845,9.87772753003463));
#45767=CARTESIAN_POINT('Ctrl Pts',(-50.,-5.11820531667845,9.87772753003463));
#45768=CARTESIAN_POINT('Ctrl Pts',(-66.,-5.47213743296694,9.75870627171758));
#45769=CARTESIAN_POINT('Ctrl Pts',(-50.,-5.47213743296694,9.75870627171758));
#45770=CARTESIAN_POINT('Ctrl Pts',(-66.,-5.65413925155529,9.69697552456547));
#45771=CARTESIAN_POINT('Ctrl Pts',(-50.,-5.65413925155529,9.69697552456547));
#45772=CARTESIAN_POINT('',(-65.5,-1.44933407022281,10.5256855241305));
#45773=CARTESIAN_POINT('Ctrl Pts',(-66.,-1.73214930258624,9.97573474955854));
#45774=CARTESIAN_POINT('Ctrl Pts',(-65.798241770306,-1.64175406344253,10.1962077454137));
#45775=CARTESIAN_POINT('Ctrl Pts',(-65.6331946192802,-1.50152737971468,
10.3840473982224));
#45776=CARTESIAN_POINT('Ctrl Pts',(-65.5,-1.44933407022282,10.5256855241305));
#45777=CARTESIAN_POINT('',(-50.,-1.71770404175133,7.62132856363975));
#45778=CARTESIAN_POINT('',(-66.,-1.71770404175133,7.62132856363975));
#45779=CARTESIAN_POINT('',(-50.,-1.73214930258623,9.97573474955857));
#45780=CARTESIAN_POINT('Ctrl Pts',(-50.,-1.71770404175133,7.62132856363975));
#45781=CARTESIAN_POINT('Ctrl Pts',(-50.,-1.72211236324629,7.64465040382587));
#45782=CARTESIAN_POINT('Ctrl Pts',(-50.,-1.73114351601384,7.69125979937153));
#45783=CARTESIAN_POINT('Ctrl Pts',(-50.,-1.74533379915545,7.76107103501753));
#45784=CARTESIAN_POINT('Ctrl Pts',(-50.,-1.76554278426741,7.85394672103966));
#45785=CARTESIAN_POINT('Ctrl Pts',(-50.,-1.79282501685215,7.96971775082723));
#45786=CARTESIAN_POINT('Ctrl Pts',(-50.,-1.82172638152831,8.08522764356747));
#45787=CARTESIAN_POINT('Ctrl Pts',(-50.,-1.85143550623823,8.20060271308051));
#45788=CARTESIAN_POINT('Ctrl Pts',(-50.,-1.88056621240513,8.31605826857219));
#45789=CARTESIAN_POINT('Ctrl Pts',(-50.,-1.90734586372592,8.43188330807973));
#45790=CARTESIAN_POINT('Ctrl Pts',(-50.,-1.92983859755222,8.54842389981909));
#45791=CARTESIAN_POINT('Ctrl Pts',(-50.,-1.946156153962,8.66606230815238));
#45792=CARTESIAN_POINT('Ctrl Pts',(-50.,-1.9546707872231,8.78521112835341));
#45793=CARTESIAN_POINT('Ctrl Pts',(-50.,-1.95429313266907,8.90618445422908));
#45794=CARTESIAN_POINT('Ctrl Pts',(-50.,-1.94481943015312,9.02901758387114));
#45795=CARTESIAN_POINT('Ctrl Pts',(-50.,-1.92716985958894,9.15334156764019));
#45796=CARTESIAN_POINT('Ctrl Pts',(-50.,-1.90390174602853,9.27813729897652));
#45797=CARTESIAN_POINT('Ctrl Pts',(-50.,-1.87839580987116,9.40205903508911));
#45798=CARTESIAN_POINT('Ctrl Pts',(-50.,-1.85326437907112,9.52408870045544));
#45799=CARTESIAN_POINT('Ctrl Pts',(-50.,-1.82924899221979,9.6439846953703));
#45800=CARTESIAN_POINT('Ctrl Pts',(-50.,-1.80473911014373,9.75659074881182));
#45801=CARTESIAN_POINT('Ctrl Pts',(-50.,-1.77981396896489,9.84661534325229));
#45802=CARTESIAN_POINT('Ctrl Pts',(-50.,-1.7566321755647,9.91396594201961));
#45803=CARTESIAN_POINT('Ctrl Pts',(-50.,-1.73969457287395,9.95733191816359));
#45804=CARTESIAN_POINT('Ctrl Pts',(-50.,-1.73214930258623,9.97573474955856));
#45805=CARTESIAN_POINT('',(-50.5,-1.44933407022281,10.5256855241305));
#45806=CARTESIAN_POINT('Ctrl Pts',(-50.5,-1.44933407022281,10.5256855241306));
#45807=CARTESIAN_POINT('Ctrl Pts',(-50.4982567069801,-1.45001719265382,
10.5238317198435));
#45808=CARTESIAN_POINT('Ctrl Pts',(-50.4965113438764,-1.45071323966274,
10.521973923119));
#45809=CARTESIAN_POINT('Ctrl Pts',(-50.3581212730779,-1.50682835643054,
10.3745309539659));
#45810=CARTESIAN_POINT('Ctrl Pts',(-50.2022201285462,-1.64154711546685,
10.1967124892543));
#45811=CARTESIAN_POINT('Ctrl Pts',(-50.,-1.73214930258623,9.97573474955857));
#45812=CARTESIAN_POINT('Ctrl Pts',(-65.5,-1.44933407022281,10.5256855241305));
#45813=CARTESIAN_POINT('Ctrl Pts',(-60.5,-1.44933407022281,10.5256855241305));
#45814=CARTESIAN_POINT('Ctrl Pts',(-55.5,-1.44933407022281,10.5256855241305));
#45815=CARTESIAN_POINT('Ctrl Pts',(-50.5,-1.44933407022281,10.5256855241305));
#45816=CARTESIAN_POINT('Origin',(-66.,0.,0.));
#45817=CARTESIAN_POINT('',(-50.,-3.09005277149945,7.17542543124438));
#45818=CARTESIAN_POINT('',(-66.,-3.09005277149945,7.17542543124438));
#45819=CARTESIAN_POINT('Origin',(-50.,0.,0.));
#45820=CARTESIAN_POINT('Ctrl Pts',(-66.,-5.65413925155529,9.69697552456547));
#45821=CARTESIAN_POINT('Ctrl Pts',(-50.,-5.65413925155529,9.69697552456547));
#45822=CARTESIAN_POINT('Ctrl Pts',(-66.,-5.63209603048086,9.68829772129611));
#45823=CARTESIAN_POINT('Ctrl Pts',(-50.,-5.63209603048086,9.68829772129611));
#45824=CARTESIAN_POINT('Ctrl Pts',(-66.,-5.58815405214666,9.67078491165305));
#45825=CARTESIAN_POINT('Ctrl Pts',(-50.,-5.58815405214666,9.67078491165305));
#45826=CARTESIAN_POINT('Ctrl Pts',(-66.,-5.5226744762667,9.64404408806114));
#45827=CARTESIAN_POINT('Ctrl Pts',(-50.,-5.5226744762667,9.64404408806114));
#45828=CARTESIAN_POINT('Ctrl Pts',(-66.,-5.4362363094396,9.60744518241504));
#45829=CARTESIAN_POINT('Ctrl Pts',(-50.,-5.4362363094396,9.60744518241504));
#45830=CARTESIAN_POINT('Ctrl Pts',(-66.,-5.32964529086513,9.56011453711931));
#45831=CARTESIAN_POINT('Ctrl Pts',(-50.,-5.32964529086513,9.56011453711931));
#45832=CARTESIAN_POINT('Ctrl Pts',(-66.,-5.22452969316523,9.51119085715981));
#45833=CARTESIAN_POINT('Ctrl Pts',(-50.,-5.22452969316523,9.51119085715981));
#45834=CARTESIAN_POINT('Ctrl Pts',(-66.,-5.12091822551194,9.46066176882258));
#45835=CARTESIAN_POINT('Ctrl Pts',(-50.,-5.12091822551194,9.46066176882258));
#45836=CARTESIAN_POINT('Ctrl Pts',(-66.,-5.01885059329289,9.40851536080546));
#45837=CARTESIAN_POINT('Ctrl Pts',(-50.,-5.01885059329289,9.40851536080546));
#45838=CARTESIAN_POINT('Ctrl Pts',(-66.,-4.91837913858716,9.35474236922936));
#45839=CARTESIAN_POINT('Ctrl Pts',(-50.,-4.91837913858716,9.35474236922936));
#45840=CARTESIAN_POINT('Ctrl Pts',(-66.,-4.81956587831414,9.29933686755924));
#45841=CARTESIAN_POINT('Ctrl Pts',(-50.,-4.81956587831414,9.29933686755924));
#45842=CARTESIAN_POINT('Ctrl Pts',(-66.,-4.72247848391254,9.24229656378374));
#45843=CARTESIAN_POINT('Ctrl Pts',(-50.,-4.72247848391254,9.24229656378374));
#45844=CARTESIAN_POINT('Ctrl Pts',(-66.,-4.62718613666396,9.18362365365267));
#45845=CARTESIAN_POINT('Ctrl Pts',(-50.,-4.62718613666396,9.18362365365267));
#45846=CARTESIAN_POINT('Ctrl Pts',(-66.,-4.53375600481471,9.12332515945933));
#45847=CARTESIAN_POINT('Ctrl Pts',(-50.,-4.53375600481471,9.12332515945933));
#45848=CARTESIAN_POINT('Ctrl Pts',(-66.,-4.44224733169088,9.06141496467922));
#45849=CARTESIAN_POINT('Ctrl Pts',(-50.,-4.44224733169088,9.06141496467922));
#45850=CARTESIAN_POINT('Ctrl Pts',(-66.,-4.35271597876535,8.99790906190847));
#45851=CARTESIAN_POINT('Ctrl Pts',(-50.,-4.35271597876535,8.99790906190847));
#45852=CARTESIAN_POINT('Ctrl Pts',(-66.,-4.26522443974139,8.93281753244224));
#45853=CARTESIAN_POINT('Ctrl Pts',(-50.,-4.26522443974139,8.93281753244224));
#45854=CARTESIAN_POINT('Ctrl Pts',(-66.,-4.17984979305941,8.86613739951103));
#45855=CARTESIAN_POINT('Ctrl Pts',(-50.,-4.17984979305941,8.86613739951103));
#45856=CARTESIAN_POINT('Ctrl Pts',(-66.,-4.09669269754511,8.79784590915275));
#45857=CARTESIAN_POINT('Ctrl Pts',(-50.,-4.09669269754511,8.79784590915275));
#45858=CARTESIAN_POINT('Ctrl Pts',(-66.,-4.01588494277018,8.72789205657743));
#45859=CARTESIAN_POINT('Ctrl Pts',(-50.,-4.01588494277018,8.72789205657743));
#45860=CARTESIAN_POINT('Ctrl Pts',(-66.,-3.93760085807652,8.65619659951692));
#45861=CARTESIAN_POINT('Ctrl Pts',(-50.,-3.93760085807652,8.65619659951692));
#45862=CARTESIAN_POINT('Ctrl Pts',(-66.,-3.86206885883931,8.58265845343488));
#45863=CARTESIAN_POINT('Ctrl Pts',(-50.,-3.86206885883931,8.58265845343488));
#45864=CARTESIAN_POINT('Ctrl Pts',(-66.,-3.78958659965516,8.50715832573905));
#45865=CARTESIAN_POINT('Ctrl Pts',(-50.,-3.78958659965516,8.50715832573905));
#45866=CARTESIAN_POINT('Ctrl Pts',(-66.,-3.720526640373,8.42956563125176));
#45867=CARTESIAN_POINT('Ctrl Pts',(-50.,-3.720526640373,8.42956563125176));
#45868=CARTESIAN_POINT('Ctrl Pts',(-66.,-3.65536627573726,8.34973908999167));
#45869=CARTESIAN_POINT('Ctrl Pts',(-50.,-3.65536627573726,8.34973908999167));
#45870=CARTESIAN_POINT('Ctrl Pts',(-66.,-3.59461383040384,8.26755365668696));
#45871=CARTESIAN_POINT('Ctrl Pts',(-50.,-3.59461383040384,8.26755365668696));
#45872=CARTESIAN_POINT('Ctrl Pts',(-66.,-3.53867623893612,8.18294180840626));
#45873=CARTESIAN_POINT('Ctrl Pts',(-50.,-3.53867623893612,8.18294180840626));
#45874=CARTESIAN_POINT('Ctrl Pts',(-66.,-3.48773626701595,8.09593368911593));
#45875=CARTESIAN_POINT('Ctrl Pts',(-50.,-3.48773626701595,8.09593368911593));
#45876=CARTESIAN_POINT('Ctrl Pts',(-66.,-3.441640425645,8.00669249258951));
#45877=CARTESIAN_POINT('Ctrl Pts',(-50.,-3.441640425645,8.00669249258951));
#45878=CARTESIAN_POINT('Ctrl Pts',(-66.,-3.39973851923894,7.91556814228226));
#45879=CARTESIAN_POINT('Ctrl Pts',(-50.,-3.39973851923894,7.91556814228226));
#45880=CARTESIAN_POINT('Ctrl Pts',(-66.,-3.3609897589824,7.82305272705443));
#45881=CARTESIAN_POINT('Ctrl Pts',(-50.,-3.3609897589824,7.82305272705443));
#45882=CARTESIAN_POINT('Ctrl Pts',(-66.,-3.32416425071599,7.72970101571594));
#45883=CARTESIAN_POINT('Ctrl Pts',(-50.,-3.32416425071599,7.72970101571594));
#45884=CARTESIAN_POINT('Ctrl Pts',(-66.,-3.28801529731225,7.63606148881098));
#45885=CARTESIAN_POINT('Ctrl Pts',(-50.,-3.28801529731225,7.63606148881098));
#45886=CARTESIAN_POINT('Ctrl Pts',(-66.,-3.25145480239525,7.5426066324152));
#45887=CARTESIAN_POINT('Ctrl Pts',(-50.,-3.25145480239525,7.5426066324152));
#45888=CARTESIAN_POINT('Ctrl Pts',(-66.,-3.21375006071206,7.44965417630122));
#45889=CARTESIAN_POINT('Ctrl Pts',(-50.,-3.21375006071206,7.44965417630122));
#45890=CARTESIAN_POINT('Ctrl Pts',(-66.,-3.17447364404108,7.35738957226508));
#45891=CARTESIAN_POINT('Ctrl Pts',(-50.,-3.17447364404108,7.35738957226508));
#45892=CARTESIAN_POINT('Ctrl Pts',(-66.,-3.14162759082209,7.28420082769005));
#45893=CARTESIAN_POINT('Ctrl Pts',(-50.,-3.14162759082209,7.28420082769005));
#45894=CARTESIAN_POINT('Ctrl Pts',(-66.,-3.11616269844133,7.22967217437288));
#45895=CARTESIAN_POINT('Ctrl Pts',(-50.,-3.11616269844133,7.22967217437288));
#45896=CARTESIAN_POINT('Ctrl Pts',(-66.,-3.09881751111224,7.19348083086667));
#45897=CARTESIAN_POINT('Ctrl Pts',(-50.,-3.09881751111224,7.19348083086667));
#45898=CARTESIAN_POINT('Ctrl Pts',(-66.,-3.09005277149946,7.17542543124437));
#45899=CARTESIAN_POINT('Ctrl Pts',(-50.,-3.09005277149946,7.17542543124437));
#45900=CARTESIAN_POINT('Ctrl Pts',(-50.,-4.47433860192363,9.08272641200518));
#45901=CARTESIAN_POINT('Ctrl Pts',(-50.,-4.46799546208136,9.07840367583189));
#45902=CARTESIAN_POINT('Ctrl Pts',(-50.,-4.44345829930701,9.0616132340732));
#45903=CARTESIAN_POINT('Ctrl Pts',(-50.,-4.40102613216983,9.03211165933191));
#45904=CARTESIAN_POINT('Ctrl Pts',(-50.,-4.34130290913254,8.98941802189944));
#45905=CARTESIAN_POINT('Ctrl Pts',(-50.,-4.26522443974139,8.93281753244224));
#45906=CARTESIAN_POINT('Ctrl Pts',(-50.,-4.17984979305941,8.86613739951103));
#45907=CARTESIAN_POINT('Ctrl Pts',(-50.,-4.09669269754511,8.79784590915275));
#45908=CARTESIAN_POINT('Ctrl Pts',(-50.,-4.01588494277018,8.72789205657743));
#45909=CARTESIAN_POINT('Ctrl Pts',(-50.,-3.93760085807652,8.65619659951692));
#45910=CARTESIAN_POINT('Ctrl Pts',(-50.,-3.86206885883931,8.58265845343488));
#45911=CARTESIAN_POINT('Ctrl Pts',(-50.,-3.78958659965516,8.50715832573905));
#45912=CARTESIAN_POINT('Ctrl Pts',(-50.,-3.720526640373,8.42956563125176));
#45913=CARTESIAN_POINT('Ctrl Pts',(-50.,-3.65536627573726,8.34973908999167));
#45914=CARTESIAN_POINT('Ctrl Pts',(-50.,-3.59461383040384,8.26755365668696));
#45915=CARTESIAN_POINT('Ctrl Pts',(-50.,-3.53867623893612,8.18294180840626));
#45916=CARTESIAN_POINT('Ctrl Pts',(-50.,-3.48773626701595,8.09593368911593));
#45917=CARTESIAN_POINT('Ctrl Pts',(-50.,-3.441640425645,8.00669249258951));
#45918=CARTESIAN_POINT('Ctrl Pts',(-50.,-3.39973851923894,7.91556814228226));
#45919=CARTESIAN_POINT('Ctrl Pts',(-50.,-3.3609897589824,7.82305272705443));
#45920=CARTESIAN_POINT('Ctrl Pts',(-50.,-3.32416425071599,7.72970101571594));
#45921=CARTESIAN_POINT('Ctrl Pts',(-50.,-3.28801529731225,7.63606148881098));
#45922=CARTESIAN_POINT('Ctrl Pts',(-50.,-3.25145480239525,7.5426066324152));
#45923=CARTESIAN_POINT('Ctrl Pts',(-50.,-3.21375006071206,7.44965417630122));
#45924=CARTESIAN_POINT('Ctrl Pts',(-50.,-3.17447364404108,7.35738957226508));
#45925=CARTESIAN_POINT('Ctrl Pts',(-50.,-3.14162759082209,7.28420082769005));
#45926=CARTESIAN_POINT('Ctrl Pts',(-50.,-3.11616269844133,7.22967217437288));
#45927=CARTESIAN_POINT('Ctrl Pts',(-50.,-3.09881751111224,7.19348083086667));
#45928=CARTESIAN_POINT('Ctrl Pts',(-50.,-3.09005277149946,7.17542543124437));
#45929=CARTESIAN_POINT('Origin',(-50.,-3.39879369590239,8.87754687038761));
#45930=CARTESIAN_POINT('Origin',(-50.,0.,0.));
#45931=CARTESIAN_POINT('Origin',(-65.75,0.,0.));
#45932=CARTESIAN_POINT('',(-65.5,-0.730107932396199,10.5998852544286));
#45933=CARTESIAN_POINT('Origin',(-65.5,0.,0.));
#45934=CARTESIAN_POINT('',(-66.,-0.393234054947371,10.1173609196287));
#45935=CARTESIAN_POINT('Ctrl Pts',(-65.5,-0.730107932396319,10.5998852544287));
#45936=CARTESIAN_POINT('Ctrl Pts',(-65.5869131822983,-0.665642665095681,
10.5172110652076));
#45937=CARTESIAN_POINT('Ctrl Pts',(-65.6744370580972,-0.603721341078077,
10.4332627470386));
#45938=CARTESIAN_POINT('Ctrl Pts',(-65.762669377962,-0.544547419148644,
10.3480202685378));
#45939=CARTESIAN_POINT('Ctrl Pts',(-65.8411954666452,-0.491883081995573,
10.2721551157618));
#45940=CARTESIAN_POINT('Ctrl Pts',(-65.9202827042116,-0.441398804290209,
10.1952663740677));
#45941=CARTESIAN_POINT('Ctrl Pts',(-66.,-0.39323405494737,10.1173609196287));
#45942=CARTESIAN_POINT('Origin',(-66.,0.,0.));
#45943=CARTESIAN_POINT('Origin',(-58.,0.,0.));
#45944=CARTESIAN_POINT('',(-50.5,-0.730107932396199,10.5998852544286));
#45945=CARTESIAN_POINT('Origin',(-50.5,0.,0.));
#45946=CARTESIAN_POINT('Ctrl Pts',(-50.5,-0.730107932396198,10.5998852544286));
#45947=CARTESIAN_POINT('Ctrl Pts',(-55.5,-0.730107932396198,10.5998852544286));
#45948=CARTESIAN_POINT('Ctrl Pts',(-60.5,-0.730107932396198,10.5998852544286));
#45949=CARTESIAN_POINT('Ctrl Pts',(-65.5,-0.730107932396198,10.5998852544286));
#45950=CARTESIAN_POINT('Origin',(-50.25,0.,0.));
#45951=CARTESIAN_POINT('',(-50.,-0.393234054947381,10.1173609196287));
#45952=CARTESIAN_POINT('Origin',(-50.,0.,0.));
#45953=CARTESIAN_POINT('Ctrl Pts',(-50.,-0.393234054947385,10.1173609196287));
#45954=CARTESIAN_POINT('Ctrl Pts',(-50.0956594798899,-0.451030983776946,
10.2108462188794));
#45955=CARTESIAN_POINT('Ctrl Pts',(-50.190411700126,-0.512169084664846,
10.3028667171489));
#45956=CARTESIAN_POINT('Ctrl Pts',(-50.2843757312842,-0.576403624495566,
10.3934130596283));
#45957=CARTESIAN_POINT('Ctrl Pts',(-50.3566993358377,-0.625844601006806,
10.4631060877639));
#45958=CARTESIAN_POINT('Ctrl Pts',(-50.4285559937478,-0.677116466219517,
10.5319257673242));
#45959=CARTESIAN_POINT('Ctrl Pts',(-50.5,-0.730107932396319,10.5998852544287));
#45960=CARTESIAN_POINT('Origin',(-66.,0.505871070453596,9.49245655683042));
#45961=CARTESIAN_POINT('',(-66.,2.4750997369136,9.81781575974668));
#45962=CARTESIAN_POINT('Origin',(-66.,0.,0.));
#45963=CARTESIAN_POINT('',(-66.,0.0956047792658118,7.81191500057326));
#45964=CARTESIAN_POINT('Ctrl Pts',(-66.,0.0956047792658046,7.81191500057326));
#45965=CARTESIAN_POINT('Ctrl Pts',(-66.,0.0949415838368861,7.83197436965167));
#45966=CARTESIAN_POINT('Ctrl Pts',(-66.,0.0938163123065552,7.8720917303855));
#45967=CARTESIAN_POINT('Ctrl Pts',(-66.,0.0927317769444286,7.93226363877801));
#45968=CARTESIAN_POINT('Ctrl Pts',(-66.,0.0924939585041115,8.01248457735968));
#45969=CARTESIAN_POINT('Ctrl Pts',(-66.,0.094140561782238,8.11274764514689));
#45970=CARTESIAN_POINT('Ctrl Pts',(-66.,0.0975027362514239,8.2129998392668));
#45971=CARTESIAN_POINT('Ctrl Pts',(-66.,0.102114576760388,8.31324559179353));
#45972=CARTESIAN_POINT('Ctrl Pts',(-66.,0.107177491412388,8.4134926602115));
#45973=CARTESIAN_POINT('Ctrl Pts',(-66.,0.111505277305432,8.51375197567978));
#45974=CARTESIAN_POINT('Ctrl Pts',(-66.,0.113735932806315,8.61402955369318));
#45975=CARTESIAN_POINT('Ctrl Pts',(-66.,0.112520248888933,8.71431883074707));
#45976=CARTESIAN_POINT('Ctrl Pts',(-66.,0.106707267087506,8.81459358824736));
#45977=CARTESIAN_POINT('Ctrl Pts',(-66.,0.095560677487882,8.91479861358025));
#45978=CARTESIAN_POINT('Ctrl Pts',(-66.,0.078873884025214,9.01484725141515));
#45979=CARTESIAN_POINT('Ctrl Pts',(-66.,0.0568015908022762,9.11463762636861));
#45980=CARTESIAN_POINT('Ctrl Pts',(-66.,0.0297430150914363,9.21406590850962));
#45981=CARTESIAN_POINT('Ctrl Pts',(-66.,-0.00178660493279414,9.31303957811411));
#45982=CARTESIAN_POINT('Ctrl Pts',(-66.,-0.0372937750793528,9.41149356760519));
#45983=CARTESIAN_POINT('Ctrl Pts',(-66.,-0.0763850312137404,9.50939563873644));
#45984=CARTESIAN_POINT('Ctrl Pts',(-66.,-0.11873993166277,9.60673370368225));
#45985=CARTESIAN_POINT('Ctrl Pts',(-66.,-0.164108693813002,9.70350720285868));
#45986=CARTESIAN_POINT('Ctrl Pts',(-66.,-0.212299829151872,9.79971762154855));
#45987=CARTESIAN_POINT('Ctrl Pts',(-66.,-0.263172196397742,9.89535795129807));
#45988=CARTESIAN_POINT('Ctrl Pts',(-66.,-0.309651843456158,9.97800897259254));
#45989=CARTESIAN_POINT('Ctrl Pts',(-66.,-0.346846655807676,10.0413031743911));
#45990=CARTESIAN_POINT('Ctrl Pts',(-66.,-0.373610997878055,10.0855129212091));
#45991=CARTESIAN_POINT('Ctrl Pts',(-66.,-0.389197523557302,10.110831916227));
#45992=CARTESIAN_POINT('Ctrl Pts',(-66.,-0.393234054947371,10.1173609196287));
#45993=CARTESIAN_POINT('',(-66.,1.53067287083627,7.66108326625457));
#45994=CARTESIAN_POINT('Origin',(-66.,0.,0.));
#45995=CARTESIAN_POINT('Ctrl Pts',(-66.,2.4750997369136,9.81781575974667));
#45996=CARTESIAN_POINT('Ctrl Pts',(-66.,2.46072168365089,9.80407287462596));
#45997=CARTESIAN_POINT('Ctrl Pts',(-66.,2.42760988208889,9.77134522776358));
#45998=CARTESIAN_POINT('Ctrl Pts',(-66.,2.37903830357638,9.71924627901826));
#45999=CARTESIAN_POINT('Ctrl Pts',(-66.,2.31965175273437,9.64714268794233));
#46000=CARTESIAN_POINT('Ctrl Pts',(-66.,2.25145985312962,9.55424100647557));
#46001=CARTESIAN_POINT('Ctrl Pts',(-66.,2.18075461106815,9.45447850276164));
#46002=CARTESIAN_POINT('Ctrl Pts',(-66.,2.10816197016995,9.35322073006787));
#46003=CARTESIAN_POINT('Ctrl Pts',(-66.,2.0344576270999,9.25038678979018));
#46004=CARTESIAN_POINT('Ctrl Pts',(-66.,1.96244215081495,9.14584421069497));
#46005=CARTESIAN_POINT('Ctrl Pts',(-66.,1.89575134598467,9.03944732712972));
#46006=CARTESIAN_POINT('Ctrl Pts',(-66.,1.83713595327505,8.93108698145603));
#46007=CARTESIAN_POINT('Ctrl Pts',(-66.,1.78758666420428,8.82072595505194));
#46008=CARTESIAN_POINT('Ctrl Pts',(-66.,1.74690297758844,8.70841487822418));
#46009=CARTESIAN_POINT('Ctrl Pts',(-66.,1.71396195582416,8.59430989652968));
#46010=CARTESIAN_POINT('Ctrl Pts',(-66.,1.687108761575,8.4786961492651));
#46011=CARTESIAN_POINT('Ctrl Pts',(-66.,1.66446290264294,8.36199244506075));
#46012=CARTESIAN_POINT('Ctrl Pts',(-66.,1.6441151218745,8.24467002114497));
#46013=CARTESIAN_POINT('Ctrl Pts',(-66.,1.62432848933541,8.1271858608129));
#46014=CARTESIAN_POINT('Ctrl Pts',(-66.,1.60374909373978,8.00990707893858));
#46015=CARTESIAN_POINT('Ctrl Pts',(-66.,1.5815843333707,7.89304829685241));
#46016=CARTESIAN_POINT('Ctrl Pts',(-66.,1.56227021516729,7.79998240099705));
#46017=CARTESIAN_POINT('Ctrl Pts',(-66.,1.54683889623834,7.73043495565091));
#46018=CARTESIAN_POINT('Ctrl Pts',(-66.,1.53613151574638,7.68418185330693));
#46019=CARTESIAN_POINT('Ctrl Pts',(-66.,1.53067287083627,7.66108326625457));
#46020=CARTESIAN_POINT('Ctrl Pts',(-66.,1.53067287083627,7.66108326625457));
#46021=CARTESIAN_POINT('Ctrl Pts',(-50.,1.53067287083627,7.66108326625457));
#46022=CARTESIAN_POINT('Ctrl Pts',(-66.,1.53613151574638,7.68418185330693));
#46023=CARTESIAN_POINT('Ctrl Pts',(-50.,1.53613151574638,7.68418185330693));
#46024=CARTESIAN_POINT('Ctrl Pts',(-66.,1.54683889623834,7.73043495565091));
#46025=CARTESIAN_POINT('Ctrl Pts',(-50.,1.54683889623834,7.73043495565091));
#46026=CARTESIAN_POINT('Ctrl Pts',(-66.,1.56227021516729,7.79998240099705));
#46027=CARTESIAN_POINT('Ctrl Pts',(-50.,1.56227021516729,7.79998240099705));
#46028=CARTESIAN_POINT('Ctrl Pts',(-66.,1.5815843333707,7.89304829685241));
#46029=CARTESIAN_POINT('Ctrl Pts',(-50.,1.5815843333707,7.89304829685241));
#46030=CARTESIAN_POINT('Ctrl Pts',(-66.,1.60374909373978,8.00990707893858));
#46031=CARTESIAN_POINT('Ctrl Pts',(-50.,1.60374909373978,8.00990707893858));
#46032=CARTESIAN_POINT('Ctrl Pts',(-66.,1.62432848933541,8.1271858608129));
#46033=CARTESIAN_POINT('Ctrl Pts',(-50.,1.62432848933541,8.1271858608129));
#46034=CARTESIAN_POINT('Ctrl Pts',(-66.,1.6441151218745,8.24467002114497));
#46035=CARTESIAN_POINT('Ctrl Pts',(-50.,1.6441151218745,8.24467002114497));
#46036=CARTESIAN_POINT('Ctrl Pts',(-66.,1.66446290264294,8.36199244506075));
#46037=CARTESIAN_POINT('Ctrl Pts',(-50.,1.66446290264294,8.36199244506075));
#46038=CARTESIAN_POINT('Ctrl Pts',(-66.,1.687108761575,8.4786961492651));
#46039=CARTESIAN_POINT('Ctrl Pts',(-50.,1.687108761575,8.4786961492651));
#46040=CARTESIAN_POINT('Ctrl Pts',(-66.,1.71396195582416,8.59430989652968));
#46041=CARTESIAN_POINT('Ctrl Pts',(-50.,1.71396195582416,8.59430989652968));
#46042=CARTESIAN_POINT('Ctrl Pts',(-66.,1.74690297758844,8.70841487822418));
#46043=CARTESIAN_POINT('Ctrl Pts',(-50.,1.74690297758844,8.70841487822418));
#46044=CARTESIAN_POINT('Ctrl Pts',(-66.,1.78758666420428,8.82072595505194));
#46045=CARTESIAN_POINT('Ctrl Pts',(-50.,1.78758666420428,8.82072595505194));
#46046=CARTESIAN_POINT('Ctrl Pts',(-66.,1.83713595327505,8.93108698145603));
#46047=CARTESIAN_POINT('Ctrl Pts',(-50.,1.83713595327505,8.93108698145603));
#46048=CARTESIAN_POINT('Ctrl Pts',(-66.,1.89575134598467,9.03944732712972));
#46049=CARTESIAN_POINT('Ctrl Pts',(-50.,1.89575134598467,9.03944732712972));
#46050=CARTESIAN_POINT('Ctrl Pts',(-66.,1.96244215081495,9.14584421069497));
#46051=CARTESIAN_POINT('Ctrl Pts',(-50.,1.96244215081495,9.14584421069497));
#46052=CARTESIAN_POINT('Ctrl Pts',(-66.,2.0344576270999,9.25038678979018));
#46053=CARTESIAN_POINT('Ctrl Pts',(-50.,2.0344576270999,9.25038678979018));
#46054=CARTESIAN_POINT('Ctrl Pts',(-66.,2.10816197016995,9.35322073006787));
#46055=CARTESIAN_POINT('Ctrl Pts',(-50.,2.10816197016995,9.35322073006787));
#46056=CARTESIAN_POINT('Ctrl Pts',(-66.,2.18075461106815,9.45447850276164));
#46057=CARTESIAN_POINT('Ctrl Pts',(-50.,2.18075461106815,9.45447850276164));
#46058=CARTESIAN_POINT('Ctrl Pts',(-66.,2.25145985312962,9.55424100647557));
#46059=CARTESIAN_POINT('Ctrl Pts',(-50.,2.25145985312962,9.55424100647557));
#46060=CARTESIAN_POINT('Ctrl Pts',(-66.,2.32356876504542,9.65247905534274));
#46061=CARTESIAN_POINT('Ctrl Pts',(-50.,2.32356876504542,9.65247905534274));
#46062=CARTESIAN_POINT('Ctrl Pts',(-66.,2.40375833141064,9.74906184805482));
#46063=CARTESIAN_POINT('Ctrl Pts',(-50.,2.40375833141064,9.74906184805482));
#46064=CARTESIAN_POINT('Ctrl Pts',(-66.,2.49824854034584,9.8438431355273));
#46065=CARTESIAN_POINT('Ctrl Pts',(-50.,2.49824854034584,9.8438431355273));
#46066=CARTESIAN_POINT('Ctrl Pts',(-66.,2.60996854609427,9.93672339619266));
#46067=CARTESIAN_POINT('Ctrl Pts',(-50.,2.60996854609427,9.93672339619266));
#46068=CARTESIAN_POINT('Ctrl Pts',(-66.,2.7348865821668,10.0277304471861));
#46069=CARTESIAN_POINT('Ctrl Pts',(-50.,2.7348865821668,10.0277304471861));
#46070=CARTESIAN_POINT('Ctrl Pts',(-66.,2.85989756918902,10.117067973778));
#46071=CARTESIAN_POINT('Ctrl Pts',(-50.,2.85989756918902,10.117067973778));
#46072=CARTESIAN_POINT('Ctrl Pts',(-66.,2.96655997197117,10.2050458427552));
#46073=CARTESIAN_POINT('Ctrl Pts',(-50.,2.96655997197117,10.2050458427552));
#46074=CARTESIAN_POINT('Ctrl Pts',(-66.,3.03402551345445,10.2920269460792));
#46075=CARTESIAN_POINT('Ctrl Pts',(-50.,3.03402551345445,10.2920269460792));
#46076=CARTESIAN_POINT('Ctrl Pts',(-66.,3.04215148505188,10.3783701788403));
#46077=CARTESIAN_POINT('Ctrl Pts',(-50.,3.04215148505188,10.3783701788403));
#46078=CARTESIAN_POINT('Ctrl Pts',(-66.,2.9748385291403,10.4643699989842));
#46079=CARTESIAN_POINT('Ctrl Pts',(-50.,2.9748385291403,10.4643699989842));
#46080=CARTESIAN_POINT('Ctrl Pts',(-66.,2.81986096053206,10.5502574863892));
#46081=CARTESIAN_POINT('Ctrl Pts',(-50.,2.81986096053206,10.5502574863892));
#46082=CARTESIAN_POINT('Ctrl Pts',(-66.,2.56820026819713,10.6362103353318));
#46083=CARTESIAN_POINT('Ctrl Pts',(-50.,2.56820026819713,10.6362103353318));
#46084=CARTESIAN_POINT('Ctrl Pts',(-66.,2.21358394293369,10.7223593673151));
#46085=CARTESIAN_POINT('Ctrl Pts',(-50.,2.21358394293369,10.7223593673151));
#46086=CARTESIAN_POINT('Ctrl Pts',(-66.,1.7519651212833,10.8087962346463));
#46087=CARTESIAN_POINT('Ctrl Pts',(-50.,1.7519651212833,10.8087962346463));
#46088=CARTESIAN_POINT('Ctrl Pts',(-66.,1.18105323929441,10.8955803579119));
#46089=CARTESIAN_POINT('Ctrl Pts',(-50.,1.18105323929441,10.8955803579119));
#46090=CARTESIAN_POINT('Ctrl Pts',(-66.,0.499846109826311,10.9827459672994));
#46091=CARTESIAN_POINT('Ctrl Pts',(-50.,0.499846109826311,10.9827459672994));
#46092=CARTESIAN_POINT('Ctrl Pts',(-66.,-0.133484792308076,11.0527963170055));
#46093=CARTESIAN_POINT('Ctrl Pts',(-50.,-0.133484792308076,11.0527963170055));
#46094=CARTESIAN_POINT('Ctrl Pts',(-66.,-0.658079481550103,11.1055147659729));
#46095=CARTESIAN_POINT('Ctrl Pts',(-50.,-0.658079481550103,11.1055147659729));
#46096=CARTESIAN_POINT('Ctrl Pts',(-66.,-1.02982286576183,11.1407405969304));
#46097=CARTESIAN_POINT('Ctrl Pts',(-50.,-1.02982286576183,11.1407405969304));
#46098=CARTESIAN_POINT('Ctrl Pts',(-66.,-1.22119795728711,11.158373561999));
#46099=CARTESIAN_POINT('Ctrl Pts',(-50.,-1.22119795728711,11.158373561999));
#46100=CARTESIAN_POINT('',(-65.5,2.95714943969769,10.2051894735618));
#46101=CARTESIAN_POINT('Ctrl Pts',(-66.,2.47509973691359,9.81781575974667));
#46102=CARTESIAN_POINT('Ctrl Pts',(-65.7982417703062,2.64735434324867,9.98246080752347));
#46103=CARTESIAN_POINT('Ctrl Pts',(-65.6331946192803,2.85185906302854,10.097025538503));
#46104=CARTESIAN_POINT('Ctrl Pts',(-65.5,2.95714943969768,10.2051894735618));
#46105=CARTESIAN_POINT('',(-50.,1.53067287083627,7.66108326625457));
#46106=CARTESIAN_POINT('',(-66.,1.53067287083627,7.66108326625457));
#46107=CARTESIAN_POINT('',(-50.,2.47509973691361,9.81781575974669));
#46108=CARTESIAN_POINT('Ctrl Pts',(-50.,1.53067287083627,7.66108326625457));
#46109=CARTESIAN_POINT('Ctrl Pts',(-50.,1.53613151574638,7.68418185330693));
#46110=CARTESIAN_POINT('Ctrl Pts',(-50.,1.54683889623834,7.73043495565091));
#46111=CARTESIAN_POINT('Ctrl Pts',(-50.,1.56227021516729,7.79998240099705));
#46112=CARTESIAN_POINT('Ctrl Pts',(-50.,1.5815843333707,7.89304829685241));
#46113=CARTESIAN_POINT('Ctrl Pts',(-50.,1.60374909373978,8.00990707893858));
#46114=CARTESIAN_POINT('Ctrl Pts',(-50.,1.62432848933541,8.1271858608129));
#46115=CARTESIAN_POINT('Ctrl Pts',(-50.,1.6441151218745,8.24467002114497));
#46116=CARTESIAN_POINT('Ctrl Pts',(-50.,1.66446290264294,8.36199244506075));
#46117=CARTESIAN_POINT('Ctrl Pts',(-50.,1.687108761575,8.4786961492651));
#46118=CARTESIAN_POINT('Ctrl Pts',(-50.,1.71396195582416,8.59430989652968));
#46119=CARTESIAN_POINT('Ctrl Pts',(-50.,1.74690297758844,8.70841487822418));
#46120=CARTESIAN_POINT('Ctrl Pts',(-50.,1.78758666420428,8.82072595505194));
#46121=CARTESIAN_POINT('Ctrl Pts',(-50.,1.83713595327505,8.93108698145603));
#46122=CARTESIAN_POINT('Ctrl Pts',(-50.,1.89575134598467,9.03944732712972));
#46123=CARTESIAN_POINT('Ctrl Pts',(-50.,1.96244215081495,9.14584421069497));
#46124=CARTESIAN_POINT('Ctrl Pts',(-50.,2.0344576270999,9.25038678979018));
#46125=CARTESIAN_POINT('Ctrl Pts',(-50.,2.10816197016995,9.35322073006787));
#46126=CARTESIAN_POINT('Ctrl Pts',(-50.,2.18075461106815,9.45447850276164));
#46127=CARTESIAN_POINT('Ctrl Pts',(-50.,2.25145985312962,9.55424100647557));
#46128=CARTESIAN_POINT('Ctrl Pts',(-50.,2.31965175273437,9.64714268794233));
#46129=CARTESIAN_POINT('Ctrl Pts',(-50.,2.37903830357638,9.71924627901827));
#46130=CARTESIAN_POINT('Ctrl Pts',(-50.,2.4276098820889,9.77134522776359));
#46131=CARTESIAN_POINT('Ctrl Pts',(-50.,2.4607216836509,9.80407287462597));
#46132=CARTESIAN_POINT('Ctrl Pts',(-50.,2.47509973691361,9.81781575974669));
#46133=CARTESIAN_POINT('',(-50.5,2.95714943969769,10.2051894735618));
#46134=CARTESIAN_POINT('Ctrl Pts',(-50.5,2.9571494396977,10.2051894735618));
#46135=CARTESIAN_POINT('Ctrl Pts',(-50.4466445089803,2.91497191197781,10.161860847399));
#46136=CARTESIAN_POINT('Ctrl Pts',(-50.3887477139858,2.85816646933579,10.1179041696984));
#46137=CARTESIAN_POINT('Ctrl Pts',(-50.2270346138796,2.69292179906152,9.99595555654163));
#46138=CARTESIAN_POINT('Ctrl Pts',(-50.1250229592142,2.58184026816719,9.91984089708192));
#46139=CARTESIAN_POINT('Ctrl Pts',(-50.,2.47509973691361,9.81781575974669));
#46140=CARTESIAN_POINT('Ctrl Pts',(-65.5,2.95714943969769,10.2051894735618));
#46141=CARTESIAN_POINT('Ctrl Pts',(-60.5,2.95714943969769,10.2051894735618));
#46142=CARTESIAN_POINT('Ctrl Pts',(-55.5,2.95714943969769,10.2051894735618));
#46143=CARTESIAN_POINT('Ctrl Pts',(-50.5,2.95714943969769,10.2051894735618));
#46144=CARTESIAN_POINT('Origin',(-66.,0.,0.));
#46145=CARTESIAN_POINT('',(-50.,0.0956047792658118,7.81191500057326));
#46146=CARTESIAN_POINT('',(-66.,0.0956047792658118,7.81191500057326));
#46147=CARTESIAN_POINT('Origin',(-50.,0.,0.));
#46148=CARTESIAN_POINT('Ctrl Pts',(-66.,-1.22119795728711,11.158373561999));
#46149=CARTESIAN_POINT('Ctrl Pts',(-50.,-1.22119795728711,11.158373561999));
#46150=CARTESIAN_POINT('Ctrl Pts',(-66.,-1.20459005337381,11.1414802084975));
#46151=CARTESIAN_POINT('Ctrl Pts',(-50.,-1.20459005337381,11.1414802084975));
#46152=CARTESIAN_POINT('Ctrl Pts',(-66.,-1.17157016007181,11.1076086480398));
#46153=CARTESIAN_POINT('Ctrl Pts',(-50.,-1.17157016007181,11.1076086480398));
#46154=CARTESIAN_POINT('Ctrl Pts',(-66.,-1.12262806377916,11.0565467472304));
#46155=CARTESIAN_POINT('Ctrl Pts',(-50.,-1.12262806377916,11.0565467472304));
#46156=CARTESIAN_POINT('Ctrl Pts',(-66.,-1.05854898513006,10.9879544134138));
#46157=CARTESIAN_POINT('Ctrl Pts',(-50.,-1.05854898513006,10.9879544134138));
#46158=CARTESIAN_POINT('Ctrl Pts',(-66.,-0.98042435206805,10.9013612443196));
#46159=CARTESIAN_POINT('Ctrl Pts',(-50.,-0.98042435206805,10.9013612443196));
#46160=CARTESIAN_POINT('Ctrl Pts',(-66.,-0.904295528615561,10.813912873378));
#46161=CARTESIAN_POINT('Ctrl Pts',(-50.,-0.904295528615561,10.813912873378));
#46162=CARTESIAN_POINT('Ctrl Pts',(-66.,-0.830193774749181,10.7256096737113));
#46163=CARTESIAN_POINT('Ctrl Pts',(-50.,-0.830193774749181,10.7256096737113));
#46164=CARTESIAN_POINT('Ctrl Pts',(-66.,-0.758160207908483,10.6364569134394));
#46165=CARTESIAN_POINT('Ctrl Pts',(-50.,-0.758160207908483,10.6364569134394));
#46166=CARTESIAN_POINT('Ctrl Pts',(-66.,-0.688246412921118,10.5464674190292));
#46167=CARTESIAN_POINT('Ctrl Pts',(-50.,-0.688246412921118,10.5464674190292));
#46168=CARTESIAN_POINT('Ctrl Pts',(-66.,-0.62051145560108,10.4556610008753));
#46169=CARTESIAN_POINT('Ctrl Pts',(-50.,-0.62051145560108,10.4556610008753));
#46170=CARTESIAN_POINT('Ctrl Pts',(-66.,-0.55501808912882,10.3640630895747));
#46171=CARTESIAN_POINT('Ctrl Pts',(-50.,-0.55501808912882,10.3640630895747));
#46172=CARTESIAN_POINT('Ctrl Pts',(-66.,-0.491828620657976,10.2717038296071));
#46173=CARTESIAN_POINT('Ctrl Pts',(-50.,-0.491828620657976,10.2717038296071));
#46174=CARTESIAN_POINT('Ctrl Pts',(-66.,-0.431001555210865,10.1786169559436));
#46175=CARTESIAN_POINT('Ctrl Pts',(-50.,-0.431001555210865,10.1786169559436));
#46176=CARTESIAN_POINT('Ctrl Pts',(-66.,-0.372585367340722,10.0848392482018));
#46177=CARTESIAN_POINT('Ctrl Pts',(-50.,-0.372585367340722,10.0848392482018));
#46178=CARTESIAN_POINT('Ctrl Pts',(-66.,-0.316624584267477,9.99040803725309));
#46179=CARTESIAN_POINT('Ctrl Pts',(-50.,-0.316624584267477,9.99040803725309));
#46180=CARTESIAN_POINT('Ctrl Pts',(-66.,-0.263172196397742,9.89535795129807));
#46181=CARTESIAN_POINT('Ctrl Pts',(-50.,-0.263172196397742,9.89535795129807));
#46182=CARTESIAN_POINT('Ctrl Pts',(-66.,-0.212299829151872,9.79971762154855));
#46183=CARTESIAN_POINT('Ctrl Pts',(-50.,-0.212299829151872,9.79971762154855));
#46184=CARTESIAN_POINT('Ctrl Pts',(-66.,-0.164108693813002,9.70350720285868));
#46185=CARTESIAN_POINT('Ctrl Pts',(-50.,-0.164108693813002,9.70350720285868));
#46186=CARTESIAN_POINT('Ctrl Pts',(-66.,-0.11873993166277,9.60673370368225));
#46187=CARTESIAN_POINT('Ctrl Pts',(-50.,-0.11873993166277,9.60673370368225));
#46188=CARTESIAN_POINT('Ctrl Pts',(-66.,-0.0763850312137404,9.50939563873644));
#46189=CARTESIAN_POINT('Ctrl Pts',(-50.,-0.0763850312137404,9.50939563873644));
#46190=CARTESIAN_POINT('Ctrl Pts',(-66.,-0.0372937750793528,9.41149356760519));
#46191=CARTESIAN_POINT('Ctrl Pts',(-50.,-0.0372937750793528,9.41149356760519));
#46192=CARTESIAN_POINT('Ctrl Pts',(-66.,-0.00178660493279414,9.31303957811411));
#46193=CARTESIAN_POINT('Ctrl Pts',(-50.,-0.00178660493279414,9.31303957811411));
#46194=CARTESIAN_POINT('Ctrl Pts',(-66.,0.0297430150914363,9.21406590850962));
#46195=CARTESIAN_POINT('Ctrl Pts',(-50.,0.0297430150914363,9.21406590850962));
#46196=CARTESIAN_POINT('Ctrl Pts',(-66.,0.0568015908022762,9.11463762636861));
#46197=CARTESIAN_POINT('Ctrl Pts',(-50.,0.0568015908022762,9.11463762636861));
#46198=CARTESIAN_POINT('Ctrl Pts',(-66.,0.078873884025214,9.01484725141515));
#46199=CARTESIAN_POINT('Ctrl Pts',(-50.,0.078873884025214,9.01484725141515));
#46200=CARTESIAN_POINT('Ctrl Pts',(-66.,0.095560677487882,8.91479861358025));
#46201=CARTESIAN_POINT('Ctrl Pts',(-50.,0.095560677487882,8.91479861358025));
#46202=CARTESIAN_POINT('Ctrl Pts',(-66.,0.106707267087506,8.81459358824736));
#46203=CARTESIAN_POINT('Ctrl Pts',(-50.,0.106707267087506,8.81459358824736));
#46204=CARTESIAN_POINT('Ctrl Pts',(-66.,0.112520248888933,8.71431883074707));
#46205=CARTESIAN_POINT('Ctrl Pts',(-50.,0.112520248888933,8.71431883074707));
#46206=CARTESIAN_POINT('Ctrl Pts',(-66.,0.113735932806315,8.61402955369318));
#46207=CARTESIAN_POINT('Ctrl Pts',(-50.,0.113735932806315,8.61402955369318));
#46208=CARTESIAN_POINT('Ctrl Pts',(-66.,0.111505277305432,8.51375197567978));
#46209=CARTESIAN_POINT('Ctrl Pts',(-50.,0.111505277305432,8.51375197567978));
#46210=CARTESIAN_POINT('Ctrl Pts',(-66.,0.107177491412388,8.4134926602115));
#46211=CARTESIAN_POINT('Ctrl Pts',(-50.,0.107177491412388,8.4134926602115));
#46212=CARTESIAN_POINT('Ctrl Pts',(-66.,0.102114576760388,8.31324559179353));
#46213=CARTESIAN_POINT('Ctrl Pts',(-50.,0.102114576760388,8.31324559179353));
#46214=CARTESIAN_POINT('Ctrl Pts',(-66.,0.0975027362514239,8.2129998392668));
#46215=CARTESIAN_POINT('Ctrl Pts',(-50.,0.0975027362514239,8.2129998392668));
#46216=CARTESIAN_POINT('Ctrl Pts',(-66.,0.094140561782238,8.11274764514689));
#46217=CARTESIAN_POINT('Ctrl Pts',(-50.,0.094140561782238,8.11274764514689));
#46218=CARTESIAN_POINT('Ctrl Pts',(-66.,0.0924939585041115,8.01248457735968));
#46219=CARTESIAN_POINT('Ctrl Pts',(-50.,0.0924939585041115,8.01248457735968));
#46220=CARTESIAN_POINT('Ctrl Pts',(-66.,0.0927317769444286,7.93226363877801));
#46221=CARTESIAN_POINT('Ctrl Pts',(-50.,0.0927317769444286,7.93226363877801));
#46222=CARTESIAN_POINT('Ctrl Pts',(-66.,0.0938163123065552,7.8720917303855));
#46223=CARTESIAN_POINT('Ctrl Pts',(-50.,0.0938163123065552,7.8720917303855));
#46224=CARTESIAN_POINT('Ctrl Pts',(-66.,0.0949415838368861,7.83197436965167));
#46225=CARTESIAN_POINT('Ctrl Pts',(-50.,0.0949415838368861,7.83197436965167));
#46226=CARTESIAN_POINT('Ctrl Pts',(-66.,0.0956047792658046,7.81191500057326));
#46227=CARTESIAN_POINT('Ctrl Pts',(-50.,0.0956047792658046,7.81191500057326));
#46228=CARTESIAN_POINT('Ctrl Pts',(-50.,-0.393234054947381,10.1173609196287));
#46229=CARTESIAN_POINT('Ctrl Pts',(-50.,-0.389197523557309,10.110831916227));
#46230=CARTESIAN_POINT('Ctrl Pts',(-50.,-0.373610997878061,10.0855129212091));
#46231=CARTESIAN_POINT('Ctrl Pts',(-50.,-0.34684665580768,10.0413031743911));
#46232=CARTESIAN_POINT('Ctrl Pts',(-50.,-0.30965184345616,9.97800897259254));
#46233=CARTESIAN_POINT('Ctrl Pts',(-50.,-0.263172196397742,9.89535795129807));
#46234=CARTESIAN_POINT('Ctrl Pts',(-50.,-0.212299829151872,9.79971762154855));
#46235=CARTESIAN_POINT('Ctrl Pts',(-50.,-0.164108693813002,9.70350720285868));
#46236=CARTESIAN_POINT('Ctrl Pts',(-50.,-0.11873993166277,9.60673370368225));
#46237=CARTESIAN_POINT('Ctrl Pts',(-50.,-0.0763850312137404,9.50939563873644));
#46238=CARTESIAN_POINT('Ctrl Pts',(-50.,-0.0372937750793528,9.41149356760519));
#46239=CARTESIAN_POINT('Ctrl Pts',(-50.,-0.00178660493279414,9.31303957811411));
#46240=CARTESIAN_POINT('Ctrl Pts',(-50.,0.0297430150914363,9.21406590850962));
#46241=CARTESIAN_POINT('Ctrl Pts',(-50.,0.0568015908022762,9.11463762636861));
#46242=CARTESIAN_POINT('Ctrl Pts',(-50.,0.078873884025214,9.01484725141515));
#46243=CARTESIAN_POINT('Ctrl Pts',(-50.,0.095560677487882,8.91479861358025));
#46244=CARTESIAN_POINT('Ctrl Pts',(-50.,0.106707267087506,8.81459358824736));
#46245=CARTESIAN_POINT('Ctrl Pts',(-50.,0.112520248888933,8.71431883074707));
#46246=CARTESIAN_POINT('Ctrl Pts',(-50.,0.113735932806315,8.61402955369318));
#46247=CARTESIAN_POINT('Ctrl Pts',(-50.,0.111505277305432,8.51375197567978));
#46248=CARTESIAN_POINT('Ctrl Pts',(-50.,0.107177491412388,8.4134926602115));
#46249=CARTESIAN_POINT('Ctrl Pts',(-50.,0.102114576760388,8.31324559179353));
#46250=CARTESIAN_POINT('Ctrl Pts',(-50.,0.0975027362514239,8.2129998392668));
#46251=CARTESIAN_POINT('Ctrl Pts',(-50.,0.094140561782238,8.11274764514689));
#46252=CARTESIAN_POINT('Ctrl Pts',(-50.,0.0924939585041115,8.01248457735968));
#46253=CARTESIAN_POINT('Ctrl Pts',(-50.,0.0927317769444286,7.93226363877801));
#46254=CARTESIAN_POINT('Ctrl Pts',(-50.,0.0938163123065552,7.8720917303855));
#46255=CARTESIAN_POINT('Ctrl Pts',(-50.,0.0949415838368861,7.83197436965167));
#46256=CARTESIAN_POINT('Ctrl Pts',(-50.,0.0956047792658046,7.81191500057326));
#46257=CARTESIAN_POINT('Origin',(-50.,0.505871070453596,9.49245655683042));
#46258=CARTESIAN_POINT('Origin',(-50.,0.,0.));
#46259=CARTESIAN_POINT('Origin',(-65.75,0.,0.));
#46260=CARTESIAN_POINT('',(-65.5,3.64437496014557,9.98043867522185));
#46261=CARTESIAN_POINT('Origin',(-65.5,0.,0.));
#46262=CARTESIAN_POINT('',(-66.,3.7558642325485,9.40261181090992));
#46263=CARTESIAN_POINT('Ctrl Pts',(-65.5,3.64437496014557,9.98043867522184));
#46264=CARTESIAN_POINT('Ctrl Pts',(-65.6642917360006,3.69213647626342,9.78809637135388));
#46265=CARTESIAN_POINT('Ctrl Pts',(-65.8311182354843,3.72977758693438,9.59488878684897));
#46266=CARTESIAN_POINT('Ctrl Pts',(-66.,3.7558642325485,9.40261181090993));
#46267=CARTESIAN_POINT('Origin',(-66.,0.,0.));
#46268=CARTESIAN_POINT('Origin',(-58.,0.,0.));
#46269=CARTESIAN_POINT('',(-50.5,3.64437496014557,9.98043867522185));
#46270=CARTESIAN_POINT('Origin',(-50.5,0.,0.));
#46271=CARTESIAN_POINT('Ctrl Pts',(-50.5,3.64437496014557,9.98043867522185));
#46272=CARTESIAN_POINT('Ctrl Pts',(-55.5,3.64437496014557,9.98043867522185));
#46273=CARTESIAN_POINT('Ctrl Pts',(-60.5,3.64437496014557,9.98043867522185));
#46274=CARTESIAN_POINT('Ctrl Pts',(-65.5,3.64437496014557,9.98043867522185));
#46275=CARTESIAN_POINT('Origin',(-50.25,0.,0.));
#46276=CARTESIAN_POINT('',(-50.,3.7558642325485,9.40261181090994));
#46277=CARTESIAN_POINT('Origin',(-50.,0.,0.));
#46278=CARTESIAN_POINT('Ctrl Pts',(-50.,3.7558642325485,9.40261181090995));
#46279=CARTESIAN_POINT('Ctrl Pts',(-50.1688817645159,3.72977758693434,9.59488878684923));
#46280=CARTESIAN_POINT('Ctrl Pts',(-50.3357082639996,3.69213647626336,9.78809637135414));
#46281=CARTESIAN_POINT('Ctrl Pts',(-50.5,3.64437496014557,9.98043867522185));
#46282=CARTESIAN_POINT('Origin',(-66.,4.32306613303376,8.4660342683367));
#46283=CARTESIAN_POINT('',(-66.,6.25438154632586,7.96230723301848));
#46284=CARTESIAN_POINT('Origin',(-66.,0.,0.));
#46285=CARTESIAN_POINT('',(-66.,3.26473139515386,7.09765349728322));
#46286=CARTESIAN_POINT('Ctrl Pts',(-66.,3.26473139515386,7.09765349728322));
#46287=CARTESIAN_POINT('Ctrl Pts',(-66.,3.27228441642341,7.11624838867044));
#46288=CARTESIAN_POINT('Ctrl Pts',(-66.,3.2875736303622,7.15335511050624));
#46289=CARTESIAN_POINT('Ctrl Pts',(-66.,3.31105697803551,7.20876600436839));
#46290=CARTESIAN_POINT('Ctrl Pts',(-66.,3.34346851534271,7.28214820789157));
#46291=CARTESIAN_POINT('Ctrl Pts',(-66.,3.38575342590423,7.37307334414807));
#46292=CARTESIAN_POINT('Ctrl Pts',(-66.,3.42960116601568,7.46329076114798));
#46293=CARTESIAN_POINT('Ctrl Pts',(-66.,3.47458791282935,7.55299400848973));
#46294=CARTESIAN_POINT('Ctrl Pts',(-66.,3.51998727159863,7.64251498957522));
#46295=CARTESIAN_POINT('Ctrl Pts',(-66.,3.56472003815351,7.73234616270153));
#46296=CARTESIAN_POINT('Ctrl Pts',(-66.,3.60754440881085,7.82304699926879));
#46297=CARTESIAN_POINT('Ctrl Pts',(-66.,3.6472251501756,7.91516027596723));
#46298=CARTESIAN_POINT('Ctrl Pts',(-66.,3.68270014530645,8.009130177902));
#46299=CARTESIAN_POINT('Ctrl Pts',(-66.,3.71327428463273,8.10520575006332));
#46300=CARTESIAN_POINT('Ctrl Pts',(-66.,3.73872358735957,8.20339185905743));
#46301=CARTESIAN_POINT('Ctrl Pts',(-66.,3.75914794626584,8.3035325132631));
#46302=CARTESIAN_POINT('Ctrl Pts',(-66.,3.77486983303976,8.40537048302527));
#46303=CARTESIAN_POINT('Ctrl Pts',(-66.,3.78632231001325,8.50861168112478));
#46304=CARTESIAN_POINT('Ctrl Pts',(-66.,3.79392974119514,8.61299594320168));
#46305=CARTESIAN_POINT('Ctrl Pts',(-66.,3.79803846148212,8.71833378187116));
#46306=CARTESIAN_POINT('Ctrl Pts',(-66.,3.79893629234755,8.82448381898456));
#46307=CARTESIAN_POINT('Ctrl Pts',(-66.,3.79685119396006,8.93134394759486));
#46308=CARTESIAN_POINT('Ctrl Pts',(-66.,3.79195870389943,9.03883763918063));
#46309=CARTESIAN_POINT('Ctrl Pts',(-66.,3.78438491054742,9.14690108386965));
#46310=CARTESIAN_POINT('Ctrl Pts',(-66.,3.77554083905247,9.24131152455862));
#46311=CARTESIAN_POINT('Ctrl Pts',(-66.,3.76730575834657,9.31426214822247));
#46312=CARTESIAN_POINT('Ctrl Pts',(-66.,3.76083703923337,9.36553580025943));
#46313=CARTESIAN_POINT('Ctrl Pts',(-66.,3.7568962025383,9.39500546428211));
#46314=CARTESIAN_POINT('Ctrl Pts',(-66.,3.7558642325485,9.40261181090992));
#46315=CARTESIAN_POINT('',(-66.,4.51438253832981,6.37616707337746));
#46316=CARTESIAN_POINT('Origin',(-66.,0.,0.));
#46317=CARTESIAN_POINT('Ctrl Pts',(-66.,6.25438154632586,7.96230723301848));
#46318=CARTESIAN_POINT('Ctrl Pts',(-66.,6.2356568061178,7.95560056385959));
#46319=CARTESIAN_POINT('Ctrl Pts',(-66.,6.1920961369859,7.93917015374265));
#46320=CARTESIAN_POINT('Ctrl Pts',(-66.,6.12653324054481,7.91133123656148));
#46321=CARTESIAN_POINT('Ctrl Pts',(-66.,6.04295375419009,7.86961601478767));
#46322=CARTESIAN_POINT('Ctrl Pts',(-66.,5.94287083600227,7.81248225000655));
#46323=CARTESIAN_POINT('Ctrl Pts',(-66.,5.83770131742005,7.75010308069958));
#46324=CARTESIAN_POINT('Ctrl Pts',(-66.,5.73019939351842,7.68712558947513));
#46325=CARTESIAN_POINT('Ctrl Pts',(-66.,5.62104079403545,7.62316036752337));
#46326=CARTESIAN_POINT('Ctrl Pts',(-66.,5.51273008511568,7.55694730233435));
#46327=CARTESIAN_POINT('Ctrl Pts',(-66.,5.4085294920414,7.48687450672668));
#46328=CARTESIAN_POINT('Ctrl Pts',(-66.,5.31090754304174,7.41172343321117));
#46329=CARTESIAN_POINT('Ctrl Pts',(-66.,5.22075414167572,7.33105713034238));
#46330=CARTESIAN_POINT('Ctrl Pts',(-66.,5.13790671419851,7.2450034023855));
#46331=CARTESIAN_POINT('Ctrl Pts',(-66.,5.061402916183,7.15416163527599));
#46332=CARTESIAN_POINT('Ctrl Pts',(-66.,4.98984695509768,7.05946539970615));
#46333=CARTESIAN_POINT('Ctrl Pts',(-66.,4.9216912606533,6.9620621614818));
#46334=CARTESIAN_POINT('Ctrl Pts',(-66.,4.85538330909815,6.86315898207772));
#46335=CARTESIAN_POINT('Ctrl Pts',(-66.,4.78952220783198,6.76387980955812));
#46336=CARTESIAN_POINT('Ctrl Pts',(-66.,4.72302041642098,6.66511070538007));
#46337=CARTESIAN_POINT('Ctrl Pts',(-66.,4.65524115152641,6.56737011604671));
#46338=CARTESIAN_POINT('Ctrl Pts',(-66.,4.59974351650827,6.49020594922863));
#46339=CARTESIAN_POINT('Ctrl Pts',(-66.,4.5573588107407,6.43294767930141));
#46340=CARTESIAN_POINT('Ctrl Pts',(-66.,4.52876430034979,6.39504845175062));
#46341=CARTESIAN_POINT('Ctrl Pts',(-66.,4.51438253832981,6.37616707337746));
#46342=CARTESIAN_POINT('Ctrl Pts',(-66.,4.51438253832981,6.37616707337746));
#46343=CARTESIAN_POINT('Ctrl Pts',(-50.,4.51438253832981,6.37616707337746));
#46344=CARTESIAN_POINT('Ctrl Pts',(-66.,4.52876430034979,6.39504845175062));
#46345=CARTESIAN_POINT('Ctrl Pts',(-50.,4.52876430034979,6.39504845175062));
#46346=CARTESIAN_POINT('Ctrl Pts',(-66.,4.5573588107407,6.43294767930141));
#46347=CARTESIAN_POINT('Ctrl Pts',(-50.,4.5573588107407,6.43294767930141));
#46348=CARTESIAN_POINT('Ctrl Pts',(-66.,4.59974351650827,6.49020594922863));
#46349=CARTESIAN_POINT('Ctrl Pts',(-50.,4.59974351650827,6.49020594922863));
#46350=CARTESIAN_POINT('Ctrl Pts',(-66.,4.65524115152641,6.56737011604671));
#46351=CARTESIAN_POINT('Ctrl Pts',(-50.,4.65524115152641,6.56737011604671));
#46352=CARTESIAN_POINT('Ctrl Pts',(-66.,4.72302041642098,6.66511070538007));
#46353=CARTESIAN_POINT('Ctrl Pts',(-50.,4.72302041642098,6.66511070538007));
#46354=CARTESIAN_POINT('Ctrl Pts',(-66.,4.78952220783198,6.76387980955812));
#46355=CARTESIAN_POINT('Ctrl Pts',(-50.,4.78952220783198,6.76387980955812));
#46356=CARTESIAN_POINT('Ctrl Pts',(-66.,4.85538330909815,6.86315898207772));
#46357=CARTESIAN_POINT('Ctrl Pts',(-50.,4.85538330909815,6.86315898207772));
#46358=CARTESIAN_POINT('Ctrl Pts',(-66.,4.9216912606533,6.9620621614818));
#46359=CARTESIAN_POINT('Ctrl Pts',(-50.,4.9216912606533,6.9620621614818));
#46360=CARTESIAN_POINT('Ctrl Pts',(-66.,4.98984695509768,7.05946539970615));
#46361=CARTESIAN_POINT('Ctrl Pts',(-50.,4.98984695509768,7.05946539970615));
#46362=CARTESIAN_POINT('Ctrl Pts',(-66.,5.061402916183,7.15416163527599));
#46363=CARTESIAN_POINT('Ctrl Pts',(-50.,5.061402916183,7.15416163527599));
#46364=CARTESIAN_POINT('Ctrl Pts',(-66.,5.13790671419851,7.2450034023855));
#46365=CARTESIAN_POINT('Ctrl Pts',(-50.,5.13790671419851,7.2450034023855));
#46366=CARTESIAN_POINT('Ctrl Pts',(-66.,5.22075414167572,7.33105713034238));
#46367=CARTESIAN_POINT('Ctrl Pts',(-50.,5.22075414167572,7.33105713034238));
#46368=CARTESIAN_POINT('Ctrl Pts',(-66.,5.31090754304174,7.41172343321117));
#46369=CARTESIAN_POINT('Ctrl Pts',(-50.,5.31090754304174,7.41172343321117));
#46370=CARTESIAN_POINT('Ctrl Pts',(-66.,5.4085294920414,7.48687450672668));
#46371=CARTESIAN_POINT('Ctrl Pts',(-50.,5.4085294920414,7.48687450672668));
#46372=CARTESIAN_POINT('Ctrl Pts',(-66.,5.51273008511568,7.55694730233435));
#46373=CARTESIAN_POINT('Ctrl Pts',(-50.,5.51273008511568,7.55694730233435));
#46374=CARTESIAN_POINT('Ctrl Pts',(-66.,5.62104079403545,7.62316036752337));
#46375=CARTESIAN_POINT('Ctrl Pts',(-50.,5.62104079403545,7.62316036752337));
#46376=CARTESIAN_POINT('Ctrl Pts',(-66.,5.73019939351842,7.68712558947513));
#46377=CARTESIAN_POINT('Ctrl Pts',(-50.,5.73019939351842,7.68712558947513));
#46378=CARTESIAN_POINT('Ctrl Pts',(-66.,5.83770131742005,7.75010308069958));
#46379=CARTESIAN_POINT('Ctrl Pts',(-50.,5.83770131742005,7.75010308069958));
#46380=CARTESIAN_POINT('Ctrl Pts',(-66.,5.94287083600227,7.81248225000655));
#46381=CARTESIAN_POINT('Ctrl Pts',(-50.,5.94287083600227,7.81248225000655));
#46382=CARTESIAN_POINT('Ctrl Pts',(-66.,6.04870261915705,7.87289783654834));
#46383=CARTESIAN_POINT('Ctrl Pts',(-50.,6.04870261915705,7.87289783654834));
#46384=CARTESIAN_POINT('Ctrl Pts',(-66.,6.16124319414692,7.92851457308381));
#46385=CARTESIAN_POINT('Ctrl Pts',(-50.,6.16124319414692,7.92851457308381));
#46386=CARTESIAN_POINT('Ctrl Pts',(-66.,6.28611531800434,7.97666895733798));
#46387=CARTESIAN_POINT('Ctrl Pts',(-50.,6.28611531800434,7.97666895733798));
#46388=CARTESIAN_POINT('Ctrl Pts',(-66.,6.42595442721465,8.01607867747095));
#46389=CARTESIAN_POINT('Ctrl Pts',(-50.,6.42595442721465,8.01607867747095));
#46390=CARTESIAN_POINT('Ctrl Pts',(-66.,6.57708863406363,8.04840901286766));
#46391=CARTESIAN_POINT('Ctrl Pts',(-50.,6.57708863406363,8.04840901286766));
#46392=CARTESIAN_POINT('Ctrl Pts',(-66.,6.72762869907988,8.07917635527372));
#46393=CARTESIAN_POINT('Ctrl Pts',(-50.,6.72762869907988,8.07917635527372));
#46394=CARTESIAN_POINT('Ctrl Pts',(-66.,6.86085347573554,8.11616463020096));
#46395=CARTESIAN_POINT('Ctrl Pts',(-50.,6.86085347573554,8.11616463020096));
#46396=CARTESIAN_POINT('Ctrl Pts',(-66.,6.95786471668201,8.16818511417712));
#46397=CARTESIAN_POINT('Ctrl Pts',(-50.,6.95786471668201,8.16818511417712));
#46398=CARTESIAN_POINT('Ctrl Pts',(-66.,7.00040711776935,8.24375845185494));
#46399=CARTESIAN_POINT('Ctrl Pts',(-50.,7.00040711776935,8.24375845185494));
#46400=CARTESIAN_POINT('Ctrl Pts',(-66.,6.97389295080625,8.3497018426284));
#46401=CARTESIAN_POINT('Ctrl Pts',(-50.,6.97389295080625,8.3497018426284));
#46402=CARTESIAN_POINT('Ctrl Pts',(-66.,6.86724748527703,8.49119902262338));
#46403=CARTESIAN_POINT('Ctrl Pts',(-50.,6.86724748527703,8.49119902262338));
#46404=CARTESIAN_POINT('Ctrl Pts',(-66.,6.672304176169,8.67208048254081));
#46405=CARTESIAN_POINT('Ctrl Pts',(-50.,6.672304176169,8.67208048254081));
#46406=CARTESIAN_POINT('Ctrl Pts',(-66.,6.38338601109175,8.89501699310692));
#46407=CARTESIAN_POINT('Ctrl Pts',(-50.,6.38338601109175,8.89501699310692));
#46408=CARTESIAN_POINT('Ctrl Pts',(-66.,5.99683327466702,9.16173829052894));
#46409=CARTESIAN_POINT('Ctrl Pts',(-50.,5.99683327466702,9.16173829052894));
#46410=CARTESIAN_POINT('Ctrl Pts',(-66.,5.51057760113121,9.47323031450598));
#46411=CARTESIAN_POINT('Ctrl Pts',(-50.,5.51057760113121,9.47323031450598));
#46412=CARTESIAN_POINT('Ctrl Pts',(-66.,4.92371736964581,9.82993196210374));
#46413=CARTESIAN_POINT('Ctrl Pts',(-50.,4.92371736964581,9.82993196210374));
#46414=CARTESIAN_POINT('Ctrl Pts',(-66.,4.37363284490199,10.1515250259743));
#46415=CARTESIAN_POINT('Ctrl Pts',(-50.,4.37363284490199,10.1515250259743));
#46416=CARTESIAN_POINT('Ctrl Pts',(-66.,3.91583427440266,10.4130576084401));
#46417=CARTESIAN_POINT('Ctrl Pts',(-50.,3.91583427440266,10.4130576084401));
#46418=CARTESIAN_POINT('Ctrl Pts',(-66.,3.59055743058054,10.5964396624829));
#46419=CARTESIAN_POINT('Ctrl Pts',(-50.,3.59055743058054,10.5964396624829));
#46420=CARTESIAN_POINT('Ctrl Pts',(-66.,3.42289955803116,10.6903874399214));
#46421=CARTESIAN_POINT('Ctrl Pts',(-50.,3.42289955803116,10.6903874399214));
#46422=CARTESIAN_POINT('',(-65.5,6.85231494663519,8.12012345177831));
#46423=CARTESIAN_POINT('Ctrl Pts',(-66.,6.25438154632586,7.96230723301848));
#46424=CARTESIAN_POINT('Ctrl Pts',(-65.7982417703063,6.478711133533,8.04265570820322));
#46425=CARTESIAN_POINT('Ctrl Pts',(-65.6331946192803,6.71213316544796,8.06413623457925));
#46426=CARTESIAN_POINT('Ctrl Pts',(-65.5,6.85231494663518,8.1201234517783));
#46427=CARTESIAN_POINT('',(-50.,4.51438253832981,6.37616707337746));
#46428=CARTESIAN_POINT('',(-66.,4.51438253832981,6.37616707337746));
#46429=CARTESIAN_POINT('',(-50.,6.25438154632588,7.96230723301849));
#46430=CARTESIAN_POINT('Ctrl Pts',(-50.,4.51438253832981,6.37616707337746));
#46431=CARTESIAN_POINT('Ctrl Pts',(-50.,4.52876430034979,6.39504845175062));
#46432=CARTESIAN_POINT('Ctrl Pts',(-50.,4.5573588107407,6.43294767930141));
#46433=CARTESIAN_POINT('Ctrl Pts',(-50.,4.59974351650827,6.49020594922863));
#46434=CARTESIAN_POINT('Ctrl Pts',(-50.,4.65524115152641,6.56737011604671));
#46435=CARTESIAN_POINT('Ctrl Pts',(-50.,4.72302041642098,6.66511070538007));
#46436=CARTESIAN_POINT('Ctrl Pts',(-50.,4.78952220783198,6.76387980955812));
#46437=CARTESIAN_POINT('Ctrl Pts',(-50.,4.85538330909815,6.86315898207772));
#46438=CARTESIAN_POINT('Ctrl Pts',(-50.,4.9216912606533,6.9620621614818));
#46439=CARTESIAN_POINT('Ctrl Pts',(-50.,4.98984695509768,7.05946539970615));
#46440=CARTESIAN_POINT('Ctrl Pts',(-50.,5.061402916183,7.15416163527599));
#46441=CARTESIAN_POINT('Ctrl Pts',(-50.,5.13790671419851,7.2450034023855));
#46442=CARTESIAN_POINT('Ctrl Pts',(-50.,5.22075414167572,7.33105713034238));
#46443=CARTESIAN_POINT('Ctrl Pts',(-50.,5.31090754304174,7.41172343321117));
#46444=CARTESIAN_POINT('Ctrl Pts',(-50.,5.4085294920414,7.48687450672668));
#46445=CARTESIAN_POINT('Ctrl Pts',(-50.,5.51273008511568,7.55694730233435));
#46446=CARTESIAN_POINT('Ctrl Pts',(-50.,5.62104079403545,7.62316036752337));
#46447=CARTESIAN_POINT('Ctrl Pts',(-50.,5.73019939351842,7.68712558947513));
#46448=CARTESIAN_POINT('Ctrl Pts',(-50.,5.83770131742005,7.75010308069958));
#46449=CARTESIAN_POINT('Ctrl Pts',(-50.,5.94287083600227,7.81248225000655));
#46450=CARTESIAN_POINT('Ctrl Pts',(-50.,6.04295375419009,7.86961601478767));
#46451=CARTESIAN_POINT('Ctrl Pts',(-50.,6.12653324054482,7.91133123656149));
#46452=CARTESIAN_POINT('Ctrl Pts',(-50.,6.19209613698591,7.93917015374266));
#46453=CARTESIAN_POINT('Ctrl Pts',(-50.,6.23565680611781,7.9556005638596));
#46454=CARTESIAN_POINT('Ctrl Pts',(-50.,6.25438154632588,7.96230723301849));
#46455=CARTESIAN_POINT('',(-50.5,6.85231494663519,8.12012345177831));
#46456=CARTESIAN_POINT('Ctrl Pts',(-50.5,6.8523149466352,8.12012345177831));
#46457=CARTESIAN_POINT('Ctrl Pts',(-50.493830180584,6.8458214690457,8.11753002104072));
#46458=CARTESIAN_POINT('Ctrl Pts',(-50.4876312970856,6.83917923121437,8.1150220909353));
#46459=CARTESIAN_POINT('Ctrl Pts',(-50.3468664668717,6.68598458219145,8.06000624664622));
#46460=CARTESIAN_POINT('Ctrl Pts',(-50.1957285018887,6.47200684022351,8.04025442110009));
#46461=CARTESIAN_POINT('Ctrl Pts',(-50.,6.25438154632588,7.96230723301849));
#46462=CARTESIAN_POINT('Ctrl Pts',(-65.5,6.85231494663519,8.1201234517783));
#46463=CARTESIAN_POINT('Ctrl Pts',(-60.5,6.85231494663519,8.1201234517783));
#46464=CARTESIAN_POINT('Ctrl Pts',(-55.5,6.85231494663519,8.12012345177831));
#46465=CARTESIAN_POINT('Ctrl Pts',(-50.5,6.85231494663519,8.12012345177831));
#46466=CARTESIAN_POINT('Origin',(-66.,0.,0.));
#46467=CARTESIAN_POINT('',(-50.,3.26473139515386,7.09765349728322));
#46468=CARTESIAN_POINT('',(-66.,3.26473139515386,7.09765349728322));
#46469=CARTESIAN_POINT('Origin',(-50.,0.,0.));
#46470=CARTESIAN_POINT('Ctrl Pts',(-66.,3.42289955803116,10.6903874399214));
#46471=CARTESIAN_POINT('Ctrl Pts',(-50.,3.42289955803116,10.6903874399214));
#46472=CARTESIAN_POINT('Ctrl Pts',(-66.,3.43120048731865,10.6681995504796));
#46473=CARTESIAN_POINT('Ctrl Pts',(-50.,3.43120048731865,10.6681995504796));
#46474=CARTESIAN_POINT('Ctrl Pts',(-66.,3.44758885606022,10.6238259397238));
#46475=CARTESIAN_POINT('Ctrl Pts',(-50.,3.44758885606022,10.6238259397238));
#46476=CARTESIAN_POINT('Ctrl Pts',(-66.,3.47153093969157,10.5572720282296));
#46477=CARTESIAN_POINT('Ctrl Pts',(-50.,3.47153093969157,10.5572720282296));
#46478=CARTESIAN_POINT('Ctrl Pts',(-66.,3.50217107532409,10.4685465039012));
#46479=CARTESIAN_POINT('Ctrl Pts',(-50.,3.50217107532409,10.4685465039012));
#46480=CARTESIAN_POINT('Ctrl Pts',(-66.,3.53832086407721,10.3576635566192));
#46481=CARTESIAN_POINT('Ctrl Pts',(-50.,3.53832086407721,10.3576635566192));
#46482=CARTESIAN_POINT('Ctrl Pts',(-66.,3.57229954809871,10.2468111124749));
#46483=CARTESIAN_POINT('Ctrl Pts',(-50.,3.57229954809871,10.2468111124749));
#46484=CARTESIAN_POINT('Ctrl Pts',(-66.,3.60407872174138,10.1360022269104));
#46485=CARTESIAN_POINT('Ctrl Pts',(-50.,3.60407872174138,10.1360022269104));
#46486=CARTESIAN_POINT('Ctrl Pts',(-66.,3.63362296509257,10.0252584365622));
#46487=CARTESIAN_POINT('Ctrl Pts',(-50.,3.63362296509257,10.0252584365622));
#46488=CARTESIAN_POINT('Ctrl Pts',(-66.,3.66089037006135,9.91461244043035));
#46489=CARTESIAN_POINT('Ctrl Pts',(-50.,3.66089037006135,9.91461244043035));
#46490=CARTESIAN_POINT('Ctrl Pts',(-66.,3.68583503495501,9.80410636044176));
#46491=CARTESIAN_POINT('Ctrl Pts',(-50.,3.68583503495501,9.80410636044176));
#46492=CARTESIAN_POINT('Ctrl Pts',(-66.,3.70840997544632,9.69378895262094));
#46493=CARTESIAN_POINT('Ctrl Pts',(-50.,3.70840997544632,9.69378895262094));
#46494=CARTESIAN_POINT('Ctrl Pts',(-66.,3.72857053198252,9.58371309792272));
#46495=CARTESIAN_POINT('Ctrl Pts',(-50.,3.72857053198252,9.58371309792272));
#46496=CARTESIAN_POINT('Ctrl Pts',(-66.,3.74627697881514,9.47393341091317));
#46497=CARTESIAN_POINT('Ctrl Pts',(-50.,3.74627697881514,9.47393341091317));
#46498=CARTESIAN_POINT('Ctrl Pts',(-66.,3.76149999185445,9.36450320782188));
#46499=CARTESIAN_POINT('Ctrl Pts',(-50.,3.76149999185445,9.36450320782188));
#46500=CARTESIAN_POINT('Ctrl Pts',(-66.,3.77421407729429,9.25547470294892));
#46501=CARTESIAN_POINT('Ctrl Pts',(-50.,3.77421407729429,9.25547470294892));
#46502=CARTESIAN_POINT('Ctrl Pts',(-66.,3.78438491054742,9.14690108386965));
#46503=CARTESIAN_POINT('Ctrl Pts',(-50.,3.78438491054742,9.14690108386965));
#46504=CARTESIAN_POINT('Ctrl Pts',(-66.,3.79195870389943,9.03883763918063));
#46505=CARTESIAN_POINT('Ctrl Pts',(-50.,3.79195870389943,9.03883763918063));
#46506=CARTESIAN_POINT('Ctrl Pts',(-66.,3.79685119396006,8.93134394759486));
#46507=CARTESIAN_POINT('Ctrl Pts',(-50.,3.79685119396006,8.93134394759486));
#46508=CARTESIAN_POINT('Ctrl Pts',(-66.,3.79893629234755,8.82448381898456));
#46509=CARTESIAN_POINT('Ctrl Pts',(-50.,3.79893629234755,8.82448381898456));
#46510=CARTESIAN_POINT('Ctrl Pts',(-66.,3.79803846148212,8.71833378187116));
#46511=CARTESIAN_POINT('Ctrl Pts',(-50.,3.79803846148212,8.71833378187116));
#46512=CARTESIAN_POINT('Ctrl Pts',(-66.,3.79392974119514,8.61299594320168));
#46513=CARTESIAN_POINT('Ctrl Pts',(-50.,3.79392974119514,8.61299594320168));
#46514=CARTESIAN_POINT('Ctrl Pts',(-66.,3.78632231001325,8.50861168112478));
#46515=CARTESIAN_POINT('Ctrl Pts',(-50.,3.78632231001325,8.50861168112478));
#46516=CARTESIAN_POINT('Ctrl Pts',(-66.,3.77486983303976,8.40537048302527));
#46517=CARTESIAN_POINT('Ctrl Pts',(-50.,3.77486983303976,8.40537048302527));
#46518=CARTESIAN_POINT('Ctrl Pts',(-66.,3.75914794626584,8.3035325132631));
#46519=CARTESIAN_POINT('Ctrl Pts',(-50.,3.75914794626584,8.3035325132631));
#46520=CARTESIAN_POINT('Ctrl Pts',(-66.,3.73872358735957,8.20339185905743));
#46521=CARTESIAN_POINT('Ctrl Pts',(-50.,3.73872358735957,8.20339185905743));
#46522=CARTESIAN_POINT('Ctrl Pts',(-66.,3.71327428463273,8.10520575006332));
#46523=CARTESIAN_POINT('Ctrl Pts',(-50.,3.71327428463273,8.10520575006332));
#46524=CARTESIAN_POINT('Ctrl Pts',(-66.,3.68270014530645,8.009130177902));
#46525=CARTESIAN_POINT('Ctrl Pts',(-50.,3.68270014530645,8.009130177902));
#46526=CARTESIAN_POINT('Ctrl Pts',(-66.,3.6472251501756,7.91516027596723));
#46527=CARTESIAN_POINT('Ctrl Pts',(-50.,3.6472251501756,7.91516027596723));
#46528=CARTESIAN_POINT('Ctrl Pts',(-66.,3.60754440881085,7.82304699926879));
#46529=CARTESIAN_POINT('Ctrl Pts',(-50.,3.60754440881085,7.82304699926879));
#46530=CARTESIAN_POINT('Ctrl Pts',(-66.,3.56472003815351,7.73234616270153));
#46531=CARTESIAN_POINT('Ctrl Pts',(-50.,3.56472003815351,7.73234616270153));
#46532=CARTESIAN_POINT('Ctrl Pts',(-66.,3.51998727159863,7.64251498957522));
#46533=CARTESIAN_POINT('Ctrl Pts',(-50.,3.51998727159863,7.64251498957522));
#46534=CARTESIAN_POINT('Ctrl Pts',(-66.,3.47458791282935,7.55299400848973));
#46535=CARTESIAN_POINT('Ctrl Pts',(-50.,3.47458791282935,7.55299400848973));
#46536=CARTESIAN_POINT('Ctrl Pts',(-66.,3.42960116601568,7.46329076114798));
#46537=CARTESIAN_POINT('Ctrl Pts',(-50.,3.42960116601568,7.46329076114798));
#46538=CARTESIAN_POINT('Ctrl Pts',(-66.,3.38575342590423,7.37307334414807));
#46539=CARTESIAN_POINT('Ctrl Pts',(-50.,3.38575342590423,7.37307334414807));
#46540=CARTESIAN_POINT('Ctrl Pts',(-66.,3.34346851534271,7.28214820789157));
#46541=CARTESIAN_POINT('Ctrl Pts',(-50.,3.34346851534271,7.28214820789157));
#46542=CARTESIAN_POINT('Ctrl Pts',(-66.,3.31105697803551,7.20876600436839));
#46543=CARTESIAN_POINT('Ctrl Pts',(-50.,3.31105697803551,7.20876600436839));
#46544=CARTESIAN_POINT('Ctrl Pts',(-66.,3.2875736303622,7.15335511050624));
#46545=CARTESIAN_POINT('Ctrl Pts',(-50.,3.2875736303622,7.15335511050624));
#46546=CARTESIAN_POINT('Ctrl Pts',(-66.,3.27228441642341,7.11624838867044));
#46547=CARTESIAN_POINT('Ctrl Pts',(-50.,3.27228441642341,7.11624838867044));
#46548=CARTESIAN_POINT('Ctrl Pts',(-66.,3.26473139515386,7.09765349728322));
#46549=CARTESIAN_POINT('Ctrl Pts',(-50.,3.26473139515386,7.09765349728322));
#46550=CARTESIAN_POINT('Ctrl Pts',(-50.,3.7558642325485,9.40261181090994));
#46551=CARTESIAN_POINT('Ctrl Pts',(-50.,3.7568962025383,9.39500546428213));
#46552=CARTESIAN_POINT('Ctrl Pts',(-50.,3.76083703923337,9.36553580025944));
#46553=CARTESIAN_POINT('Ctrl Pts',(-50.,3.76730575834657,9.31426214822248));
#46554=CARTESIAN_POINT('Ctrl Pts',(-50.,3.77554083905247,9.24131152455862));
#46555=CARTESIAN_POINT('Ctrl Pts',(-50.,3.78438491054742,9.14690108386965));
#46556=CARTESIAN_POINT('Ctrl Pts',(-50.,3.79195870389943,9.03883763918063));
#46557=CARTESIAN_POINT('Ctrl Pts',(-50.,3.79685119396006,8.93134394759486));
#46558=CARTESIAN_POINT('Ctrl Pts',(-50.,3.79893629234755,8.82448381898456));
#46559=CARTESIAN_POINT('Ctrl Pts',(-50.,3.79803846148212,8.71833378187116));
#46560=CARTESIAN_POINT('Ctrl Pts',(-50.,3.79392974119514,8.61299594320168));
#46561=CARTESIAN_POINT('Ctrl Pts',(-50.,3.78632231001325,8.50861168112478));
#46562=CARTESIAN_POINT('Ctrl Pts',(-50.,3.77486983303976,8.40537048302527));
#46563=CARTESIAN_POINT('Ctrl Pts',(-50.,3.75914794626584,8.3035325132631));
#46564=CARTESIAN_POINT('Ctrl Pts',(-50.,3.73872358735957,8.20339185905743));
#46565=CARTESIAN_POINT('Ctrl Pts',(-50.,3.71327428463273,8.10520575006332));
#46566=CARTESIAN_POINT('Ctrl Pts',(-50.,3.68270014530645,8.009130177902));
#46567=CARTESIAN_POINT('Ctrl Pts',(-50.,3.6472251501756,7.91516027596723));
#46568=CARTESIAN_POINT('Ctrl Pts',(-50.,3.60754440881085,7.82304699926879));
#46569=CARTESIAN_POINT('Ctrl Pts',(-50.,3.56472003815351,7.73234616270153));
#46570=CARTESIAN_POINT('Ctrl Pts',(-50.,3.51998727159863,7.64251498957522));
#46571=CARTESIAN_POINT('Ctrl Pts',(-50.,3.47458791282935,7.55299400848973));
#46572=CARTESIAN_POINT('Ctrl Pts',(-50.,3.42960116601568,7.46329076114798));
#46573=CARTESIAN_POINT('Ctrl Pts',(-50.,3.38575342590423,7.37307334414807));
#46574=CARTESIAN_POINT('Ctrl Pts',(-50.,3.34346851534271,7.28214820789157));
#46575=CARTESIAN_POINT('Ctrl Pts',(-50.,3.31105697803551,7.20876600436839));
#46576=CARTESIAN_POINT('Ctrl Pts',(-50.,3.2875736303622,7.15335511050624));
#46577=CARTESIAN_POINT('Ctrl Pts',(-50.,3.27228441642341,7.11624838867044));
#46578=CARTESIAN_POINT('Ctrl Pts',(-50.,3.26473139515386,7.09765349728322));
#46579=CARTESIAN_POINT('Origin',(-50.,4.32306613303376,8.4660342683367));
#46580=CARTESIAN_POINT('Origin',(-50.,0.,0.));
#46581=CARTESIAN_POINT('Origin',(-65.75,0.,0.));
#46582=CARTESIAN_POINT('',(-65.5,7.38871231397104,7.63528357963034));
#46583=CARTESIAN_POINT('Origin',(-65.5,0.,0.));
#46584=CARTESIAN_POINT('',(-66.,7.25553947328137,7.06206570003818));
#46585=CARTESIAN_POINT('Ctrl Pts',(-65.5,7.38871231397104,7.63528357963033));
#46586=CARTESIAN_POINT('Ctrl Pts',(-65.6642917360006,7.35411196707391,7.44014378288531));
#46587=CARTESIAN_POINT('Ctrl Pts',(-65.8311182354837,7.30991422840986,7.24832985268342));
#46588=CARTESIAN_POINT('Ctrl Pts',(-66.,7.25553947328137,7.06206570003818));
#46589=CARTESIAN_POINT('Origin',(-66.,0.,0.));
#46590=CARTESIAN_POINT('Origin',(-58.,0.,0.));
#46591=CARTESIAN_POINT('',(-50.5,7.38871231397104,7.63528357963034));
#46592=CARTESIAN_POINT('Origin',(-50.5,0.,0.));
#46593=CARTESIAN_POINT('Ctrl Pts',(-50.5,7.38871231397104,7.63528357963034));
#46594=CARTESIAN_POINT('Ctrl Pts',(-55.5,7.38871231397104,7.63528357963034));
#46595=CARTESIAN_POINT('Ctrl Pts',(-60.5,7.38871231397104,7.63528357963034));
#46596=CARTESIAN_POINT('Ctrl Pts',(-65.5,7.38871231397104,7.63528357963034));
#46597=CARTESIAN_POINT('Origin',(-50.25,0.,0.));
#46598=CARTESIAN_POINT('',(-50.,7.25553947328138,7.0620657000382));
#46599=CARTESIAN_POINT('Origin',(-50.,0.,0.));
#46600=CARTESIAN_POINT('Ctrl Pts',(-50.,7.25553947328138,7.0620657000382));
#46601=CARTESIAN_POINT('Ctrl Pts',(-50.1688817645172,7.30991422841014,7.24832985268443));
#46602=CARTESIAN_POINT('Ctrl Pts',(-50.3357082640003,7.35411196707409,7.4401437828864));
#46603=CARTESIAN_POINT('Ctrl Pts',(-50.5,7.38871231397104,7.63528357963035));
#46604=CARTESIAN_POINT('Origin',(-66.,7.39276378738951,5.97575774334076));
#46605=CARTESIAN_POINT('',(-66.,8.9522239671058,4.73004345041105));
#46606=CARTESIAN_POINT('Origin',(-66.,0.,0.));
#46607=CARTESIAN_POINT('',(-66.,5.86935629366619,5.15614322415515));
#46608=CARTESIAN_POINT('Ctrl Pts',(-66.,5.86935629366619,5.15614322415516));
#46609=CARTESIAN_POINT('Ctrl Pts',(-66.,5.88381954563966,5.17005841220104));
#46610=CARTESIAN_POINT('Ctrl Pts',(-66.,5.91287960105941,5.19773840582942));
#46611=CARTESIAN_POINT('Ctrl Pts',(-66.,5.95687034761592,5.23880723822028));
#46612=CARTESIAN_POINT('Ctrl Pts',(-66.,6.01632699142066,5.29266225703943));
#46613=CARTESIAN_POINT('Ctrl Pts',(-66.,6.09193876408314,5.35852767967753));
#46614=CARTESIAN_POINT('Ctrl Pts',(-66.,6.16869039722735,5.42311090855867));
#46615=CARTESIAN_POINT('Ctrl Pts',(-66.,6.24627343312988,5.48676114432161));
#46616=CARTESIAN_POINT('Ctrl Pts',(-66.,6.32415927444501,5.55007704717236));
#46617=CARTESIAN_POINT('Ctrl Pts',(-66.,6.40156231993997,5.61394745203258));
#46618=CARTESIAN_POINT('Ctrl Pts',(-66.,6.47757568301991,5.67938854851998));
#46619=CARTESIAN_POINT('Ctrl Pts',(-66.,6.5512916889966,5.74739860249896));
#46620=CARTESIAN_POINT('Ctrl Pts',(-66.,6.6219207121214,5.81881539913394));
#46621=CARTESIAN_POINT('Ctrl Pts',(-66.,6.68892903392674,5.89414917887782));
#46622=CARTESIAN_POINT('Ctrl Pts',(-66.,6.75211401720195,5.97349548879327));
#46623=CARTESIAN_POINT('Ctrl Pts',(-66.,6.81150347103307,6.0566711933897));
#46624=CARTESIAN_POINT('Ctrl Pts',(-66.,6.86728736323967,6.14331014063223));
#46625=CARTESIAN_POINT('Ctrl Pts',(-66.,6.91974169989968,6.23296752615852));
#46626=CARTESIAN_POINT('Ctrl Pts',(-66.,6.96914833844732,6.3252330736069));
#46627=CARTESIAN_POINT('Ctrl Pts',(-66.,7.0157466000915,6.41979281054442));
#46628=CARTESIAN_POINT('Ctrl Pts',(-66.,7.05974191915822,6.51640051406571));
#46629=CARTESIAN_POINT('Ctrl Pts',(-66.,7.10130101698719,6.61487018507936));
#46630=CARTESIAN_POINT('Ctrl Pts',(-66.,7.14055312818317,6.71506051373632));
#46631=CARTESIAN_POINT('Ctrl Pts',(-66.,7.17758748640133,6.81686192205253));
#46632=CARTESIAN_POINT('Ctrl Pts',(-66.,7.2079082107772,6.90670735924895));
#46633=CARTESIAN_POINT('Ctrl Pts',(-66.,7.23005678198432,6.97670057921104));
#46634=CARTESIAN_POINT('Ctrl Pts',(-66.,7.24500218612944,7.02617245622325));
#46635=CARTESIAN_POINT('Ctrl Pts',(-66.,7.25338844488451,7.05469721661769));
#46636=CARTESIAN_POINT('Ctrl Pts',(-66.,7.25553947328137,7.06206570003819));
#46637=CARTESIAN_POINT('',(-66.,6.71751445306827,3.98875366785402));
#46638=CARTESIAN_POINT('Origin',(-66.,0.,0.));
#46639=CARTESIAN_POINT('Ctrl Pts',(-66.,8.9522239671058,4.73004345041105));
#46640=CARTESIAN_POINT('Ctrl Pts',(-66.,8.93239021764327,4.73153264123973));
#46641=CARTESIAN_POINT('Ctrl Pts',(-66.,8.88591271637064,4.73424043504303));
#46642=CARTESIAN_POINT('Ctrl Pts',(-66.,8.81469492241586,4.73547515111526));
#46643=CARTESIAN_POINT('Ctrl Pts',(-66.,8.72137415303495,4.73136123945916));
#46644=CARTESIAN_POINT('Ctrl Pts',(-66.,8.6067054620435,4.7198743383383));
#46645=CARTESIAN_POINT('Ctrl Pts',(-66.,8.48525643213848,4.70566442850842));
#46646=CARTESIAN_POINT('Ctrl Pts',(-66.,8.36143328450034,4.69185659911854));
#46647=CARTESIAN_POINT('Ctrl Pts',(-66.,8.23569494212978,4.67782026347397));
#46648=CARTESIAN_POINT('Ctrl Pts',(-66.,8.10981690611934,4.66138555268912));
#46649=CARTESIAN_POINT('Ctrl Pts',(-66.,7.98612375397626,4.63975306799096));
#46650=CARTESIAN_POINT('Ctrl Pts',(-66.,7.86637497053616,4.61080556997054));
#46651=CARTESIAN_POINT('Ctrl Pts',(-66.,7.75120579898901,4.57378192723342));
#46652=CARTESIAN_POINT('Ctrl Pts',(-66.,7.6405197035065,4.52886501948474));
#46653=CARTESIAN_POINT('Ctrl Pts',(-66.,7.53368133093183,4.476993833765));
#46654=CARTESIAN_POINT('Ctrl Pts',(-66.,7.42979527874749,4.41958894930823));
#46655=CARTESIAN_POINT('Ctrl Pts',(-66.,7.32791448753526,4.35832808183351));
#46656=CARTESIAN_POINT('Ctrl Pts',(-66.,7.22711161240614,4.29494540516727));
#46657=CARTESIAN_POINT('Ctrl Pts',(-66.,7.12656402515112,4.23103749131175));
#46658=CARTESIAN_POINT('Ctrl Pts',(-66.,7.02563860180952,4.1678561402315));
#46659=CARTESIAN_POINT('Ctrl Pts',(-66.,6.92396448304503,4.10613397949206));
#46660=CARTESIAN_POINT('Ctrl Pts',(-66.,6.84187937648697,4.05821392716855));
#46661=CARTESIAN_POINT('Ctrl Pts',(-66.,6.77986998456097,4.02314530770572));
#46662=CARTESIAN_POINT('Ctrl Pts',(-66.,6.73833259489066,4.00015307569533));
#46663=CARTESIAN_POINT('Ctrl Pts',(-66.,6.71751445306827,3.98875366785402));
#46664=CARTESIAN_POINT('Ctrl Pts',(-66.,6.71751445306827,3.98875366785402));
#46665=CARTESIAN_POINT('Ctrl Pts',(-50.,6.71751445306827,3.98875366785402));
#46666=CARTESIAN_POINT('Ctrl Pts',(-66.,6.73833259489066,4.00015307569533));
#46667=CARTESIAN_POINT('Ctrl Pts',(-50.,6.73833259489066,4.00015307569533));
#46668=CARTESIAN_POINT('Ctrl Pts',(-66.,6.77986998456097,4.02314530770572));
#46669=CARTESIAN_POINT('Ctrl Pts',(-50.,6.77986998456097,4.02314530770572));
#46670=CARTESIAN_POINT('Ctrl Pts',(-66.,6.84187937648697,4.05821392716855));
#46671=CARTESIAN_POINT('Ctrl Pts',(-50.,6.84187937648697,4.05821392716855));
#46672=CARTESIAN_POINT('Ctrl Pts',(-66.,6.92396448304503,4.10613397949206));
#46673=CARTESIAN_POINT('Ctrl Pts',(-50.,6.92396448304503,4.10613397949206));
#46674=CARTESIAN_POINT('Ctrl Pts',(-66.,7.02563860180952,4.1678561402315));
#46675=CARTESIAN_POINT('Ctrl Pts',(-50.,7.02563860180952,4.1678561402315));
#46676=CARTESIAN_POINT('Ctrl Pts',(-66.,7.12656402515112,4.23103749131175));
#46677=CARTESIAN_POINT('Ctrl Pts',(-50.,7.12656402515112,4.23103749131175));
#46678=CARTESIAN_POINT('Ctrl Pts',(-66.,7.22711161240614,4.29494540516727));
#46679=CARTESIAN_POINT('Ctrl Pts',(-50.,7.22711161240614,4.29494540516727));
#46680=CARTESIAN_POINT('Ctrl Pts',(-66.,7.32791448753526,4.35832808183351));
#46681=CARTESIAN_POINT('Ctrl Pts',(-50.,7.32791448753526,4.35832808183351));
#46682=CARTESIAN_POINT('Ctrl Pts',(-66.,7.42979527874749,4.41958894930823));
#46683=CARTESIAN_POINT('Ctrl Pts',(-50.,7.42979527874749,4.41958894930823));
#46684=CARTESIAN_POINT('Ctrl Pts',(-66.,7.53368133093183,4.476993833765));
#46685=CARTESIAN_POINT('Ctrl Pts',(-50.,7.53368133093183,4.476993833765));
#46686=CARTESIAN_POINT('Ctrl Pts',(-66.,7.6405197035065,4.52886501948474));
#46687=CARTESIAN_POINT('Ctrl Pts',(-50.,7.6405197035065,4.52886501948474));
#46688=CARTESIAN_POINT('Ctrl Pts',(-66.,7.75120579898901,4.57378192723342));
#46689=CARTESIAN_POINT('Ctrl Pts',(-50.,7.75120579898901,4.57378192723342));
#46690=CARTESIAN_POINT('Ctrl Pts',(-66.,7.86637497053616,4.61080556997054));
#46691=CARTESIAN_POINT('Ctrl Pts',(-50.,7.86637497053616,4.61080556997054));
#46692=CARTESIAN_POINT('Ctrl Pts',(-66.,7.98612375397626,4.63975306799096));
#46693=CARTESIAN_POINT('Ctrl Pts',(-50.,7.98612375397626,4.63975306799096));
#46694=CARTESIAN_POINT('Ctrl Pts',(-66.,8.10981690611934,4.66138555268912));
#46695=CARTESIAN_POINT('Ctrl Pts',(-50.,8.10981690611934,4.66138555268912));
#46696=CARTESIAN_POINT('Ctrl Pts',(-66.,8.23569494212978,4.67782026347397));
#46697=CARTESIAN_POINT('Ctrl Pts',(-50.,8.23569494212978,4.67782026347397));
#46698=CARTESIAN_POINT('Ctrl Pts',(-66.,8.36143328450034,4.69185659911854));
#46699=CARTESIAN_POINT('Ctrl Pts',(-50.,8.36143328450034,4.69185659911854));
#46700=CARTESIAN_POINT('Ctrl Pts',(-66.,8.48525643213848,4.70566442850842));
#46701=CARTESIAN_POINT('Ctrl Pts',(-50.,8.48525643213848,4.70566442850842));
#46702=CARTESIAN_POINT('Ctrl Pts',(-66.,8.6067054620435,4.7198743383383));
#46703=CARTESIAN_POINT('Ctrl Pts',(-50.,8.6067054620435,4.7198743383383));
#46704=CARTESIAN_POINT('Ctrl Pts',(-66.,8.72796083967823,4.73202105878326));
#46705=CARTESIAN_POINT('Ctrl Pts',(-50.,8.72796083967823,4.73202105878326));
#46706=CARTESIAN_POINT('Ctrl Pts',(-66.,8.85339313547798,4.73705510013294));
#46707=CARTESIAN_POINT('Ctrl Pts',(-50.,8.85339313547798,4.73705510013294));
#46708=CARTESIAN_POINT('Ctrl Pts',(-66.,8.98705564961503,4.7302562506624));
#46709=CARTESIAN_POINT('Ctrl Pts',(-50.,8.98705564961503,4.7302562506624));
#46710=CARTESIAN_POINT('Ctrl Pts',(-66.,9.13083440990634,4.70938113162593));
#46711=CARTESIAN_POINT('Ctrl Pts',(-50.,9.13083440990634,4.70938113162593));
#46712=CARTESIAN_POINT('Ctrl Pts',(-66.,9.28205231015641,4.67744454272398));
#46713=CARTESIAN_POINT('Ctrl Pts',(-50.,9.28205231015641,4.67744454272398));
#46714=CARTESIAN_POINT('Ctrl Pts',(-66.,9.43209170831184,4.64432174792964));
#46715=CARTESIAN_POINT('Ctrl Pts',(-50.,9.43209170831184,4.64432174792964));
#46716=CARTESIAN_POINT('Ctrl Pts',(-66.,9.56884308464813,4.62392482004402));
#46717=CARTESIAN_POINT('Ctrl Pts',(-50.,9.56884308464813,4.62392482004402));
#46718=CARTESIAN_POINT('Ctrl Pts',(-66.,9.6786259001787,4.63198987040163));
#46719=CARTESIAN_POINT('Ctrl Pts',(-50.,9.6786259001787,4.63198987040163));
#46720=CARTESIAN_POINT('Ctrl Pts',(-66.,9.74822876312235,4.68372599634944));
#46721=CARTESIAN_POINT('Ctrl Pts',(-50.,9.74822876312235,4.68372599634944));
#46722=CARTESIAN_POINT('Ctrl Pts',(-66.,9.7670979254493,4.79129438302231));
#46723=CARTESIAN_POINT('Ctrl Pts',(-50.,9.7670979254493,4.79129438302231));
#46724=CARTESIAN_POINT('Ctrl Pts',(-66.,9.72722453283275,4.96393510772457));
#46725=CARTESIAN_POINT('Ctrl Pts',(-50.,9.72722453283275,4.96393510772457));
#46726=CARTESIAN_POINT('Ctrl Pts',(-66.,9.62270607610076,5.20846913094059));
#46727=CARTESIAN_POINT('Ctrl Pts',(-50.,9.62270607610076,5.20846913094059));
#46728=CARTESIAN_POINT('Ctrl Pts',(-66.,9.4494426466907,5.52964537209809));
#46729=CARTESIAN_POINT('Ctrl Pts',(-50.,9.4494426466907,5.52964537209809));
#46730=CARTESIAN_POINT('Ctrl Pts',(-66.,9.20479447534083,5.93053256419968));
#46731=CARTESIAN_POINT('Ctrl Pts',(-50.,9.20479447534083,5.93053256419968));
#46732=CARTESIAN_POINT('Ctrl Pts',(-66.,8.88727303370654,6.41287268812632));
#46733=CARTESIAN_POINT('Ctrl Pts',(-50.,8.88727303370654,6.41287268812632));
#46734=CARTESIAN_POINT('Ctrl Pts',(-66.,8.49623316568549,6.97743341853195));
#46735=CARTESIAN_POINT('Ctrl Pts',(-50.,8.49623316568549,6.97743341853195));
#46736=CARTESIAN_POINT('Ctrl Pts',(-66.,8.12450963002148,7.49496283424254));
#46737=CARTESIAN_POINT('Ctrl Pts',(-50.,8.12450963002148,7.49496283424254));
#46738=CARTESIAN_POINT('Ctrl Pts',(-66.,7.81266471007362,7.92008819074951));
#46739=CARTESIAN_POINT('Ctrl Pts',(-50.,7.81266471007362,7.92008819074951));
#46740=CARTESIAN_POINT('Ctrl Pts',(-66.,7.59009772798531,8.21991804475996));
#46741=CARTESIAN_POINT('Ctrl Pts',(-50.,7.59009772798531,8.21991804475996));
#46742=CARTESIAN_POINT('Ctrl Pts',(-66.,7.47514664369958,8.37393621036051));
#46743=CARTESIAN_POINT('Ctrl Pts',(-50.,7.47514664369958,8.37393621036051));
#46744=CARTESIAN_POINT('',(-65.5,9.56265294797246,4.6310143161767));
#46745=CARTESIAN_POINT('Ctrl Pts',(-66.,8.9522239671058,4.73004345041105));
#46746=CARTESIAN_POINT('Ctrl Pts',(-65.7982417703063,9.18983991158661,4.71220237170136));
#46747=CARTESIAN_POINT('Ctrl Pts',(-65.6331946192803,9.4118184657459,4.63688451531894));
#46748=CARTESIAN_POINT('Ctrl Pts',(-65.5,9.56265294797246,4.6310143161767));
#46749=CARTESIAN_POINT('',(-50.,6.71751445306827,3.98875366785402));
#46750=CARTESIAN_POINT('',(-66.,6.71751445306827,3.98875366785402));
#46751=CARTESIAN_POINT('',(-50.,8.95222396710582,4.73004345041105));
#46752=CARTESIAN_POINT('Ctrl Pts',(-50.,6.71751445306827,3.98875366785402));
#46753=CARTESIAN_POINT('Ctrl Pts',(-50.,6.73833259489066,4.00015307569533));
#46754=CARTESIAN_POINT('Ctrl Pts',(-50.,6.77986998456097,4.02314530770572));
#46755=CARTESIAN_POINT('Ctrl Pts',(-50.,6.84187937648697,4.05821392716855));
#46756=CARTESIAN_POINT('Ctrl Pts',(-50.,6.92396448304503,4.10613397949206));
#46757=CARTESIAN_POINT('Ctrl Pts',(-50.,7.02563860180952,4.1678561402315));
#46758=CARTESIAN_POINT('Ctrl Pts',(-50.,7.12656402515112,4.23103749131175));
#46759=CARTESIAN_POINT('Ctrl Pts',(-50.,7.22711161240614,4.29494540516727));
#46760=CARTESIAN_POINT('Ctrl Pts',(-50.,7.32791448753526,4.35832808183351));
#46761=CARTESIAN_POINT('Ctrl Pts',(-50.,7.42979527874749,4.41958894930823));
#46762=CARTESIAN_POINT('Ctrl Pts',(-50.,7.53368133093183,4.476993833765));
#46763=CARTESIAN_POINT('Ctrl Pts',(-50.,7.6405197035065,4.52886501948474));
#46764=CARTESIAN_POINT('Ctrl Pts',(-50.,7.75120579898901,4.57378192723342));
#46765=CARTESIAN_POINT('Ctrl Pts',(-50.,7.86637497053616,4.61080556997054));
#46766=CARTESIAN_POINT('Ctrl Pts',(-50.,7.98612375397626,4.63975306799096));
#46767=CARTESIAN_POINT('Ctrl Pts',(-50.,8.10981690611934,4.66138555268912));
#46768=CARTESIAN_POINT('Ctrl Pts',(-50.,8.23569494212978,4.67782026347397));
#46769=CARTESIAN_POINT('Ctrl Pts',(-50.,8.36143328450034,4.69185659911854));
#46770=CARTESIAN_POINT('Ctrl Pts',(-50.,8.48525643213848,4.70566442850842));
#46771=CARTESIAN_POINT('Ctrl Pts',(-50.,8.6067054620435,4.7198743383383));
#46772=CARTESIAN_POINT('Ctrl Pts',(-50.,8.72137415303496,4.73136123945916));
#46773=CARTESIAN_POINT('Ctrl Pts',(-50.,8.81469492241586,4.73547515111526));
#46774=CARTESIAN_POINT('Ctrl Pts',(-50.,8.88591271637065,4.73424043504303));
#46775=CARTESIAN_POINT('Ctrl Pts',(-50.,8.93239021764329,4.73153264123973));
#46776=CARTESIAN_POINT('Ctrl Pts',(-50.,8.95222396710582,4.73004345041105));
#46777=CARTESIAN_POINT('',(-50.5,9.56265294797246,4.6310143161767));
#46778=CARTESIAN_POINT('Ctrl Pts',(-50.5,9.56265294797247,4.6310143161767));
#46779=CARTESIAN_POINT('Ctrl Pts',(-50.4982567069791,9.56067877888363,4.63109114718723));
#46780=CARTESIAN_POINT('Ctrl Pts',(-50.4965113438742,9.55869681884698,4.63117903647081));
#46781=CARTESIAN_POINT('Ctrl Pts',(-50.3581212730752,9.40112969752826,4.63898530076718));
#46782=CARTESIAN_POINT('Ctrl Pts',(-50.2022201285446,9.19038390194521,4.71216152690525));
#46783=CARTESIAN_POINT('Ctrl Pts',(-50.,8.95222396710582,4.73004345041105));
#46784=CARTESIAN_POINT('Ctrl Pts',(-65.5,9.56265294797246,4.6310143161767));
#46785=CARTESIAN_POINT('Ctrl Pts',(-60.5,9.56265294797246,4.6310143161767));
#46786=CARTESIAN_POINT('Ctrl Pts',(-55.5,9.56265294797246,4.6310143161767));
#46787=CARTESIAN_POINT('Ctrl Pts',(-50.5,9.56265294797246,4.6310143161767));
#46788=CARTESIAN_POINT('Origin',(-66.,0.,0.));
#46789=CARTESIAN_POINT('',(-50.,5.86935629366619,5.15614322415515));
#46790=CARTESIAN_POINT('',(-66.,5.86935629366619,5.15614322415515));
#46791=CARTESIAN_POINT('Origin',(-50.,0.,0.));
#46792=CARTESIAN_POINT('Ctrl Pts',(-66.,7.47514664369958,8.37393621036051));
#46793=CARTESIAN_POINT('Ctrl Pts',(-50.,7.47514664369958,8.37393621036051));
#46794=CARTESIAN_POINT('Ctrl Pts',(-66.,7.47370529227588,8.35029027263347));
#46795=CARTESIAN_POINT('Ctrl Pts',(-50.,7.47370529227588,8.35029027263347));
#46796=CARTESIAN_POINT('Ctrl Pts',(-66.,7.47062843861794,8.30308721200087));
#46797=CARTESIAN_POINT('Ctrl Pts',(-50.,7.47062843861794,8.30308721200087));
#46798=CARTESIAN_POINT('Ctrl Pts',(-66.,7.46543070582113,8.2325490657425));
#46799=CARTESIAN_POINT('Ctrl Pts',(-50.,7.46543070582113,8.2325490657425));
#46800=CARTESIAN_POINT('Ctrl Pts',(-66.,7.45733394062932,8.13903180010481));
#46801=CARTESIAN_POINT('Ctrl Pts',(-50.,7.45733394062932,8.13903180010481));
#46802=CARTESIAN_POINT('Ctrl Pts',(-66.,7.44525825818761,8.02303174355991));
#46803=CARTESIAN_POINT('Ctrl Pts',(-50.,7.44525825818761,8.02303174355991));
#46804=CARTESIAN_POINT('Ctrl Pts',(-66.,7.43121157962414,7.90794262086832));
#46805=CARTESIAN_POINT('Ctrl Pts',(-50.,7.43121157962414,7.90794262086832));
#46806=CARTESIAN_POINT('Ctrl Pts',(-66.,7.41517326521556,7.79378791238727));
#46807=CARTESIAN_POINT('Ctrl Pts',(-50.,7.41517326521556,7.79378791238727));
#46808=CARTESIAN_POINT('Ctrl Pts',(-66.,7.39711971700079,7.68060169938963));
#46809=CARTESIAN_POINT('Ctrl Pts',(-50.,7.39711971700079,7.68060169938963));
#46810=CARTESIAN_POINT('Ctrl Pts',(-66.,7.3770259499153,7.56843089945469));
#46811=CARTESIAN_POINT('Ctrl Pts',(-50.,7.3770259499153,7.56843089945469));
#46812=CARTESIAN_POINT('Ctrl Pts',(-66.,7.35486716320729,7.45733266277773));
#46813=CARTESIAN_POINT('Ctrl Pts',(-50.,7.35486716320729,7.45733266277773));
#46814=CARTESIAN_POINT('Ctrl Pts',(-66.,7.33062026541981,7.34737064045104));
#46815=CARTESIAN_POINT('Ctrl Pts',(-50.,7.33062026541981,7.34737064045104));
#46816=CARTESIAN_POINT('Ctrl Pts',(-66.,7.30426596664335,7.23861130630728));
#46817=CARTESIAN_POINT('Ctrl Pts',(-50.,7.30426596664335,7.23861130630728));
#46818=CARTESIAN_POINT('Ctrl Pts',(-66.,7.27579018934611,7.13112071115277));
#46819=CARTESIAN_POINT('Ctrl Pts',(-50.,7.27579018934611,7.13112071115277));
#46820=CARTESIAN_POINT('Ctrl Pts',(-66.,7.24518783030335,7.02495948896872));
#46821=CARTESIAN_POINT('Ctrl Pts',(-50.,7.24518783030335,7.02495948896872));
#46822=CARTESIAN_POINT('Ctrl Pts',(-66.,7.21245683723339,6.92018570915688));
#46823=CARTESIAN_POINT('Ctrl Pts',(-50.,7.21245683723339,6.92018570915688));
#46824=CARTESIAN_POINT('Ctrl Pts',(-66.,7.17758748640133,6.81686192205253));
#46825=CARTESIAN_POINT('Ctrl Pts',(-50.,7.17758748640133,6.81686192205253));
#46826=CARTESIAN_POINT('Ctrl Pts',(-66.,7.14055312818317,6.71506051373632));
#46827=CARTESIAN_POINT('Ctrl Pts',(-50.,7.14055312818317,6.71506051373632));
#46828=CARTESIAN_POINT('Ctrl Pts',(-66.,7.10130101698719,6.61487018507936));
#46829=CARTESIAN_POINT('Ctrl Pts',(-50.,7.10130101698719,6.61487018507936));
#46830=CARTESIAN_POINT('Ctrl Pts',(-66.,7.05974191915822,6.51640051406571));
#46831=CARTESIAN_POINT('Ctrl Pts',(-50.,7.05974191915822,6.51640051406571));
#46832=CARTESIAN_POINT('Ctrl Pts',(-66.,7.0157466000915,6.41979281054442));
#46833=CARTESIAN_POINT('Ctrl Pts',(-50.,7.0157466000915,6.41979281054442));
#46834=CARTESIAN_POINT('Ctrl Pts',(-66.,6.96914833844732,6.3252330736069));
#46835=CARTESIAN_POINT('Ctrl Pts',(-50.,6.96914833844732,6.3252330736069));
#46836=CARTESIAN_POINT('Ctrl Pts',(-66.,6.91974169989968,6.23296752615852));
#46837=CARTESIAN_POINT('Ctrl Pts',(-50.,6.91974169989968,6.23296752615852));
#46838=CARTESIAN_POINT('Ctrl Pts',(-66.,6.86728736323967,6.14331014063223));
#46839=CARTESIAN_POINT('Ctrl Pts',(-50.,6.86728736323967,6.14331014063223));
#46840=CARTESIAN_POINT('Ctrl Pts',(-66.,6.81150347103307,6.0566711933897));
#46841=CARTESIAN_POINT('Ctrl Pts',(-50.,6.81150347103307,6.0566711933897));
#46842=CARTESIAN_POINT('Ctrl Pts',(-66.,6.75211401720195,5.97349548879327));
#46843=CARTESIAN_POINT('Ctrl Pts',(-50.,6.75211401720195,5.97349548879327));
#46844=CARTESIAN_POINT('Ctrl Pts',(-66.,6.68892903392674,5.89414917887782));
#46845=CARTESIAN_POINT('Ctrl Pts',(-50.,6.68892903392674,5.89414917887782));
#46846=CARTESIAN_POINT('Ctrl Pts',(-66.,6.6219207121214,5.81881539913394));
#46847=CARTESIAN_POINT('Ctrl Pts',(-50.,6.6219207121214,5.81881539913394));
#46848=CARTESIAN_POINT('Ctrl Pts',(-66.,6.5512916889966,5.74739860249896));
#46849=CARTESIAN_POINT('Ctrl Pts',(-50.,6.5512916889966,5.74739860249896));
#46850=CARTESIAN_POINT('Ctrl Pts',(-66.,6.47757568301991,5.67938854851998));
#46851=CARTESIAN_POINT('Ctrl Pts',(-50.,6.47757568301991,5.67938854851998));
#46852=CARTESIAN_POINT('Ctrl Pts',(-66.,6.40156231993997,5.61394745203258));
#46853=CARTESIAN_POINT('Ctrl Pts',(-50.,6.40156231993997,5.61394745203258));
#46854=CARTESIAN_POINT('Ctrl Pts',(-66.,6.32415927444501,5.55007704717236));
#46855=CARTESIAN_POINT('Ctrl Pts',(-50.,6.32415927444501,5.55007704717236));
#46856=CARTESIAN_POINT('Ctrl Pts',(-66.,6.24627343312988,5.48676114432161));
#46857=CARTESIAN_POINT('Ctrl Pts',(-50.,6.24627343312988,5.48676114432161));
#46858=CARTESIAN_POINT('Ctrl Pts',(-66.,6.16869039722735,5.42311090855867));
#46859=CARTESIAN_POINT('Ctrl Pts',(-50.,6.16869039722735,5.42311090855867));
#46860=CARTESIAN_POINT('Ctrl Pts',(-66.,6.09193876408314,5.35852767967753));
#46861=CARTESIAN_POINT('Ctrl Pts',(-50.,6.09193876408314,5.35852767967753));
#46862=CARTESIAN_POINT('Ctrl Pts',(-66.,6.01632699142066,5.29266225703943));
#46863=CARTESIAN_POINT('Ctrl Pts',(-50.,6.01632699142066,5.29266225703943));
#46864=CARTESIAN_POINT('Ctrl Pts',(-66.,5.95687034761592,5.23880723822028));
#46865=CARTESIAN_POINT('Ctrl Pts',(-50.,5.95687034761592,5.23880723822028));
#46866=CARTESIAN_POINT('Ctrl Pts',(-66.,5.91287960105941,5.19773840582942));
#46867=CARTESIAN_POINT('Ctrl Pts',(-50.,5.91287960105941,5.19773840582942));
#46868=CARTESIAN_POINT('Ctrl Pts',(-66.,5.88381954563966,5.17005841220104));
#46869=CARTESIAN_POINT('Ctrl Pts',(-50.,5.88381954563966,5.17005841220104));
#46870=CARTESIAN_POINT('Ctrl Pts',(-66.,5.86935629366619,5.15614322415516));
#46871=CARTESIAN_POINT('Ctrl Pts',(-50.,5.86935629366619,5.15614322415516));
#46872=CARTESIAN_POINT('Ctrl Pts',(-50.,7.25553947328138,7.0620657000382));
#46873=CARTESIAN_POINT('Ctrl Pts',(-50.,7.25338844488451,7.0546972166177));
#46874=CARTESIAN_POINT('Ctrl Pts',(-50.,7.24500218612945,7.02617245622326));
#46875=CARTESIAN_POINT('Ctrl Pts',(-50.,7.23005678198432,6.97670057921104));
#46876=CARTESIAN_POINT('Ctrl Pts',(-50.,7.2079082107772,6.90670735924896));
#46877=CARTESIAN_POINT('Ctrl Pts',(-50.,7.17758748640133,6.81686192205253));
#46878=CARTESIAN_POINT('Ctrl Pts',(-50.,7.14055312818317,6.71506051373632));
#46879=CARTESIAN_POINT('Ctrl Pts',(-50.,7.10130101698719,6.61487018507936));
#46880=CARTESIAN_POINT('Ctrl Pts',(-50.,7.05974191915822,6.51640051406571));
#46881=CARTESIAN_POINT('Ctrl Pts',(-50.,7.0157466000915,6.41979281054442));
#46882=CARTESIAN_POINT('Ctrl Pts',(-50.,6.96914833844732,6.3252330736069));
#46883=CARTESIAN_POINT('Ctrl Pts',(-50.,6.91974169989968,6.23296752615852));
#46884=CARTESIAN_POINT('Ctrl Pts',(-50.,6.86728736323967,6.14331014063223));
#46885=CARTESIAN_POINT('Ctrl Pts',(-50.,6.81150347103307,6.0566711933897));
#46886=CARTESIAN_POINT('Ctrl Pts',(-50.,6.75211401720195,5.97349548879327));
#46887=CARTESIAN_POINT('Ctrl Pts',(-50.,6.68892903392674,5.89414917887782));
#46888=CARTESIAN_POINT('Ctrl Pts',(-50.,6.6219207121214,5.81881539913394));
#46889=CARTESIAN_POINT('Ctrl Pts',(-50.,6.5512916889966,5.74739860249896));
#46890=CARTESIAN_POINT('Ctrl Pts',(-50.,6.47757568301991,5.67938854851998));
#46891=CARTESIAN_POINT('Ctrl Pts',(-50.,6.40156231993997,5.61394745203258));
#46892=CARTESIAN_POINT('Ctrl Pts',(-50.,6.32415927444501,5.55007704717236));
#46893=CARTESIAN_POINT('Ctrl Pts',(-50.,6.24627343312988,5.48676114432161));
#46894=CARTESIAN_POINT('Ctrl Pts',(-50.,6.16869039722735,5.42311090855867));
#46895=CARTESIAN_POINT('Ctrl Pts',(-50.,6.09193876408314,5.35852767967753));
#46896=CARTESIAN_POINT('Ctrl Pts',(-50.,6.01632699142066,5.29266225703943));
#46897=CARTESIAN_POINT('Ctrl Pts',(-50.,5.95687034761592,5.23880723822028));
#46898=CARTESIAN_POINT('Ctrl Pts',(-50.,5.91287960105941,5.19773840582942));
#46899=CARTESIAN_POINT('Ctrl Pts',(-50.,5.88381954563966,5.17005841220104));
#46900=CARTESIAN_POINT('Ctrl Pts',(-50.,5.86935629366619,5.15614322415516));
#46901=CARTESIAN_POINT('Origin',(-50.,7.39276378738951,5.97575774334076));
#46902=CARTESIAN_POINT('Origin',(-50.,0.,0.));
#46903=CARTESIAN_POINT('Origin',(-65.75,0.,0.));
#46904=CARTESIAN_POINT('',(-65.5,9.85547418436682,3.96991858874703));
#46905=CARTESIAN_POINT('Origin',(-65.5,0.,0.));
#46906=CARTESIAN_POINT('',(-66.,9.50066602457707,3.50042427277708));
#46907=CARTESIAN_POINT('Ctrl Pts',(-65.5,9.85547418436681,3.96991858874702));
#46908=CARTESIAN_POINT('Ctrl Pts',(-65.6642917360003,9.74449468876773,3.80572274277181));
#46909=CARTESIAN_POINT('Ctrl Pts',(-65.8311182354839,9.62610029130724,3.64846883797855));
#46910=CARTESIAN_POINT('Ctrl Pts',(-66.,9.50066602457707,3.50042427277707));
#46911=CARTESIAN_POINT('Origin',(-66.,0.,0.));
#46912=CARTESIAN_POINT('Origin',(-58.,0.,0.));
#46913=CARTESIAN_POINT('',(-50.5,9.85547418436682,3.96991858874703));
#46914=CARTESIAN_POINT('Origin',(-50.5,0.,0.));
#46915=CARTESIAN_POINT('Ctrl Pts',(-50.5,9.85547418436682,3.96991858874703));
#46916=CARTESIAN_POINT('Ctrl Pts',(-55.5,9.85547418436682,3.96991858874703));
#46917=CARTESIAN_POINT('Ctrl Pts',(-60.5,9.85547418436682,3.96991858874703));
#46918=CARTESIAN_POINT('Ctrl Pts',(-65.5,9.85547418436682,3.96991858874703));
#46919=CARTESIAN_POINT('Origin',(-50.25,0.,0.));
#46920=CARTESIAN_POINT('',(-50.,9.50066602457708,3.50042427277709));
#46921=CARTESIAN_POINT('Origin',(-50.,0.,0.));
#46922=CARTESIAN_POINT('Ctrl Pts',(-50.,9.50066602457708,3.50042427277709));
#46923=CARTESIAN_POINT('Ctrl Pts',(-50.1688817645154,9.62610029130675,3.64846883797794));
#46924=CARTESIAN_POINT('Ctrl Pts',(-50.335708263999,9.74449468876727,3.80572274277114));
#46925=CARTESIAN_POINT('Ctrl Pts',(-50.5,9.85547418436682,3.96991858874704));
#46926=CARTESIAN_POINT('Ctrl Pts',(-66.,10.234872965097,4.60955533520604));
#46927=CARTESIAN_POINT('Ctrl Pts',(-50.,10.234872965097,4.60955533520604));
#46928=CARTESIAN_POINT('Ctrl Pts',(-66.,10.2239385557175,4.58853994664336));
#46929=CARTESIAN_POINT('Ctrl Pts',(-50.,10.2239385557175,4.58853994664336));
#46930=CARTESIAN_POINT('Ctrl Pts',(-66.,10.2019284956099,4.54666927414369));
#46931=CARTESIAN_POINT('Ctrl Pts',(-50.,10.2019284956099,4.54666927414369));
#46932=CARTESIAN_POINT('Ctrl Pts',(-66.,10.1684896816054,4.48434357942821));
#46933=CARTESIAN_POINT('Ctrl Pts',(-50.,10.1684896816054,4.48434357942821));
#46934=CARTESIAN_POINT('Ctrl Pts',(-66.,10.1230560198477,4.40220455728764));
#46935=CARTESIAN_POINT('Ctrl Pts',(-50.,10.1230560198477,4.40220455728764));
#46936=CARTESIAN_POINT('Ctrl Pts',(-66.,10.0648428614095,4.30114485508394));
#46937=CARTESIAN_POINT('Ctrl Pts',(-50.,10.0648428614095,4.30114485508394));
#46938=CARTESIAN_POINT('Ctrl Pts',(-66.,10.0051996185948,4.20171900871024));
#46939=CARTESIAN_POINT('Ctrl Pts',(-50.,10.0051996185948,4.20171900871024));
#46940=CARTESIAN_POINT('Ctrl Pts',(-66.,9.94411698639968,4.103956863472));
#46941=CARTESIAN_POINT('Ctrl Pts',(-50.,9.94411698639968,4.103956863472));
#46942=CARTESIAN_POINT('Ctrl Pts',(-66.,9.88158726911661,4.00789915231672));
#46943=CARTESIAN_POINT('Ctrl Pts',(-50.,9.88158726911661,4.00789915231672));
#46944=CARTESIAN_POINT('Ctrl Pts',(-66.,9.81760672485207,3.91359889892712));
#46945=CARTESIAN_POINT('Ctrl Pts',(-50.,9.81760672485207,3.91359889892712));
#46946=CARTESIAN_POINT('Ctrl Pts',(-66.,9.75217594207047,3.82111839997903));
#46947=CARTESIAN_POINT('Ctrl Pts',(-50.,9.75217594207047,3.82111839997903));
#46948=CARTESIAN_POINT('Ctrl Pts',(-66.,9.68529971490782,3.73052519578036));
#46949=CARTESIAN_POINT('Ctrl Pts',(-50.,9.68529971490782,3.73052519578036));
#46950=CARTESIAN_POINT('Ctrl Pts',(-66.,9.61698745849843,3.64188785911205));
#46951=CARTESIAN_POINT('Ctrl Pts',(-50.,9.61698745849843,3.64188785911205));
#46952=CARTESIAN_POINT('Ctrl Pts',(-66.,9.54725317766033,3.55527245623621));
#46953=CARTESIAN_POINT('Ctrl Pts',(-50.,9.54725317766033,3.55527245623621));
#46954=CARTESIAN_POINT('Ctrl Pts',(-66.,9.4761168724277,3.47073645471943));
#46955=CARTESIAN_POINT('Ctrl Pts',(-50.,9.4761168724277,3.47073645471943));
#46956=CARTESIAN_POINT('Ctrl Pts',(-66.,9.40360028690147,3.3883337383381));
#46957=CARTESIAN_POINT('Ctrl Pts',(-50.,9.40360028690147,3.3883337383381));
#46958=CARTESIAN_POINT('Ctrl Pts',(-66.,9.3297199795212,3.30812540466615));
#46959=CARTESIAN_POINT('Ctrl Pts',(-50.,9.3297199795212,3.30812540466615));
#46960=CARTESIAN_POINT('Ctrl Pts',(-66.,9.25448104671536,3.23018842105738));
#46961=CARTESIAN_POINT('Ctrl Pts',(-50.,9.25448104671536,3.23018842105738));
#46962=CARTESIAN_POINT('Ctrl Pts',(-66.,9.17787138088281,3.15462527335458));
#46963=CARTESIAN_POINT('Ctrl Pts',(-50.,9.17787138088281,3.15462527335458));
#46964=CARTESIAN_POINT('Ctrl Pts',(-66.,9.09985403240456,3.08157236062471));
#46965=CARTESIAN_POINT('Ctrl Pts',(-50.,9.09985403240456,3.08157236062471));
#46966=CARTESIAN_POINT('Ctrl Pts',(-66.,9.0203684154881,3.01121134028781));
#46967=CARTESIAN_POINT('Ctrl Pts',(-50.,9.0203684154881,3.01121134028781));
#46968=CARTESIAN_POINT('Ctrl Pts',(-66.,8.93933787525693,2.94377994264697));
#46969=CARTESIAN_POINT('Ctrl Pts',(-50.,8.93933787525693,2.94377994264697));
#46970=CARTESIAN_POINT('Ctrl Pts',(-66.,8.85667488599363,2.87958666118713));
#46971=CARTESIAN_POINT('Ctrl Pts',(-50.,8.85667488599363,2.87958666118713));
#46972=CARTESIAN_POINT('Ctrl Pts',(-66.,8.7722885209883,2.81901566470334));
#46973=CARTESIAN_POINT('Ctrl Pts',(-50.,8.7722885209883,2.81901566470334));
#46974=CARTESIAN_POINT('Ctrl Pts',(-66.,8.68608816509229,2.7625564010488));
#46975=CARTESIAN_POINT('Ctrl Pts',(-50.,8.68608816509229,2.7625564010488));
#46976=CARTESIAN_POINT('Ctrl Pts',(-66.,8.59800259243998,2.71072748101388));
#46977=CARTESIAN_POINT('Ctrl Pts',(-50.,8.59800259243998,2.71072748101388));
#46978=CARTESIAN_POINT('Ctrl Pts',(-66.,8.50800718624223,2.66394066800009));
#46979=CARTESIAN_POINT('Ctrl Pts',(-50.,8.50800718624223,2.66394066800009));
#46980=CARTESIAN_POINT('Ctrl Pts',(-66.,8.41615102954947,2.62237457557726));
#46981=CARTESIAN_POINT('Ctrl Pts',(-50.,8.41615102954947,2.62237457557726));
#46982=CARTESIAN_POINT('Ctrl Pts',(-66.,8.32258037817354,2.58585949718149));
#46983=CARTESIAN_POINT('Ctrl Pts',(-50.,8.32258037817354,2.58585949718149));
#46984=CARTESIAN_POINT('Ctrl Pts',(-66.,8.22757527470717,2.55371222210688));
#46985=CARTESIAN_POINT('Ctrl Pts',(-50.,8.22757527470717,2.55371222210688));
#46986=CARTESIAN_POINT('Ctrl Pts',(-66.,8.13151632024086,2.52484622579571));
#46987=CARTESIAN_POINT('Ctrl Pts',(-50.,8.13151632024086,2.52484622579571));
#46988=CARTESIAN_POINT('Ctrl Pts',(-66.,8.0348266855565,2.49798036244632));
#46989=CARTESIAN_POINT('Ctrl Pts',(-50.,8.0348266855565,2.49798036244632));
#46990=CARTESIAN_POINT('Ctrl Pts',(-66.,7.93792153122956,2.47181743264013));
#46991=CARTESIAN_POINT('Ctrl Pts',(-50.,7.93792153122956,2.47181743264013));
#46992=CARTESIAN_POINT('Ctrl Pts',(-66.,7.84115701796548,2.44522591246363));
#46993=CARTESIAN_POINT('Ctrl Pts',(-50.,7.84115701796548,2.44522591246363));
#46994=CARTESIAN_POINT('Ctrl Pts',(-66.,7.74477254642582,2.41744389869504));
#46995=CARTESIAN_POINT('Ctrl Pts',(-50.,7.74477254642582,2.41744389869504));
#46996=CARTESIAN_POINT('Ctrl Pts',(-66.,7.64890787406712,2.38802691961804));
#46997=CARTESIAN_POINT('Ctrl Pts',(-50.,7.64890787406712,2.38802691961804));
#46998=CARTESIAN_POINT('Ctrl Pts',(-66.,7.57268671762535,2.36301110751424));
#46999=CARTESIAN_POINT('Ctrl Pts',(-50.,7.57268671762535,2.36301110751424));
#47000=CARTESIAN_POINT('Ctrl Pts',(-66.,7.51579497190863,2.34338551081368));
#47001=CARTESIAN_POINT('Ctrl Pts',(-50.,7.51579497190863,2.34338551081368));
#47002=CARTESIAN_POINT('Ctrl Pts',(-66.,7.47798882259232,2.32991836775593));
#47003=CARTESIAN_POINT('Ctrl Pts',(-50.,7.47798882259232,2.32991836775593));
#47004=CARTESIAN_POINT('Ctrl Pts',(-66.,7.45911616757566,2.32308894548001));
#47005=CARTESIAN_POINT('Ctrl Pts',(-50.,7.45911616757566,2.32308894548001));
#47006=CARTESIAN_POINT('',(-50.,7.45911616757566,2.32308894548));
#47007=CARTESIAN_POINT('Ctrl Pts',(-50.,9.50066602457708,3.50042427277709));
#47008=CARTESIAN_POINT('Ctrl Pts',(-50.,9.49570393014485,3.49456773028788));
#47009=CARTESIAN_POINT('Ctrl Pts',(-50.,9.47644063626517,3.47192006373319));
#47010=CARTESIAN_POINT('Ctrl Pts',(-50.,9.44266530501315,3.43280409871903));
#47011=CARTESIAN_POINT('Ctrl Pts',(-50.,9.39396277106816,3.37787074605859));
#47012=CARTESIAN_POINT('Ctrl Pts',(-50.,9.3297199795212,3.30812540466615));
#47013=CARTESIAN_POINT('Ctrl Pts',(-50.,9.25448104671536,3.23018842105738));
#47014=CARTESIAN_POINT('Ctrl Pts',(-50.,9.17787138088281,3.15462527335458));
#47015=CARTESIAN_POINT('Ctrl Pts',(-50.,9.09985403240456,3.08157236062471));
#47016=CARTESIAN_POINT('Ctrl Pts',(-50.,9.0203684154881,3.01121134028781));
#47017=CARTESIAN_POINT('Ctrl Pts',(-50.,8.93933787525693,2.94377994264697));
#47018=CARTESIAN_POINT('Ctrl Pts',(-50.,8.85667488599363,2.87958666118713));
#47019=CARTESIAN_POINT('Ctrl Pts',(-50.,8.7722885209883,2.81901566470334));
#47020=CARTESIAN_POINT('Ctrl Pts',(-50.,8.68608816509229,2.7625564010488));
#47021=CARTESIAN_POINT('Ctrl Pts',(-50.,8.59800259243998,2.71072748101388));
#47022=CARTESIAN_POINT('Ctrl Pts',(-50.,8.50800718624223,2.66394066800009));
#47023=CARTESIAN_POINT('Ctrl Pts',(-50.,8.41615102954947,2.62237457557726));
#47024=CARTESIAN_POINT('Ctrl Pts',(-50.,8.32258037817354,2.58585949718149));
#47025=CARTESIAN_POINT('Ctrl Pts',(-50.,8.22757527470717,2.55371222210688));
#47026=CARTESIAN_POINT('Ctrl Pts',(-50.,8.13151632024086,2.52484622579571));
#47027=CARTESIAN_POINT('Ctrl Pts',(-50.,8.0348266855565,2.49798036244632));
#47028=CARTESIAN_POINT('Ctrl Pts',(-50.,7.93792153122956,2.47181743264013));
#47029=CARTESIAN_POINT('Ctrl Pts',(-50.,7.84115701796548,2.44522591246363));
#47030=CARTESIAN_POINT('Ctrl Pts',(-50.,7.74477254642582,2.41744389869504));
#47031=CARTESIAN_POINT('Ctrl Pts',(-50.,7.64890787406712,2.38802691961804));
#47032=CARTESIAN_POINT('Ctrl Pts',(-50.,7.57268671762535,2.36301110751424));
#47033=CARTESIAN_POINT('Ctrl Pts',(-50.,7.51579497190863,2.34338551081368));
#47034=CARTESIAN_POINT('Ctrl Pts',(-50.,7.47798882259232,2.32991836775593));
#47035=CARTESIAN_POINT('Ctrl Pts',(-50.,7.45911616757566,2.32308894548001));
#47036=CARTESIAN_POINT('',(-66.,7.45911616757566,2.32308894548));
#47037=CARTESIAN_POINT('',(-66.,7.45911616757566,2.32308894548));
#47038=CARTESIAN_POINT('Ctrl Pts',(-66.,7.45911616757566,2.32308894548001));
#47039=CARTESIAN_POINT('Ctrl Pts',(-66.,7.47798882259232,2.32991836775593));
#47040=CARTESIAN_POINT('Ctrl Pts',(-66.,7.51579497190863,2.34338551081368));
#47041=CARTESIAN_POINT('Ctrl Pts',(-66.,7.57268671762535,2.36301110751424));
#47042=CARTESIAN_POINT('Ctrl Pts',(-66.,7.64890787406712,2.38802691961804));
#47043=CARTESIAN_POINT('Ctrl Pts',(-66.,7.74477254642582,2.41744389869504));
#47044=CARTESIAN_POINT('Ctrl Pts',(-66.,7.84115701796548,2.44522591246363));
#47045=CARTESIAN_POINT('Ctrl Pts',(-66.,7.93792153122956,2.47181743264013));
#47046=CARTESIAN_POINT('Ctrl Pts',(-66.,8.0348266855565,2.49798036244632));
#47047=CARTESIAN_POINT('Ctrl Pts',(-66.,8.13151632024086,2.52484622579571));
#47048=CARTESIAN_POINT('Ctrl Pts',(-66.,8.22757527470717,2.55371222210688));
#47049=CARTESIAN_POINT('Ctrl Pts',(-66.,8.32258037817354,2.58585949718149));
#47050=CARTESIAN_POINT('Ctrl Pts',(-66.,8.41615102954947,2.62237457557726));
#47051=CARTESIAN_POINT('Ctrl Pts',(-66.,8.50800718624223,2.66394066800009));
#47052=CARTESIAN_POINT('Ctrl Pts',(-66.,8.59800259243998,2.71072748101388));
#47053=CARTESIAN_POINT('Ctrl Pts',(-66.,8.68608816509229,2.7625564010488));
#47054=CARTESIAN_POINT('Ctrl Pts',(-66.,8.7722885209883,2.81901566470334));
#47055=CARTESIAN_POINT('Ctrl Pts',(-66.,8.85667488599363,2.87958666118713));
#47056=CARTESIAN_POINT('Ctrl Pts',(-66.,8.93933787525693,2.94377994264697));
#47057=CARTESIAN_POINT('Ctrl Pts',(-66.,9.0203684154881,3.01121134028781));
#47058=CARTESIAN_POINT('Ctrl Pts',(-66.,9.09985403240456,3.08157236062471));
#47059=CARTESIAN_POINT('Ctrl Pts',(-66.,9.17787138088281,3.15462527335458));
#47060=CARTESIAN_POINT('Ctrl Pts',(-66.,9.25448104671536,3.23018842105738));
#47061=CARTESIAN_POINT('Ctrl Pts',(-66.,9.3297199795212,3.30812540466615));
#47062=CARTESIAN_POINT('Ctrl Pts',(-66.,9.39396277106816,3.37787074605859));
#47063=CARTESIAN_POINT('Ctrl Pts',(-66.,9.44266530501315,3.43280409871902));
#47064=CARTESIAN_POINT('Ctrl Pts',(-66.,9.47644063626516,3.47192006373319));
#47065=CARTESIAN_POINT('Ctrl Pts',(-66.,9.49570393014484,3.49456773028787));
#47066=CARTESIAN_POINT('Ctrl Pts',(-66.,9.50066602457707,3.50042427277708));
#47067=CARTESIAN_POINT('Origin',(-66.,9.18418542175504,2.4522184164664));
#47068=CARTESIAN_POINT('Origin',(-66.,0.,0.));
#47069=CARTESIAN_POINT('',(-66.,7.75912709216827,0.911648516469146));
#47070=CARTESIAN_POINT('Origin',(-66.,0.,0.));
#47071=CARTESIAN_POINT('Ctrl Pts',(-66.,10.1021455355716,0.67991218413181));
#47072=CARTESIAN_POINT('Ctrl Pts',(-66.,10.0846322123206,0.689339740324907));
#47073=CARTESIAN_POINT('Ctrl Pts',(-66.,10.0432742611121,0.710717535900336));
#47074=CARTESIAN_POINT('Ctrl Pts',(-66.,9.97871577321179,0.740812391600032));
#47075=CARTESIAN_POINT('Ctrl Pts',(-66.,9.89178972962324,0.775011122760695));
#47076=CARTESIAN_POINT('Ctrl Pts',(-66.,9.78236252423293,0.811157274859099));
#47077=CARTESIAN_POINT('Ctrl Pts',(-66.,9.66563362360549,0.847573647008884));
#47078=CARTESIAN_POINT('Ctrl Pts',(-66.,9.54689939935545,0.885322978595271));
#47079=CARTESIAN_POINT('Ctrl Pts',(-66.,9.42632261579016,0.923642539206944));
#47080=CARTESIAN_POINT('Ctrl Pts',(-66.,9.3046427086813,0.959827893625642));
#47081=CARTESIAN_POINT('Ctrl Pts',(-66.,9.18284466719198,0.990376172966252));
#47082=CARTESIAN_POINT('Ctrl Pts',(-66.,9.06167470185178,1.01263753582842));
#47083=CARTESIAN_POINT('Ctrl Pts',(-66.,8.94140355616308,1.02565827740144));
#47084=CARTESIAN_POINT('Ctrl Pts',(-66.,8.8220174241358,1.02964473126801));
#47085=CARTESIAN_POINT('Ctrl Pts',(-66.,8.70331780221627,1.02571312618391));
#47086=CARTESIAN_POINT('Ctrl Pts',(-66.,8.58506450113074,1.01552541886979));
#47087=CARTESIAN_POINT('Ctrl Pts',(-66.,8.4670747275092,1.00099948266857));
#47088=CARTESIAN_POINT('Ctrl Pts',(-66.,8.34920666168128,0.984096749349312));
#47089=CARTESIAN_POINT('Ctrl Pts',(-66.,8.23135817971997,0.966610353048665));
#47090=CARTESIAN_POINT('Ctrl Pts',(-66.,8.11346004702223,0.949941384652545));
#47091=CARTESIAN_POINT('Ctrl Pts',(-66.,7.99547145320256,0.934909974827099));
#47092=CARTESIAN_POINT('Ctrl Pts',(-66.,7.90099213574826,0.924519849384913));
#47093=CARTESIAN_POINT('Ctrl Pts',(-66.,7.83008004486546,0.917704563279999));
#47094=CARTESIAN_POINT('Ctrl Pts',(-66.,7.7827819679451,0.913594892602471));
#47095=CARTESIAN_POINT('Ctrl Pts',(-66.,7.75912709216827,0.911648516469146));
#47096=CARTESIAN_POINT('Origin',(-66.,0.,0.));
#47097=CARTESIAN_POINT('',(-50.,7.75912709216827,0.911648516469146));
#47098=CARTESIAN_POINT('Origin',(-50.,0.,0.));
#47099=CARTESIAN_POINT('',(-66.,7.75912709216827,0.911648516469146));
#47100=CARTESIAN_POINT('Ctrl Pts',(-66.,7.75912709216827,0.911648516469146));
#47101=CARTESIAN_POINT('Ctrl Pts',(-50.,7.75912709216827,0.911648516469146));
#47102=CARTESIAN_POINT('Ctrl Pts',(-66.,7.7827819679451,0.913594892602471));
#47103=CARTESIAN_POINT('Ctrl Pts',(-50.,7.7827819679451,0.913594892602471));
#47104=CARTESIAN_POINT('Ctrl Pts',(-66.,7.83008004486546,0.917704563279999));
#47105=CARTESIAN_POINT('Ctrl Pts',(-50.,7.83008004486546,0.917704563279999));
#47106=CARTESIAN_POINT('Ctrl Pts',(-66.,7.90099213574826,0.924519849384913));
#47107=CARTESIAN_POINT('Ctrl Pts',(-50.,7.90099213574826,0.924519849384913));
#47108=CARTESIAN_POINT('Ctrl Pts',(-66.,7.99547145320256,0.934909974827099));
#47109=CARTESIAN_POINT('Ctrl Pts',(-50.,7.99547145320256,0.934909974827099));
#47110=CARTESIAN_POINT('Ctrl Pts',(-66.,8.11346004702223,0.949941384652545));
#47111=CARTESIAN_POINT('Ctrl Pts',(-50.,8.11346004702223,0.949941384652545));
#47112=CARTESIAN_POINT('Ctrl Pts',(-66.,8.23135817971997,0.966610353048665));
#47113=CARTESIAN_POINT('Ctrl Pts',(-50.,8.23135817971997,0.966610353048665));
#47114=CARTESIAN_POINT('Ctrl Pts',(-66.,8.34920666168128,0.984096749349312));
#47115=CARTESIAN_POINT('Ctrl Pts',(-50.,8.34920666168128,0.984096749349312));
#47116=CARTESIAN_POINT('Ctrl Pts',(-66.,8.4670747275092,1.00099948266857));
#47117=CARTESIAN_POINT('Ctrl Pts',(-50.,8.4670747275092,1.00099948266857));
#47118=CARTESIAN_POINT('Ctrl Pts',(-66.,8.58506450113074,1.01552541886979));
#47119=CARTESIAN_POINT('Ctrl Pts',(-50.,8.58506450113074,1.01552541886979));
#47120=CARTESIAN_POINT('Ctrl Pts',(-66.,8.70331780221627,1.02571312618391));
#47121=CARTESIAN_POINT('Ctrl Pts',(-50.,8.70331780221627,1.02571312618391));
#47122=CARTESIAN_POINT('Ctrl Pts',(-66.,8.8220174241358,1.02964473126801));
#47123=CARTESIAN_POINT('Ctrl Pts',(-50.,8.8220174241358,1.02964473126801));
#47124=CARTESIAN_POINT('Ctrl Pts',(-66.,8.94140355616308,1.02565827740144));
#47125=CARTESIAN_POINT('Ctrl Pts',(-50.,8.94140355616308,1.02565827740144));
#47126=CARTESIAN_POINT('Ctrl Pts',(-66.,9.06167470185178,1.01263753582842));
#47127=CARTESIAN_POINT('Ctrl Pts',(-50.,9.06167470185178,1.01263753582842));
#47128=CARTESIAN_POINT('Ctrl Pts',(-66.,9.18284466719198,0.990376172966252));
#47129=CARTESIAN_POINT('Ctrl Pts',(-50.,9.18284466719198,0.990376172966252));
#47130=CARTESIAN_POINT('Ctrl Pts',(-66.,9.3046427086813,0.959827893625642));
#47131=CARTESIAN_POINT('Ctrl Pts',(-50.,9.3046427086813,0.959827893625642));
#47132=CARTESIAN_POINT('Ctrl Pts',(-66.,9.42632261579016,0.923642539206944));
#47133=CARTESIAN_POINT('Ctrl Pts',(-50.,9.42632261579016,0.923642539206944));
#47134=CARTESIAN_POINT('Ctrl Pts',(-66.,9.54689939935545,0.885322978595271));
#47135=CARTESIAN_POINT('Ctrl Pts',(-50.,9.54689939935545,0.885322978595271));
#47136=CARTESIAN_POINT('Ctrl Pts',(-66.,9.66563362360549,0.847573647008884));
#47137=CARTESIAN_POINT('Ctrl Pts',(-50.,9.66563362360549,0.847573647008884));
#47138=CARTESIAN_POINT('Ctrl Pts',(-66.,9.78236252423293,0.811157274859099));
#47139=CARTESIAN_POINT('Ctrl Pts',(-50.,9.78236252423293,0.811157274859099));
#47140=CARTESIAN_POINT('Ctrl Pts',(-66.,9.89807533998404,0.772934850892815));
#47141=CARTESIAN_POINT('Ctrl Pts',(-50.,9.89807533998404,0.772934850892815));
#47142=CARTESIAN_POINT('Ctrl Pts',(-66.,10.0147109731333,0.726515765574518));
#47143=CARTESIAN_POINT('Ctrl Pts',(-50.,10.0147109731333,0.726515765574518));
#47144=CARTESIAN_POINT('Ctrl Pts',(-66.,10.1340524145698,0.665939265218336));
#47145=CARTESIAN_POINT('Ctrl Pts',(-50.,10.1340524145698,0.665939265218336));
#47146=CARTESIAN_POINT('Ctrl Pts',(-66.,10.2569101720987,0.588388804738333));
#47147=CARTESIAN_POINT('Ctrl Pts',(-50.,10.2569101720987,0.588388804738333));
#47148=CARTESIAN_POINT('Ctrl Pts',(-66.,10.3820648170252,0.497707417893672));
#47149=CARTESIAN_POINT('Ctrl Pts',(-50.,10.3820648170252,0.497707417893672));
#47150=CARTESIAN_POINT('Ctrl Pts',(-66.,10.5056603733136,0.406421718030022));
#47151=CARTESIAN_POINT('Ctrl Pts',(-50.,10.5056603733136,0.406421718030022));
#47152=CARTESIAN_POINT('Ctrl Pts',(-66.,10.6222927940147,0.332166401463227));
#47153=CARTESIAN_POINT('Ctrl Pts',(-50.,10.6222927940147,0.332166401463227));
#47154=CARTESIAN_POINT('Ctrl Pts',(-66.,10.7258647379785,0.294881497726767));
#47155=CARTESIAN_POINT('Ctrl Pts',(-50.,10.7258647379785,0.294881497726767));
#47156=CARTESIAN_POINT('Ctrl Pts',(-66.,10.8104930954534,0.313834765760248));
#47157=CARTESIAN_POINT('Ctrl Pts',(-50.,10.8104930954534,0.313834765760248));
#47158=CARTESIAN_POINT('Ctrl Pts',(-66.,10.8714829374831,0.404428597048679));
#47159=CARTESIAN_POINT('Ctrl Pts',(-50.,10.8714829374831,0.404428597048679));
#47160=CARTESIAN_POINT('Ctrl Pts',(-66.,10.905276089601,0.578361716765453));
#47161=CARTESIAN_POINT('Ctrl Pts',(-50.,10.905276089601,0.578361716765453));
#47162=CARTESIAN_POINT('Ctrl Pts',(-66.,10.9092546759344,0.844266149144153));
#47163=CARTESIAN_POINT('Ctrl Pts',(-50.,10.9092546759344,0.844266149144153));
#47164=CARTESIAN_POINT('Ctrl Pts',(-66.,10.8816048031854,1.20814783100236));
#47165=CARTESIAN_POINT('Ctrl Pts',(-50.,10.8816048031854,1.20814783100236));
#47166=CARTESIAN_POINT('Ctrl Pts',(-66.,10.8211630882956,1.67388388032334));
#47167=CARTESIAN_POINT('Ctrl Pts',(-50.,10.8211630882956,1.67388388032334));
#47168=CARTESIAN_POINT('Ctrl Pts',(-66.,10.7272782204132,2.24367111485021));
#47169=CARTESIAN_POINT('Ctrl Pts',(-50.,10.7272782204132,2.24367111485021));
#47170=CARTESIAN_POINT('Ctrl Pts',(-66.,10.599673061523,2.91847324890335));
#47171=CARTESIAN_POINT('Ctrl Pts',(-50.,10.599673061523,2.91847324890335));
#47172=CARTESIAN_POINT('Ctrl Pts',(-66.,10.4705848912574,3.54245347887044));
#47173=CARTESIAN_POINT('Ctrl Pts',(-50.,10.4705848912574,3.54245347887044));
#47174=CARTESIAN_POINT('Ctrl Pts',(-66.,10.3586144415421,4.05766357313591));
#47175=CARTESIAN_POINT('Ctrl Pts',(-50.,10.3586144415421,4.05766357313591));
#47176=CARTESIAN_POINT('Ctrl Pts',(-66.,10.2772411743483,4.42209792148691));
#47177=CARTESIAN_POINT('Ctrl Pts',(-50.,10.2772411743483,4.42209792148691));
#47178=CARTESIAN_POINT('Ctrl Pts',(-66.,10.234872965097,4.60955533520604));
#47179=CARTESIAN_POINT('Ctrl Pts',(-50.,10.234872965097,4.60955533520604));
#47180=CARTESIAN_POINT('',(-50.5,10.6195213806306,0.341160733863857));
#47181=CARTESIAN_POINT('',(-50.,10.1021455355716,0.679912184131802));
#47182=CARTESIAN_POINT('Ctrl Pts',(-50.5,10.6195213806306,0.34116073386385));
#47183=CARTESIAN_POINT('Ctrl Pts',(-50.4982567069816,10.6177491374168,0.342033889391285));
#47184=CARTESIAN_POINT('Ctrl Pts',(-50.4965113438794,10.6159742746229,0.342920316017751));
#47185=CARTESIAN_POINT('Ctrl Pts',(-50.3581212730818,10.4752046404048,0.414140015287625));
#47186=CARTESIAN_POINT('Ctrl Pts',(-50.2022201285479,10.3124422287015,0.566707861725606));
#47187=CARTESIAN_POINT('Ctrl Pts',(-50.,10.1021455355716,0.679912184131803));
#47188=CARTESIAN_POINT('Ctrl Pts',(-65.5,10.6195213806306,0.341160733863858));
#47189=CARTESIAN_POINT('Ctrl Pts',(-60.5,10.6195213806306,0.341160733863858));
#47190=CARTESIAN_POINT('Ctrl Pts',(-55.5,10.6195213806306,0.341160733863856));
#47191=CARTESIAN_POINT('Ctrl Pts',(-50.5,10.6195213806306,0.341160733863856));
#47192=CARTESIAN_POINT('Ctrl Pts',(-50.,7.75912709216827,0.911648516469146));
#47193=CARTESIAN_POINT('Ctrl Pts',(-50.,7.7827819679451,0.913594892602471));
#47194=CARTESIAN_POINT('Ctrl Pts',(-50.,7.83008004486546,0.917704563279999));
#47195=CARTESIAN_POINT('Ctrl Pts',(-50.,7.90099213574826,0.924519849384913));
#47196=CARTESIAN_POINT('Ctrl Pts',(-50.,7.99547145320256,0.934909974827099));
#47197=CARTESIAN_POINT('Ctrl Pts',(-50.,8.11346004702223,0.949941384652545));
#47198=CARTESIAN_POINT('Ctrl Pts',(-50.,8.23135817971997,0.966610353048665));
#47199=CARTESIAN_POINT('Ctrl Pts',(-50.,8.34920666168128,0.984096749349312));
#47200=CARTESIAN_POINT('Ctrl Pts',(-50.,8.4670747275092,1.00099948266857));
#47201=CARTESIAN_POINT('Ctrl Pts',(-50.,8.58506450113074,1.01552541886979));
#47202=CARTESIAN_POINT('Ctrl Pts',(-50.,8.70331780221627,1.02571312618391));
#47203=CARTESIAN_POINT('Ctrl Pts',(-50.,8.8220174241358,1.02964473126801));
#47204=CARTESIAN_POINT('Ctrl Pts',(-50.,8.94140355616308,1.02565827740144));
#47205=CARTESIAN_POINT('Ctrl Pts',(-50.,9.06167470185178,1.01263753582842));
#47206=CARTESIAN_POINT('Ctrl Pts',(-50.,9.18284466719198,0.990376172966252));
#47207=CARTESIAN_POINT('Ctrl Pts',(-50.,9.3046427086813,0.959827893625642));
#47208=CARTESIAN_POINT('Ctrl Pts',(-50.,9.42632261579016,0.923642539206944));
#47209=CARTESIAN_POINT('Ctrl Pts',(-50.,9.54689939935545,0.885322978595271));
#47210=CARTESIAN_POINT('Ctrl Pts',(-50.,9.66563362360549,0.847573647008884));
#47211=CARTESIAN_POINT('Ctrl Pts',(-50.,9.78236252423293,0.811157274859099));
#47212=CARTESIAN_POINT('Ctrl Pts',(-50.,9.89178972962325,0.775011122760694));
#47213=CARTESIAN_POINT('Ctrl Pts',(-50.,9.9787157732118,0.74081239160003));
#47214=CARTESIAN_POINT('Ctrl Pts',(-50.,10.0432742611121,0.710717535900332));
#47215=CARTESIAN_POINT('Ctrl Pts',(-50.,10.0846322123207,0.689339740324902));
#47216=CARTESIAN_POINT('Ctrl Pts',(-50.,10.1021455355716,0.679912184131802));
#47217=CARTESIAN_POINT('Origin',(-50.,9.18418542175504,2.4522184164664));
#47218=CARTESIAN_POINT('Origin',(-50.,0.,0.));
#47219=CARTESIAN_POINT('Origin',(-50.25,0.,0.));
#47220=CARTESIAN_POINT('Origin',(-50.5,0.,0.));
#47221=CARTESIAN_POINT('Origin',(-50.,0.,0.));
#47222=CARTESIAN_POINT('Origin',(-58.,0.,0.));
#47223=CARTESIAN_POINT('Origin',(-110.,6.,0.));
#47224=CARTESIAN_POINT('',(-110.,-6.,-7.34788079488411E-16));
#47225=CARTESIAN_POINT('Origin',(-110.,0.,0.));
#47226=CARTESIAN_POINT('Origin',(-109.5,0.,0.));
#47227=CARTESIAN_POINT('',(-109.5,-6.5,-7.96020419445779E-16));
#47228=CARTESIAN_POINT('Origin',(-66.25,0.,0.));
#47229=CARTESIAN_POINT('',(-66.25,-8.5625,-1.04860382176992E-15));
#47230=CARTESIAN_POINT('Origin',(-49.75,0.,0.));
#47231=CARTESIAN_POINT('',(-49.75,-8.5625,-1.04860382176992E-15));
#47232=CARTESIAN_POINT('Origin',(29.75,0.,0.));
#47233=CARTESIAN_POINT('Origin',(109.067,0.,0.));
#47234=CARTESIAN_POINT('Origin',(109.5,0.,0.));
#47235=CARTESIAN_POINT('',(110.,-6.,-7.34788079488411E-16));
#47236=CARTESIAN_POINT('Origin',(110.,0.,0.));
#47237=CARTESIAN_POINT('',(109.5,-6.5,-7.96020419445779E-16));
#47238=CARTESIAN_POINT('Origin',(110.,0.,0.));
#47239=CARTESIAN_POINT('',(0.,0.,0.));
#47240=CARTESIAN_POINT('Origin',(-6.70710678118655,-22.7688383542068,29.1327993848858));
#47241=CARTESIAN_POINT('',(-6.70710678118655,-30.1934595566656,22.4152849636136));
#47242=CARTESIAN_POINT('',(-6.35355339059327,-30.0899061660723,22.3117315730203));
#47243=CARTESIAN_POINT('Origin',(-6.70710678118655,-29.8399061660723,22.0617315730203));
#47244=CARTESIAN_POINT('',(-6.35355339059327,-22.3117315730203,30.0899061660723));
#47245=CARTESIAN_POINT('',(-6.35355339059327,-23.0188383542068,29.3827993848858));
#47246=CARTESIAN_POINT('',(-6.70710678118655,-22.4152849636136,30.1934595566656));
#47247=CARTESIAN_POINT('Origin',(-6.70710678118655,-22.0617315730203,29.8399061660723));
#47248=CARTESIAN_POINT('',(-6.70710678118655,-23.1223917448001,29.486352775479));
#47249=CARTESIAN_POINT('Origin',(-6.70710678118654,-22.0617315730203,29.8399061660723));
#47250=CARTESIAN_POINT('',(-6.35355339059327,-21.8117315730203,30.0899061660723));
#47251=CARTESIAN_POINT('',(-6.70710678118655,-21.708178182427,30.1934595566656));
#47252=CARTESIAN_POINT('Origin',(-6.70710678118655,-22.0617315730203,29.8399061660723));
#47253=CARTESIAN_POINT('Origin',(-6.70710678118654,-22.0617315730203,29.8399061660723));
#47254=CARTESIAN_POINT('Origin',(-6.70710678118654,-22.0617315730203,29.8399061660723));
#47255=CARTESIAN_POINT('Origin',(-5.04640452079103,-27.4913185063573,22.0617315730203));
#47256=CARTESIAN_POINT('',(-6.14644660940673,-29.7970129472589,21.8117315730203));
#47257=CARTESIAN_POINT('',(-6.14644660940673,-29.7970129472589,22.3117315730203));
#47258=CARTESIAN_POINT('Origin',(-6.5,-29.5470129472589,22.0617315730203));
#47259=CARTESIAN_POINT('',(-4.69285113019775,-27.7413185063573,22.3117315730203));
#47260=CARTESIAN_POINT('',(-6.35355339059327,-30.0899061660723,21.8117315730203));
#47261=CARTESIAN_POINT('Origin',(-6.70710678118654,-29.8399061660723,22.0617315730203));
#47262=CARTESIAN_POINT('',(-4.69285113019775,-27.7413185063573,21.8117315730203));
#47263=CARTESIAN_POINT('Origin',(-6.5,-28.4029896810001,20.9177083067616));
#47264=CARTESIAN_POINT('',(-6.14644660940673,-26.4129509039023,18.4276695296637));
#47265=CARTESIAN_POINT('',(-6.,-26.1629509039023,18.6776695296637));
#47266=CARTESIAN_POINT('Origin',(-6.5,-26.1629509039023,18.6776695296637));
#47267=CARTESIAN_POINT('',(-6.,-29.5470129472589,22.0617315730203));
#47268=CARTESIAN_POINT('',(-6.,-28.4029896810001,20.9177083067616));
#47269=CARTESIAN_POINT('Origin',(-6.5,-29.5470129472589,22.0617315730203));
#47270=CARTESIAN_POINT('',(-6.14644660940673,-28.6529896810001,20.6677083067616));
#47271=CARTESIAN_POINT('Origin',(-6.5,-29.5470129472589,22.0617315730203));
#47272=CARTESIAN_POINT('Origin',(-6.5,-29.5470129472589,22.0617315730203));
#47273=CARTESIAN_POINT('Origin',(-6.70710678118655,-18.3847763108502,26.1629509039023));
#47274=CARTESIAN_POINT('',(-6.35355339059327,-18.1347763108502,26.4129509039023));
#47275=CARTESIAN_POINT('',(-6.70710678118655,-18.031222920257,26.5165042944955));
#47276=CARTESIAN_POINT('Origin',(-6.70710678118655,-18.3847763108502,26.1629509039023));
#47277=CARTESIAN_POINT('',(-6.35355339059327,-18.1347763108502,25.9129509039023));
#47278=CARTESIAN_POINT('Origin',(-6.70710678118655,-18.3847763108502,26.1629509039023));
#47279=CARTESIAN_POINT('',(-6.70710678118655,-18.031222920257,25.809397513309));
#47280=CARTESIAN_POINT('Origin',(-6.70710678118655,-18.3847763108502,26.1629509039023));
#47281=CARTESIAN_POINT('Origin',(-6.70710678118655,-18.3847763108502,26.1629509039023));
#47282=CARTESIAN_POINT('Origin',(-6.70710678118655,-25.4558441227157,19.0918830920368));
#47283=CARTESIAN_POINT('',(-6.35355339059327,-25.9129509039023,18.1347763108502));
#47284=CARTESIAN_POINT('',(-6.70710678118655,-25.809397513309,18.031222920257));
#47285=CARTESIAN_POINT('Origin',(-6.70710678118655,-26.1629509039023,18.3847763108502));
#47286=CARTESIAN_POINT('',(-6.70710678118655,-25.1022907321224,18.7383297014435));
#47287=CARTESIAN_POINT('',(-6.35355339059327,-25.2058441227157,18.8418830920368));
#47288=CARTESIAN_POINT('Origin',(-5.52973785412436,-26.1629509039023,20.0498274154182));
#47289=CARTESIAN_POINT('',(-6.14644660940673,-25.9129509039023,18.4276695296637));
#47290=CARTESIAN_POINT('Origin',(-6.5,-26.1629509039023,18.6776695296637));
#47291=CARTESIAN_POINT('',(-6.35355339059327,-26.4129509039023,18.1347763108502));
#47292=CARTESIAN_POINT('',(-5.17618446353109,-26.4129509039023,19.7998274154182));
#47293=CARTESIAN_POINT('Origin',(-6.70710678118655,-26.1629509039023,18.3847763108502));
#47294=CARTESIAN_POINT('',(-5.17618446353109,-25.9129509039023,19.7998274154182));
#47295=CARTESIAN_POINT('Origin',(-6.5,-26.1629509039022,18.6776695296637));
#47296=CARTESIAN_POINT('Origin',(-6.5,-26.1629509039022,18.6776695296637));
#47297=CARTESIAN_POINT('Origin',(-5.52973785412436,-22.0617315730203,28.1748550615043));
#47298=CARTESIAN_POINT('',(-6.14644660940673,-22.3117315730203,29.7970129472589));
#47299=CARTESIAN_POINT('',(-5.17618446353109,-22.3117315730203,28.4248550615043));
#47300=CARTESIAN_POINT('',(-6.14644660940673,-21.8117315730203,29.7970129472589));
#47301=CARTESIAN_POINT('Origin',(-6.5,-22.0617315730203,29.5470129472589));
#47302=CARTESIAN_POINT('',(-5.17618446353109,-21.8117315730203,28.4248550615043));
#47303=CARTESIAN_POINT('Origin',(-6.25,-24.0062752212833,28.2489159084026));
#47304=CARTESIAN_POINT('',(-6.14644660940673,-24.9937120883597,27.1150324319194));
#47305=CARTESIAN_POINT('Origin',(-6.5,-24.7437120883598,26.8650324319194));
#47306=CARTESIAN_POINT('',(-6.,-22.0617315730203,29.5470129472589));
#47307=CARTESIAN_POINT('',(-6.,-24.7437120883598,26.8650324319194));
#47308=CARTESIAN_POINT('Origin',(-6.5,-22.0617315730203,29.5470129472589));
#47309=CARTESIAN_POINT('Origin',(-6.,-24.1123412384613,24.1123412384613));
#47310=CARTESIAN_POINT('',(-6.,-18.6776695296637,26.1629509039023));
#47311=CARTESIAN_POINT('',(-6.,-23.4809703885628,21.3596500450031));
#47312=CARTESIAN_POINT('',(-6.,-19.8216927959224,27.306974170161));
#47313=CARTESIAN_POINT('Origin',(-6.5,-23.4809703885628,21.3596500450031));
#47314=CARTESIAN_POINT('',(-6.14644660940673,-18.4276695296637,25.9129509039023));
#47315=CARTESIAN_POINT('',(-6.14644660940673,-23.2309703885628,21.1096500450031));
#47316=CARTESIAN_POINT('Origin',(-6.5,-18.6776695296637,26.1629509039023));
#47317=CARTESIAN_POINT('Origin',(-6.25,-24.2184072556392,19.97576656852));
#47318=CARTESIAN_POINT('',(-4.69285113019775,-20.4833639705652,25.9129509039023));
#47319=CARTESIAN_POINT('Origin',(-6.70710678118655,-18.5792306756765,26.3574052687286));
#47320=CARTESIAN_POINT('',(-6.35355339059327,-18.3292306756765,26.6074052687286));
#47321=CARTESIAN_POINT('',(-6.70710678118655,-18.2256772850833,26.7109586593218));
#47322=CARTESIAN_POINT('Origin',(-5.04640452079103,-20.7333639705652,26.1629509039023));
#47323=CARTESIAN_POINT('',(-6.14644660940673,-18.4276695296637,26.4129509039023));
#47324=CARTESIAN_POINT('',(-4.69285113019775,-20.4833639705652,26.4129509039023));
#47325=CARTESIAN_POINT('Origin',(-6.5,-18.6776695296637,26.1629509039023));
#47326=CARTESIAN_POINT('Origin',(-6.5,-22.0617315730203,29.5470129472589));
#47327=CARTESIAN_POINT('Origin',(-6.5,-22.0617315730203,29.5470129472589));
#47328=CARTESIAN_POINT('Origin',(-6.25,-18.9504617357995,27.0821897194448));
#47329=CARTESIAN_POINT('',(-6.14644660940673,-19.5716927959224,27.556974170161));
#47330=CARTESIAN_POINT('Origin',(-6.5,-19.8216927959224,27.306974170161));
#47331=CARTESIAN_POINT('Origin',(-6.5,-18.6776695296637,26.1629509039023));
#47332=CARTESIAN_POINT('Origin',(-6.25,-29.2742207411231,21.1424927574778));
#47333=CARTESIAN_POINT('',(-6.35355339059327,-29.895451801246,21.617277208194));
#47334=CARTESIAN_POINT('Origin',(-14.,-29.8399061660723,22.0617315730203));
#47335=CARTESIAN_POINT('',(-10.0449101394378,-30.1934595566656,22.4152849636136));
#47336=CARTESIAN_POINT('',(-10.146446609406,-30.2815079190287,22.2962265447912));
#47337=CARTESIAN_POINT('Ctrl Pts',(-10.146446609406,-30.2815079190287,22.2962265447912));
#47338=CARTESIAN_POINT('Ctrl Pts',(-10.1126391838745,-30.264925350508,22.3274548959663));
#47339=CARTESIAN_POINT('Ctrl Pts',(-10.0811424950941,-30.2405707165373,
22.3636229983165));
#47340=CARTESIAN_POINT('Ctrl Pts',(-10.0542643495493,-30.2071640058445,
22.4011569393069));
#47341=CARTESIAN_POINT('Ctrl Pts',(-10.0494504338405,-30.200514147943,22.4082303723361));
#47342=CARTESIAN_POINT('Ctrl Pts',(-10.0449101394378,-30.1934595566656,
22.4152849636136));
#47343=CARTESIAN_POINT('',(-10.3535533905933,-30.3399061660723,22.0617315730203));
#47344=CARTESIAN_POINT('Origin',(-10.,-29.8399061660723,22.0617315730203));
#47345=CARTESIAN_POINT('',(-10.7071067811865,-30.1934595566656,21.708178182427));
#47346=CARTESIAN_POINT('Origin',(-10.7071067811865,-29.8399061660723,22.0617315730203));
#47347=CARTESIAN_POINT('',(-6.70710678118655,-30.1934595566656,21.708178182427));
#47348=CARTESIAN_POINT('',(-14.,-30.1934595566656,21.708178182427));
#47349=CARTESIAN_POINT('Origin',(-6.70710678118655,-29.8399061660723,22.0617315730203));
#47350=CARTESIAN_POINT('',(-14.,-30.1934595566656,22.4152849636136));
#47351=CARTESIAN_POINT('Origin',(-6.70710678118655,-29.8399061660723,22.0617315730203));
#47352=CARTESIAN_POINT('Origin',(-6.70710678118655,-29.8399061660723,22.0617315730203));
#47353=CARTESIAN_POINT('Origin',(-14.,-22.0617315730203,30.5470129472589));
#47354=CARTESIAN_POINT('',(-10.0449101394378,-22.4152849636135,30.1934595566656));
#47355=CARTESIAN_POINT('',(-14.,-22.4152849636136,30.1934595566656));
#47356=CARTESIAN_POINT('',(-10.,-22.5617315730203,30.0470129472588));
#47357=CARTESIAN_POINT('Origin',(-10.5,-22.5617315730203,30.0470129472588));
#47358=CARTESIAN_POINT('',(-10.,-30.0470129472589,22.5617315730203));
#47359=CARTESIAN_POINT('',(-10.,-24.1830519165799,28.4256926036992));
#47360=CARTESIAN_POINT('Origin',(-10.5,-30.0470129472588,22.5617315730203));
#47361=CARTESIAN_POINT('Origin',(-6.70710678118655,-29.645451801246,21.867277208194));
#47362=CARTESIAN_POINT('',(-6.70710678118655,-26.5165042944955,18.031222920257));
#47363=CARTESIAN_POINT('',(-6.70710678118655,-29.9990051918393,21.5137238176007));
#47364=CARTESIAN_POINT('Origin',(-6.70710678118655,-26.1629509039023,18.3847763108502));
#47365=CARTESIAN_POINT('Origin',(-6.70710678118655,-26.1629509039023,18.3847763108502));
#47366=CARTESIAN_POINT('Origin',(-6.70710678118655,-26.1629509039023,18.3847763108502));
#47367=CARTESIAN_POINT('Origin',(-14.,-26.1629509039023,18.3847763108502));
#47368=CARTESIAN_POINT('',(-14.,-26.5165042944955,18.031222920257));
#47369=CARTESIAN_POINT('',(-14.,-26.5165042944955,18.031222920257));
#47370=CARTESIAN_POINT('',(-14.,-25.809397513309,18.031222920257));
#47371=CARTESIAN_POINT('Origin',(-14.,-26.1629509039023,18.3847763108502));
#47372=CARTESIAN_POINT('',(-14.,-25.809397513309,18.031222920257));
#47373=CARTESIAN_POINT('Origin',(-14.,-30.5470129472589,22.0617315730203));
#47374=CARTESIAN_POINT('',(-10.7071067811865,-34.2946788875476,25.809397513309));
#47375=CARTESIAN_POINT('',(-10.7071067811865,-31.0419876940894,22.5567063198509));
#47376=CARTESIAN_POINT('',(-14.,-34.2946788875476,25.809397513309));
#47377=CARTESIAN_POINT('',(-14.,-34.2946788875476,25.809397513309));
#47378=CARTESIAN_POINT('',(-14.,-14.3948268171891,5.90954544295051));
#47379=CARTESIAN_POINT('Origin',(-10.7071067811865,-33.9411254969543,26.1629509039023));
#47380=CARTESIAN_POINT('',(-10.3535533905933,-34.1911254969543,26.4129509039023));
#47381=CARTESIAN_POINT('',(-10.7071067811865,-34.2946788875476,26.5165042944955));
#47382=CARTESIAN_POINT('Origin',(-10.7071067811865,-33.9411254969543,26.1629509039022));
#47383=CARTESIAN_POINT('Origin',(-10.7071067811865,-33.9411254969543,26.1629509039023));
#47384=CARTESIAN_POINT('',(-10.3535533905933,-34.1911254969543,25.9129509039023));
#47385=CARTESIAN_POINT('Origin',(-10.7071067811865,-33.9411254969543,26.1629509039023));
#47386=CARTESIAN_POINT('Origin',(-10.7071067811865,-33.9411254969543,26.1629509039023));
#47387=CARTESIAN_POINT('Origin',(-10.7071067811865,-30.6884343034962,22.9102597104441));
#47388=CARTESIAN_POINT('',(-10.3535533905933,-30.9384343034962,22.6602597104441));
#47389=CARTESIAN_POINT('Origin',(-14.,-33.9411254969543,26.1629509039023));
#47390=CARTESIAN_POINT('',(-14.025428935758,-34.2946788875476,26.5165042944955));
#47391=CARTESIAN_POINT('',(-14.,-34.2946788875476,26.5165042944955));
#47392=CARTESIAN_POINT('',(-14.,-34.4335120598975,26.0760286821578));
#47393=CARTESIAN_POINT('Ctrl Pts',(-14.,-34.4335120598975,26.0760286821577));
#47394=CARTESIAN_POINT('Ctrl Pts',(-14.,-34.439576740978,26.110383159214));
#47395=CARTESIAN_POINT('Ctrl Pts',(-14.0019573651892,-34.4420465318245,
26.1453834686124));
#47396=CARTESIAN_POINT('Ctrl Pts',(-14.0094015207423,-34.4388040888907,
26.2380233090204));
#47397=CARTESIAN_POINT('Ctrl Pts',(-14.0161612500453,-34.4268763441737,
26.2948454509909));
#47398=CARTESIAN_POINT('Ctrl Pts',(-14.0245143380439,-34.3882911628533,
26.3913434645052));
#47399=CARTESIAN_POINT('Ctrl Pts',(-14.026804427637,-34.3653919660536,26.4315414345033));
#47400=CARTESIAN_POINT('Ctrl Pts',(-14.026804427637,-34.3371305955527,26.4682048340719));
#47401=CARTESIAN_POINT('Ctrl Pts',(-14.026804427637,-34.3239946581065,26.4852460502184));
#47402=CARTESIAN_POINT('Ctrl Pts',(-14.0263298822064,-34.3098160327091,
26.501367149334));
#47403=CARTESIAN_POINT('Ctrl Pts',(-14.025428935758,-34.2946788875475,26.5165042944956));
#47404=CARTESIAN_POINT('Origin',(-14.,-33.9411254969543,26.1629509039023));
#47405=CARTESIAN_POINT('Origin',(-10.7071067811865,-26.8700576850888,33.2340187157677));
#47406=CARTESIAN_POINT('',(-10.3535533905933,-26.4129509039023,34.1911254969543));
#47407=CARTESIAN_POINT('',(-10.3535533905933,-27.1200576850888,33.4840187157677));
#47408=CARTESIAN_POINT('',(-10.7071067811866,-26.5165042944955,34.2946788875476));
#47409=CARTESIAN_POINT('Origin',(-10.7071067811865,-26.1629509039023,33.9411254969543));
#47410=CARTESIAN_POINT('',(-10.7071067811865,-27.2236110756821,33.587572106361));
#47411=CARTESIAN_POINT('Origin',(-8.57140452079103,-30.9207863951121,26.1629509039023));
#47412=CARTESIAN_POINT('',(-10.1464466094067,-33.8982322781408,25.9129509039023));
#47413=CARTESIAN_POINT('',(-8.21785113019776,-31.1707863951121,25.9129509039023));
#47414=CARTESIAN_POINT('',(-10.1464466094067,-33.8982322781408,26.4129509039023));
#47415=CARTESIAN_POINT('Origin',(-10.5,-33.6482322781408,26.1629509039023));
#47416=CARTESIAN_POINT('',(-8.21785113019776,-31.1707863951121,26.4129509039023));
#47417=CARTESIAN_POINT('Origin',(-10.5,-31.5319371877506,24.046655813512));
#47418=CARTESIAN_POINT('',(-10.,-33.6482322781408,26.1629509039023));
#47419=CARTESIAN_POINT('Origin',(-10.5,-33.6482322781408,26.1629509039023));
#47420=CARTESIAN_POINT('',(-10.1464466094067,-31.7819371877506,23.796655813512));
#47421=CARTESIAN_POINT('',(-10.,-31.5319371877506,24.046655813512));
#47422=CARTESIAN_POINT('Origin',(-10.5,-33.6482322781408,26.1629509039023));
#47423=CARTESIAN_POINT('Origin',(-10.5,-33.6482322781408,26.1629509039023));
#47424=CARTESIAN_POINT('Origin',(-10.25,-28.1074945521653,32.3501352392845));
#47425=CARTESIAN_POINT('',(-10.1464466094067,-26.4129509039023,33.8982322781408));
#47426=CARTESIAN_POINT('',(-10.1464466094067,-29.0949314192417,31.2162517628014));
#47427=CARTESIAN_POINT('',(-8.7011844635311,-26.4129509039023,31.8543229502591));
#47428=CARTESIAN_POINT('Origin',(-10.5,-28.8449314192417,30.9662517628014));
#47429=CARTESIAN_POINT('',(-10.,-26.1629509039023,33.6482322781408));
#47430=CARTESIAN_POINT('',(-10.,-28.8449314192417,30.9662517628014));
#47431=CARTESIAN_POINT('Origin',(-10.5,-26.1629509039023,33.6482322781408));
#47432=CARTESIAN_POINT('Origin',(-10.,-28.2842712474619,28.2842712474619));
#47433=CARTESIAN_POINT('',(-10.,-22.9506403026729,30.4359216769114));
#47434=CARTESIAN_POINT('Origin',(-6.5,-18.6776695296637,26.1629509039023));
#47435=CARTESIAN_POINT('Origin',(-14.,-18.3847763108502,26.1629509039023));
#47436=CARTESIAN_POINT('',(-14.,-18.031222920257,25.809397513309));
#47437=CARTESIAN_POINT('',(-14.,-18.031222920257,25.809397513309));
#47438=CARTESIAN_POINT('',(-14.,-18.031222920257,26.5165042944955));
#47439=CARTESIAN_POINT('Origin',(-14.,-18.3847763108502,26.1629509039023));
#47440=CARTESIAN_POINT('',(-14.,-18.031222920257,26.5165042944955));
#47441=CARTESIAN_POINT('Origin',(-14.,-17.6776695296637,26.1629509039023));
#47442=CARTESIAN_POINT('',(-14.,-25.809397513309,34.2946788875476));
#47443=CARTESIAN_POINT('',(-14.,-3.71751442127221,12.2027957955108));
#47444=CARTESIAN_POINT('',(-10.7071067811866,-25.809397513309,34.2946788875476));
#47445=CARTESIAN_POINT('',(-14.,-25.809397513309,34.2946788875476));
#47446=CARTESIAN_POINT('',(-10.7071067811866,-21.708178182427,30.1934595566656));
#47447=CARTESIAN_POINT('',(-10.7071067811866,-19.2686597873334,27.753941161572));
#47448=CARTESIAN_POINT('',(-14.,-21.708178182427,30.1934595566656));
#47449=CARTESIAN_POINT('Origin',(-14.,-22.0617315730203,29.8399061660723));
#47450=CARTESIAN_POINT('',(-10.3535533905933,-22.0617315730203,30.3399061660723));
#47451=CARTESIAN_POINT('Origin',(-10.7071067811866,-22.0617315730203,29.8399061660723));
#47452=CARTESIAN_POINT('',(-10.146446609406,-22.2962265447912,30.2815079190287));
#47453=CARTESIAN_POINT('Origin',(-10.,-22.0617315730203,29.8399061660723));
#47454=CARTESIAN_POINT('Ctrl Pts',(-10.0449101394378,-22.4152849636136,
30.1934595566656));
#47455=CARTESIAN_POINT('Ctrl Pts',(-10.0494504338405,-22.4082303723361,
30.200514147943));
#47456=CARTESIAN_POINT('Ctrl Pts',(-10.0542643495493,-22.4011569393069,
30.2071640058445));
#47457=CARTESIAN_POINT('Ctrl Pts',(-10.081142495094,-22.3636229983167,30.2405707165371));
#47458=CARTESIAN_POINT('Ctrl Pts',(-10.1126391838741,-22.3274548959667,
30.2649253505077));
#47459=CARTESIAN_POINT('Ctrl Pts',(-10.1464466094053,-22.2962265447918,
30.2815079190284));
#47460=CARTESIAN_POINT('Origin',(-10.5,-22.9506403026729,30.4359216769114));
#47461=CARTESIAN_POINT('',(-10.1464466094067,-25.9129509039023,33.8982322781408));
#47462=CARTESIAN_POINT('Origin',(-10.5,-26.1629509039023,33.6482322781408));
#47463=CARTESIAN_POINT('',(-10.1464466094067,-22.7006403026729,30.6859216769114));
#47464=CARTESIAN_POINT('Origin',(-10.5,-26.1629509039023,33.6482322781408));
#47465=CARTESIAN_POINT('Origin',(-10.5,-26.1629509039023,33.6482322781408));
#47466=CARTESIAN_POINT('Origin',(-9.05473785412437,-26.1629509039023,31.6043229502591));
#47467=CARTESIAN_POINT('',(-10.3535533905933,-25.9129509039023,34.1911254969543));
#47468=CARTESIAN_POINT('Origin',(-10.7071067811865,-26.1629509039023,33.9411254969543));
#47469=CARTESIAN_POINT('',(-8.70118446353109,-25.9129509039023,31.8543229502591));
#47470=CARTESIAN_POINT('Origin',(-14.,-26.1629509039023,34.6482322781408));
#47471=CARTESIAN_POINT('',(-14.025428935758,-26.5165042944955,34.2946788875476));
#47472=CARTESIAN_POINT('',(-14.,-26.5165042944955,34.2946788875476));
#47473=CARTESIAN_POINT('',(-14.,-27.5223620986102,33.2888210834329));
#47474=CARTESIAN_POINT('Ctrl Pts',(-14.025428935758,-26.5165042944955,34.2946788875476));
#47475=CARTESIAN_POINT('Ctrl Pts',(-14.0048893955981,-26.8615969484775,
33.9495862335655));
#47476=CARTESIAN_POINT('Ctrl Pts',(-14.,-27.2050511579839,33.6061320240592));
#47477=CARTESIAN_POINT('Ctrl Pts',(-14.,-27.5223620986102,33.2888210834329));
#47478=CARTESIAN_POINT('',(-14.,-33.2888210834329,27.5223620986102));
#47479=CARTESIAN_POINT('',(-14.,-25.2842712474619,35.5269119345812));
#47480=CARTESIAN_POINT('Ctrl Pts',(-14.,-33.2888210834329,27.5223620986102));
#47481=CARTESIAN_POINT('Ctrl Pts',(-14.,-33.6061320240592,27.2050511579839));
#47482=CARTESIAN_POINT('Ctrl Pts',(-14.0048893955981,-33.9495862335655,
26.8615969484775));
#47483=CARTESIAN_POINT('Ctrl Pts',(-14.025428935758,-34.2946788875476,26.5165042944955));
#47484=CARTESIAN_POINT('Origin',(-10.25,-31.3601857456234,23.2284577619781));
#47485=CARTESIAN_POINT('Origin',(-10.7071067811866,-19.6222131779267,27.4003877709787));
#47486=CARTESIAN_POINT('Origin',(-10.7071067811866,-26.1629509039023,33.9411254969543));
#47487=CARTESIAN_POINT('',(-10.3535533905933,-19.3722131779267,27.6503877709787));
#47488=CARTESIAN_POINT('Origin',(-10.7071067811866,-26.1629509039023,33.9411254969543));
#47489=CARTESIAN_POINT('Origin',(-10.7071067811866,-26.1629509039023,33.9411254969543));
#47490=CARTESIAN_POINT('Origin',(-14.,-26.1629509039023,33.9411254969543));
#47491=CARTESIAN_POINT('',(-14.,-26.0760286821578,34.4335120598975));
#47492=CARTESIAN_POINT('Origin',(-14.,-26.1629509039023,33.9411254969543));
#47493=CARTESIAN_POINT('Ctrl Pts',(-14.025428935758,-26.5165042944955,34.2946788875476));
#47494=CARTESIAN_POINT('Ctrl Pts',(-14.0263293530702,-26.501376039553,34.3098071424901));
#47495=CARTESIAN_POINT('Ctrl Pts',(-14.0268044276371,-26.4852549680463,
34.3239877839475));
#47496=CARTESIAN_POINT('Ctrl Pts',(-14.0268044276371,-26.4682048340719,
34.3371305955528));
#47497=CARTESIAN_POINT('Ctrl Pts',(-14.0268044276371,-26.4359460827031,
34.3619967163995));
#47498=CARTESIAN_POINT('Ctrl Pts',(-14.0250516964297,-26.4009212026149,
34.3827322393151));
#47499=CARTESIAN_POINT('Ctrl Pts',(-14.0179720411043,-26.3124348467826,
34.4215374836553));
#47500=CARTESIAN_POINT('Ctrl Pts',(-14.0115803121848,-26.2577402477616,
34.4352140696344));
#47501=CARTESIAN_POINT('Ctrl Pts',(-14.0028573458318,-26.1599875313315,
34.4429028780862));
#47502=CARTESIAN_POINT('Ctrl Pts',(-14.,-26.1175962104965,34.4408500788191));
#47503=CARTESIAN_POINT('Ctrl Pts',(-14.,-26.0760286821578,34.4335120598975));
#47504=CARTESIAN_POINT('Origin',(-10.25,-21.0364267402998,29.1681547239451));
#47505=CARTESIAN_POINT('Origin',(-14.,26.1629509039023,18.3847763108502));
#47506=CARTESIAN_POINT('',(-6.70710678118655,26.5165042944955,18.031222920257));
#47507=CARTESIAN_POINT('',(-6.70710678118655,25.809397513309,18.031222920257));
#47508=CARTESIAN_POINT('Origin',(-6.70710678118655,26.1629509039023,18.3847763108502));
#47509=CARTESIAN_POINT('',(-14.,25.809397513309,18.031222920257));
#47510=CARTESIAN_POINT('',(-14.,25.809397513309,18.031222920257));
#47511=CARTESIAN_POINT('',(-14.,26.5165042944955,18.031222920257));
#47512=CARTESIAN_POINT('Origin',(-14.,26.1629509039023,18.3847763108502));
#47513=CARTESIAN_POINT('',(-14.,26.5165042944955,18.031222920257));
#47514=CARTESIAN_POINT('Origin',(-6.70710678118654,26.3574052687286,18.5792306756765));
#47515=CARTESIAN_POINT('',(-6.35355339059328,26.4129509039023,18.1347763108502));
#47516=CARTESIAN_POINT('Origin',(-6.70710678118654,26.1629509039023,18.3847763108502));
#47517=CARTESIAN_POINT('',(-6.70710678118654,30.1934595566656,21.708178182427));
#47518=CARTESIAN_POINT('',(-6.70710678118654,26.7109586593218,18.2256772850833));
#47519=CARTESIAN_POINT('',(-6.35355339059327,30.0899061660723,21.8117315730203));
#47520=CARTESIAN_POINT('Origin',(-6.70710678118654,29.8399061660723,22.0617315730203));
#47521=CARTESIAN_POINT('',(-6.35355339059327,26.6074052687286,18.3292306756765));
#47522=CARTESIAN_POINT('Origin',(-6.70710678118654,29.8399061660723,22.0617315730203));
#47523=CARTESIAN_POINT('',(-6.35355339059327,30.0899061660723,22.3117315730203));
#47524=CARTESIAN_POINT('',(-6.70710678118655,30.1934595566656,22.4152849636136));
#47525=CARTESIAN_POINT('Origin',(-6.70710678118655,29.8399061660723,22.0617315730203));
#47526=CARTESIAN_POINT('Origin',(-6.70710678118654,29.8399061660723,22.0617315730203));
#47527=CARTESIAN_POINT('Origin',(-6.70710678118654,29.8399061660723,22.0617315730203));
#47528=CARTESIAN_POINT('Origin',(-14.,17.6776695296637,26.1629509039023));
#47529=CARTESIAN_POINT('',(-6.70710678118655,18.031222920257,25.809397513309));
#47530=CARTESIAN_POINT('',(-6.70710678118655,18.7383297014435,25.1022907321224));
#47531=CARTESIAN_POINT('',(-14.,18.031222920257,25.809397513309));
#47532=CARTESIAN_POINT('',(-14.,18.031222920257,25.809397513309));
#47533=CARTESIAN_POINT('',(-14.,22.7989898732233,21.0416305603426));
#47534=CARTESIAN_POINT('Origin',(-6.25,27.0821897194448,18.9504617357995));
#47535=CARTESIAN_POINT('',(-6.14644660940673,29.7970129472589,21.8117315730203));
#47536=CARTESIAN_POINT('',(-5.17618446353109,28.4248550615043,21.8117315730203));
#47537=CARTESIAN_POINT('',(-6.14644660940673,26.4129509039023,18.4276695296637));
#47538=CARTESIAN_POINT('',(-6.14644660940673,27.556974170161,19.5716927959224));
#47539=CARTESIAN_POINT('',(-4.69285113019775,26.4129509039023,20.4833639705652));
#47540=CARTESIAN_POINT('Origin',(-5.04640452079103,26.1629509039023,20.7333639705652));
#47541=CARTESIAN_POINT('',(-6.35355339059327,25.9129509039023,18.1347763108502));
#47542=CARTESIAN_POINT('Origin',(-6.70710678118655,26.1629509039023,18.3847763108502));
#47543=CARTESIAN_POINT('',(-6.14644660940673,25.9129509039023,18.4276695296637));
#47544=CARTESIAN_POINT('Origin',(-6.5,26.1629509039023,18.6776695296637));
#47545=CARTESIAN_POINT('',(-4.69285113019775,25.9129509039023,20.4833639705652));
#47546=CARTESIAN_POINT('Origin',(-6.70710678118655,26.1629509039023,18.3847763108502));
#47547=CARTESIAN_POINT('Origin',(-6.70710678118655,26.1629509039023,18.3847763108502));
#47548=CARTESIAN_POINT('Origin',(-6.5,27.306974170161,19.8216927959224));
#47549=CARTESIAN_POINT('',(-6.,29.5470129472589,22.0617315730203));
#47550=CARTESIAN_POINT('Origin',(-6.5,29.5470129472589,22.0617315730203));
#47551=CARTESIAN_POINT('',(-6.,26.1629509039023,18.6776695296637));
#47552=CARTESIAN_POINT('',(-6.,27.306974170161,19.8216927959224));
#47553=CARTESIAN_POINT('Origin',(-6.5,26.1629509039023,18.6776695296637));
#47554=CARTESIAN_POINT('Origin',(-6.5,26.1629509039023,18.6776695296637));
#47555=CARTESIAN_POINT('Origin',(-6.5,26.1629509039023,18.6776695296637));
#47556=CARTESIAN_POINT('Origin',(-5.52973785412436,28.1748550615043,22.0617315730203));
#47557=CARTESIAN_POINT('',(-6.14644660940673,29.7970129472589,22.3117315730203));
#47558=CARTESIAN_POINT('',(-5.17618446353109,28.4248550615043,22.3117315730203));
#47559=CARTESIAN_POINT('Origin',(-6.5,29.5470129472589,22.0617315730203));
#47560=CARTESIAN_POINT('Origin',(-6.5,29.5470129472589,22.0617315730203));
#47561=CARTESIAN_POINT('Origin',(-6.5,29.5470129472589,22.0617315730203));
#47562=CARTESIAN_POINT('Origin',(-6.70710678118655,19.0918830920368,25.4558441227157));
#47563=CARTESIAN_POINT('',(-6.35355339059327,18.1347763108502,25.9129509039023));
#47564=CARTESIAN_POINT('',(-6.35355339059327,18.8418830920368,25.2058441227157));
#47565=CARTESIAN_POINT('Origin',(-6.70710678118655,18.3847763108502,26.1629509039023));
#47566=CARTESIAN_POINT('Origin',(-6.25,19.97576656852,24.2184072556393));
#47567=CARTESIAN_POINT('',(-6.14644660940673,18.4276695296637,25.9129509039023));
#47568=CARTESIAN_POINT('',(-6.14644660940673,21.1096500450031,23.2309703885628));
#47569=CARTESIAN_POINT('',(-5.17618446353109,19.7998274154182,25.9129509039023));
#47570=CARTESIAN_POINT('Origin',(-6.5,21.3596500450031,23.4809703885628));
#47571=CARTESIAN_POINT('',(-6.,18.6776695296637,26.1629509039023));
#47572=CARTESIAN_POINT('',(-6.,21.3596500450031,23.4809703885628));
#47573=CARTESIAN_POINT('Origin',(-6.5,18.6776695296637,26.1629509039023));
#47574=CARTESIAN_POINT('Origin',(-6.,24.1123412384613,24.1123412384613));
#47575=CARTESIAN_POINT('',(-6.,22.0617315730203,29.5470129472589));
#47576=CARTESIAN_POINT('',(-6.,26.8650324319194,24.7437120883598));
#47577=CARTESIAN_POINT('',(-6.,20.9177083067616,28.4029896810001));
#47578=CARTESIAN_POINT('Origin',(-6.5,26.8650324319194,24.7437120883598));
#47579=CARTESIAN_POINT('',(-6.14644660940673,22.3117315730203,29.7970129472589));
#47580=CARTESIAN_POINT('',(-6.14644660940673,27.1150324319194,24.9937120883598));
#47581=CARTESIAN_POINT('Origin',(-6.5,22.0617315730203,29.5470129472589));
#47582=CARTESIAN_POINT('Origin',(-6.25,28.2489159084026,24.0062752212833));
#47583=CARTESIAN_POINT('',(-6.35355339059327,22.3117315730203,30.0899061660723));
#47584=CARTESIAN_POINT('',(-6.35355339059327,29.3827993848858,23.0188383542068));
#47585=CARTESIAN_POINT('',(-4.69285113019776,22.3117315730203,27.7413185063573));
#47586=CARTESIAN_POINT('Origin',(-6.70710678118655,29.1327993848858,22.7688383542068));
#47587=CARTESIAN_POINT('',(-6.70710678118655,22.4152849636136,30.1934595566656));
#47588=CARTESIAN_POINT('',(-6.70710678118655,29.486352775479,23.1223917448001));
#47589=CARTESIAN_POINT('Origin',(-6.70710678118655,22.0617315730203,29.8399061660723));
#47590=CARTESIAN_POINT('Origin',(-10.5,28.9913780286485,21.2132034355964));
#47591=CARTESIAN_POINT('',(-10.5,34.2946788875475,25.809397513309));
#47592=CARTESIAN_POINT('',(-10.,33.9411254969543,26.1629509039023));
#47593=CARTESIAN_POINT('Origin',(-10.5,33.9411254969543,26.1629509039023));
#47594=CARTESIAN_POINT('',(-10.,30.1934595566656,22.4152849636136));
#47595=CARTESIAN_POINT('',(-10.,28.9913780286485,21.2132034355964));
#47596=CARTESIAN_POINT('',(-10.5,30.1934595566656,21.708178182427));
#47597=CARTESIAN_POINT('Origin',(-10.5,29.8399061660723,22.0617315730203));
#47598=CARTESIAN_POINT('',(-10.5,29.3449314192417,20.8596500450032));
#47599=CARTESIAN_POINT('Origin',(-14.,33.9411254969543,26.1629509039023));
#47600=CARTESIAN_POINT('',(-14.025428935758,34.2946788875476,26.5165042944955));
#47601=CARTESIAN_POINT('',(-14.,34.4335120598975,26.0760286821578));
#47602=CARTESIAN_POINT('Ctrl Pts',(-14.025428935758,34.2946788875476,26.5165042944955));
#47603=CARTESIAN_POINT('Ctrl Pts',(-14.0263293530702,34.3098071424901,26.501376039553));
#47604=CARTESIAN_POINT('Ctrl Pts',(-14.026804427637,34.3239877839475,26.4852549680463));
#47605=CARTESIAN_POINT('Ctrl Pts',(-14.026804427637,34.3371305955527,26.4682048340719));
#47606=CARTESIAN_POINT('Ctrl Pts',(-14.026804427637,34.3619967163995,26.4359460827032));
#47607=CARTESIAN_POINT('Ctrl Pts',(-14.0250516964297,34.382732239315,26.4009212026149));
#47608=CARTESIAN_POINT('Ctrl Pts',(-14.0179720411043,34.4215374836553,26.3124348467826));
#47609=CARTESIAN_POINT('Ctrl Pts',(-14.0115803121848,34.4352140696344,26.2577402477615));
#47610=CARTESIAN_POINT('Ctrl Pts',(-14.0028573458318,34.4429028780862,26.1599875313316));
#47611=CARTESIAN_POINT('Ctrl Pts',(-14.,34.4408500788191,26.1175962104965));
#47612=CARTESIAN_POINT('Ctrl Pts',(-14.,34.4335120598975,26.0760286821578));
#47613=CARTESIAN_POINT('',(-10.5,34.2946788875475,26.5165042944955));
#47614=CARTESIAN_POINT('',(-14.,34.2946788875475,26.5165042944955));
#47615=CARTESIAN_POINT('Origin',(-10.5,33.9411254969543,26.1629509039023));
#47616=CARTESIAN_POINT('',(-14.,34.2946788875476,25.809397513309));
#47617=CARTESIAN_POINT('',(-14.,34.2946788875476,25.809397513309));
#47618=CARTESIAN_POINT('Origin',(-14.,33.9411254969543,26.1629509039023));
#47619=CARTESIAN_POINT('Origin',(-10.5,33.9411254969543,26.1629509039023));
#47620=CARTESIAN_POINT('Origin',(-10.5,33.9411254969543,26.1629509039023));
#47621=CARTESIAN_POINT('Origin',(-10.,28.2842712474619,28.2842712474619));
#47622=CARTESIAN_POINT('',(-10.,26.1629509039023,33.9411254969543));
#47623=CARTESIAN_POINT('',(-10.,32.1733585439879,27.9307178568686));
#47624=CARTESIAN_POINT('',(-10.,22.4152849636136,30.1934595566656));
#47625=CARTESIAN_POINT('',(-10.,23.4052344572747,31.1834090503267));
#47626=CARTESIAN_POINT('',(-10.,28.4256926036992,24.1830519165799));
#47627=CARTESIAN_POINT('Origin',(-10.5,32.1733585439879,27.9307178568686));
#47628=CARTESIAN_POINT('',(-10.5,26.5165042944955,34.2946788875475));
#47629=CARTESIAN_POINT('',(-10.5,32.5269119345812,28.2842712474619));
#47630=CARTESIAN_POINT('Origin',(-10.5,26.1629509039023,33.9411254969543));
#47631=CARTESIAN_POINT('Origin',(-14.,34.6482322781408,26.1629509039023));
#47632=CARTESIAN_POINT('',(-14.,33.2888210834329,27.5223620986102));
#47633=CARTESIAN_POINT('Ctrl Pts',(-14.025428935758,34.2946788875476,26.5165042944955));
#47634=CARTESIAN_POINT('Ctrl Pts',(-14.0048893955981,33.9495862335655,26.8615969484775));
#47635=CARTESIAN_POINT('Ctrl Pts',(-14.,33.6061320240592,27.2050511579839));
#47636=CARTESIAN_POINT('Ctrl Pts',(-14.,33.2888210834329,27.5223620986102));
#47637=CARTESIAN_POINT('',(-14.,27.5223620986102,33.2888210834329));
#47638=CARTESIAN_POINT('',(-14.,35.5269119345812,25.2842712474619));
#47639=CARTESIAN_POINT('',(-14.025428935758,26.5165042944955,34.2946788875476));
#47640=CARTESIAN_POINT('Ctrl Pts',(-14.,27.5223620986102,33.2888210834329));
#47641=CARTESIAN_POINT('Ctrl Pts',(-14.,27.2050511579839,33.6061320240592));
#47642=CARTESIAN_POINT('Ctrl Pts',(-14.0048893955981,26.8615969484775,33.9495862335655));
#47643=CARTESIAN_POINT('Ctrl Pts',(-14.025428935758,26.5165042944955,34.2946788875476));
#47644=CARTESIAN_POINT('',(-14.,26.5165042944955,34.2946788875475));
#47645=CARTESIAN_POINT('Origin',(-10.5,26.1629509039023,33.9411254969543));
#47646=CARTESIAN_POINT('',(-10.5,25.809397513309,34.2946788875475));
#47647=CARTESIAN_POINT('Origin',(-10.5,26.1629509039023,33.9411254969543));
#47648=CARTESIAN_POINT('Origin',(-10.5,26.1629509039023,33.9411254969543));
#47649=CARTESIAN_POINT('Origin',(-14.,26.1629509039023,17.6776695296637));
#47650=CARTESIAN_POINT('',(-14.,18.2027957955108,9.71751442127219));
#47651=CARTESIAN_POINT('',(-14.,30.1934595566656,21.708178182427));
#47652=CARTESIAN_POINT('Origin',(-14.,26.1629509039023,33.9411254969543));
#47653=CARTESIAN_POINT('',(-14.,26.0760286821578,34.4335120598975));
#47654=CARTESIAN_POINT('Ctrl Pts',(-14.,26.0760286821577,34.4335120598975));
#47655=CARTESIAN_POINT('Ctrl Pts',(-14.,26.110383159214,34.439576740978));
#47656=CARTESIAN_POINT('Ctrl Pts',(-14.0019573651892,26.1453834686123,34.4420465318245));
#47657=CARTESIAN_POINT('Ctrl Pts',(-14.0094015207423,26.2380233090203,34.4388040888907));
#47658=CARTESIAN_POINT('Ctrl Pts',(-14.0161612500453,26.2948454509909,34.4268763441738));
#47659=CARTESIAN_POINT('Ctrl Pts',(-14.0245143380439,26.3913434645052,34.3882911628533));
#47660=CARTESIAN_POINT('Ctrl Pts',(-14.0268044276371,26.4315414345032,34.3653919660536));
#47661=CARTESIAN_POINT('Ctrl Pts',(-14.0268044276371,26.4682048340719,34.3371305955528));
#47662=CARTESIAN_POINT('Ctrl Pts',(-14.0268044276371,26.4852460502184,34.3239946581065));
#47663=CARTESIAN_POINT('Ctrl Pts',(-14.0263298822064,26.501367149334,34.3098160327091));
#47664=CARTESIAN_POINT('Ctrl Pts',(-14.025428935758,26.5165042944956,34.2946788875475));
#47665=CARTESIAN_POINT('',(-14.,25.809397513309,34.2946788875475));
#47666=CARTESIAN_POINT('Origin',(-14.,26.1629509039023,33.9411254969543));
#47667=CARTESIAN_POINT('',(-14.,25.809397513309,34.2946788875475));
#47668=CARTESIAN_POINT('Origin',(-10.5,23.4052344572747,31.1834090503267));
#47669=CARTESIAN_POINT('',(-10.5,21.708178182427,30.1934595566656));
#47670=CARTESIAN_POINT('',(-10.5,23.0516810666815,31.53696244092));
#47671=CARTESIAN_POINT('Origin',(-10.5,22.0617315730203,29.8399061660723));
#47672=CARTESIAN_POINT('Origin',(-5.04640452079103,22.0617315730203,27.4913185063573));
#47673=CARTESIAN_POINT('',(-6.14644660940673,21.8117315730203,29.7970129472589));
#47674=CARTESIAN_POINT('Origin',(-6.5,22.0617315730203,29.5470129472589));
#47675=CARTESIAN_POINT('',(-6.35355339059327,21.8117315730203,30.0899061660723));
#47676=CARTESIAN_POINT('Origin',(-6.70710678118654,22.0617315730203,29.8399061660723));
#47677=CARTESIAN_POINT('',(-4.69285113019776,21.8117315730203,27.7413185063573));
#47678=CARTESIAN_POINT('Origin',(-6.5,20.9177083067616,28.4029896810001));
#47679=CARTESIAN_POINT('',(-6.14644660940673,18.4276695296637,26.4129509039023));
#47680=CARTESIAN_POINT('Origin',(-6.5,18.6776695296637,26.1629509039023));
#47681=CARTESIAN_POINT('Origin',(-6.5,22.0617315730203,29.5470129472589));
#47682=CARTESIAN_POINT('',(-6.14644660940673,20.6677083067616,28.6529896810001));
#47683=CARTESIAN_POINT('Origin',(-6.5,18.6776695296637,26.1629509039023));
#47684=CARTESIAN_POINT('Origin',(-6.5,18.6776695296637,26.1629509039023));
#47685=CARTESIAN_POINT('Origin',(-5.52973785412436,20.0498274154182,26.1629509039023));
#47686=CARTESIAN_POINT('',(-6.35355339059327,18.1347763108502,26.4129509039023));
#47687=CARTESIAN_POINT('Origin',(-6.70710678118654,18.3847763108502,26.1629509039023));
#47688=CARTESIAN_POINT('',(-5.17618446353109,19.7998274154182,26.4129509039023));
#47689=CARTESIAN_POINT('Origin',(-6.5,22.0617315730203,29.5470129472589));
#47690=CARTESIAN_POINT('Origin',(-6.25,21.1424927574778,29.2742207411231));
#47691=CARTESIAN_POINT('',(-6.35355339059327,21.617277208194,29.895451801246));
#47692=CARTESIAN_POINT('Origin',(-14.,30.5470129472589,22.0617315730203));
#47693=CARTESIAN_POINT('',(-14.,30.1934595566656,22.4152849636136));
#47694=CARTESIAN_POINT('',(-14.,22.4152849636136,30.1934595566656));
#47695=CARTESIAN_POINT('Origin',(-14.,29.8399061660723,22.0617315730203));
#47696=CARTESIAN_POINT('Origin',(-14.,22.0617315730203,29.8399061660723));
#47697=CARTESIAN_POINT('',(-6.70710678118655,21.708178182427,30.1934595566656));
#47698=CARTESIAN_POINT('Origin',(-6.70710678118655,22.0617315730203,29.8399061660723));
#47699=CARTESIAN_POINT('',(-14.,21.708178182427,30.1934595566656));
#47700=CARTESIAN_POINT('Origin',(-6.70710678118655,22.0617315730203,29.8399061660723));
#47701=CARTESIAN_POINT('Origin',(-6.70710678118655,22.0617315730203,29.8399061660723));
#47702=CARTESIAN_POINT('Origin',(-6.70710678118655,21.867277208194,29.645451801246));
#47703=CARTESIAN_POINT('',(-6.70710678118655,18.031222920257,26.5165042944955));
#47704=CARTESIAN_POINT('',(-6.70710678118655,21.5137238176007,29.9990051918393));
#47705=CARTESIAN_POINT('Origin',(-6.70710678118655,18.3847763108502,26.1629509039023));
#47706=CARTESIAN_POINT('Origin',(-14.,22.0617315730203,30.5470129472589));
#47707=CARTESIAN_POINT('',(-14.,18.031222920257,26.5165042944955));
#47708=CARTESIAN_POINT('',(-14.,11.9095454429505,20.3948268171891));
#47709=CARTESIAN_POINT('',(-14.,18.031222920257,26.5165042944955));
#47710=CARTESIAN_POINT('Origin',(-6.70710678118655,18.3847763108502,26.1629509039023));
#47711=CARTESIAN_POINT('Origin',(-6.70710678118655,18.3847763108502,26.1629509039023));
#47712=CARTESIAN_POINT('Origin',(-14.,18.3847763108502,26.1629509039023));
#47713=CARTESIAN_POINT('Origin',(-14.,18.3847763108502,26.1629509039023));
#47714=CARTESIAN_POINT('Origin',(-10.5,22.9506403026729,-30.4359216769115));
#47715=CARTESIAN_POINT('',(-10.1464466094067,22.2962265447905,-30.2815079190291));
#47716=CARTESIAN_POINT('',(-10.0449101394378,22.4152849636136,-30.1934595566656));
#47717=CARTESIAN_POINT('Ctrl Pts',(-10.1464466094067,22.2962265447905,-30.2815079190291));
#47718=CARTESIAN_POINT('Ctrl Pts',(-10.1423338164079,22.3000255842635,-30.279490590864));
#47719=CARTESIAN_POINT('Ctrl Pts',(-10.1382848886043,22.3038572286173,-30.2773930503804));
#47720=CARTESIAN_POINT('Ctrl Pts',(-10.1022519938418,22.3387765065044,-30.2576611364803));
#47721=CARTESIAN_POINT('Ctrl Pts',(-10.0750196076115,22.3713854144018,-30.2344766097183));
#47722=CARTESIAN_POINT('Ctrl Pts',(-10.0513757505718,22.4054361818559,-30.2031024097759));
#47723=CARTESIAN_POINT('Ctrl Pts',(-10.0480783085823,22.4103623448515,-30.1983821754277));
#47724=CARTESIAN_POINT('Ctrl Pts',(-10.0449101394378,22.4152849636135,-30.1934595566656));
#47725=CARTESIAN_POINT('',(-10.1464466094067,25.9129509039023,-33.8982322781408));
#47726=CARTESIAN_POINT('',(-10.1464466094067,22.7006403026729,-30.6859216769115));
#47727=CARTESIAN_POINT('',(-10.,26.1629509039022,-33.6482322781408));
#47728=CARTESIAN_POINT('Origin',(-10.5,26.1629509039022,-33.6482322781408));
#47729=CARTESIAN_POINT('',(-10.,22.5617315730203,-30.0470129472589));
#47730=CARTESIAN_POINT('',(-10.,22.9506403026729,-30.4359216769115));
#47731=CARTESIAN_POINT('Origin',(-10.5,22.5617315730203,-30.0470129472589));
#47732=CARTESIAN_POINT('Origin',(-9.05473785412436,26.1629509039023,-31.6043229502591));
#47733=CARTESIAN_POINT('',(-10.4571067811865,26.2923604264535,-34.4240884100988));
#47734=CARTESIAN_POINT('',(-10.3535533905933,26.4129509039023,-34.1911254969543));
#47735=CARTESIAN_POINT('Origin',(-10.7071067811865,26.1629509039023,-33.9411254969543));
#47736=CARTESIAN_POINT('',(-10.1464466094067,26.4129509039023,-33.8982322781408));
#47737=CARTESIAN_POINT('',(-8.70118446353109,26.4129509039023,-31.8543229502591));
#47738=CARTESIAN_POINT('Origin',(-10.5,26.1629509039023,-33.6482322781408));
#47739=CARTESIAN_POINT('',(-10.4829629131445,25.9129509039023,-34.3741381988465));
#47740=CARTESIAN_POINT('',(-8.70118446353109,25.9129509039023,-31.8543229502591));
#47741=CARTESIAN_POINT('Origin',(-10.7071067811865,26.1629509039023,-33.9411254969543));
#47742=CARTESIAN_POINT('Origin',(-10.5,26.1629509039023,-33.6482322781408));
#47743=CARTESIAN_POINT('Origin',(-10.5,26.1629509039022,-33.6482322781408));
#47744=CARTESIAN_POINT('Origin',(-10.,28.2842712474619,-28.2842712474619));
#47745=CARTESIAN_POINT('',(-10.,33.6482322781408,-26.1629509039023));
#47746=CARTESIAN_POINT('',(-10.,28.8449314192417,-30.9662517628014));
#47747=CARTESIAN_POINT('',(-10.,30.0470129472588,-22.5617315730203));
#47748=CARTESIAN_POINT('',(-10.,31.5319371877506,-24.046655813512));
#47749=CARTESIAN_POINT('',(-10.,24.1830519165799,-28.4256926036992));
#47750=CARTESIAN_POINT('Origin',(-10.5,28.8449314192417,-30.9662517628014));
#47751=CARTESIAN_POINT('',(-10.1464466094067,34.0446788875475,-26.2665042944955));
#47752=CARTESIAN_POINT('',(-10.1464466094067,29.0949314192417,-31.2162517628014));
#47753=CARTESIAN_POINT('',(-10.0927098751134,34.0583901847326,-26.1629509039023));
#47754=CARTESIAN_POINT('Origin',(-10.5,33.7946788875475,-26.0165042944955));
#47755=CARTESIAN_POINT('Origin',(-10.5,33.6482322781408,-26.1629509039023));
#47756=CARTESIAN_POINT('Origin',(-10.25,28.1074945521653,-32.3501352392846));
#47757=CARTESIAN_POINT('',(-10.3535533905933,34.1911254969543,-26.4129509039023));
#47758=CARTESIAN_POINT('',(-10.3535533905933,27.1200576850888,-33.4840187157677));
#47759=CARTESIAN_POINT('',(-9.35,33.481506089183,-25.703331496131));
#47760=CARTESIAN_POINT('Origin',(-10.7071067811865,26.8700576850888,-33.2340187157677));
#47761=CARTESIAN_POINT('',(-10.7071067811865,26.5165042944955,-34.2946788875476));
#47762=CARTESIAN_POINT('Origin',(-10.7071067811865,26.1629509039022,-33.9411254969543));
#47763=CARTESIAN_POINT('',(-10.7071067811865,34.2946788875475,-26.5165042944955));
#47764=CARTESIAN_POINT('',(-10.7071067811865,27.2236110756821,-33.587572106361));
#47765=CARTESIAN_POINT('Origin',(-10.7071067811865,33.9411254969543,-26.1629509039023));
#47766=CARTESIAN_POINT('Origin',(-14.,26.1629509039022,-33.9411254969543));
#47767=CARTESIAN_POINT('',(-10.5,25.809397513309,-34.2946788875476));
#47768=CARTESIAN_POINT('Origin',(-10.,26.1629509039022,-33.9411254969543));
#47769=CARTESIAN_POINT('',(-14.,25.809397513309,-34.2946788875476));
#47770=CARTESIAN_POINT('',(-14.,25.809397513309,-34.2946788875476));
#47771=CARTESIAN_POINT('',(-14.,26.5165042944955,-34.2946788875476));
#47772=CARTESIAN_POINT('Origin',(-14.,26.1629509039022,-33.9411254969543));
#47773=CARTESIAN_POINT('',(-14.,26.5165042944955,-34.2946788875476));
#47774=CARTESIAN_POINT('Origin',(-6.70710678118654,25.4558441227157,-19.0918830920368));
#47775=CARTESIAN_POINT('',(-6.35355339059327,25.9129509039023,-18.1347763108502));
#47776=CARTESIAN_POINT('',(-6.70710678118654,25.809397513309,-18.031222920257));
#47777=CARTESIAN_POINT('Origin',(-6.70710678118654,26.1629509039023,-18.3847763108502));
#47778=CARTESIAN_POINT('',(-6.70710678118654,18.031222920257,-25.809397513309));
#47779=CARTESIAN_POINT('',(-6.70710678118654,25.1022907321224,-18.7383297014435));
#47780=CARTESIAN_POINT('',(-6.35355339059327,18.1347763108502,-25.9129509039023));
#47781=CARTESIAN_POINT('Origin',(-6.70710678118654,18.3847763108502,-26.1629509039023));
#47782=CARTESIAN_POINT('',(-6.35355339059327,25.2058441227157,-18.8418830920368));
#47783=CARTESIAN_POINT('Origin',(-6.70710678118655,18.3847763108502,-26.1629509039023));
#47784=CARTESIAN_POINT('',(-6.35355339059327,18.1347763108502,-26.4129509039023));
#47785=CARTESIAN_POINT('',(-6.70710678118654,18.031222920257,-26.5165042944955));
#47786=CARTESIAN_POINT('Origin',(-6.70710678118654,18.3847763108502,-26.1629509039023));
#47787=CARTESIAN_POINT('Origin',(-6.70710678118655,18.3847763108502,-26.1629509039023));
#47788=CARTESIAN_POINT('Origin',(-6.70710678118655,18.3847763108502,-26.1629509039023));
#47789=CARTESIAN_POINT('Origin',(-6.70710678118654,26.1629509039023,-18.3847763108502));
#47790=CARTESIAN_POINT('',(-6.35355339059327,26.4129509039023,-18.1347763108502));
#47791=CARTESIAN_POINT('',(-6.70710678118655,26.5165042944955,-18.031222920257));
#47792=CARTESIAN_POINT('Origin',(-6.70710678118655,26.1629509039023,-18.3847763108502));
#47793=CARTESIAN_POINT('Origin',(-6.70710678118654,26.1629509039023,-18.3847763108502));
#47794=CARTESIAN_POINT('Origin',(-6.70710678118654,26.1629509039023,-18.3847763108502));
#47795=CARTESIAN_POINT('Origin',(-14.,26.1629509039023,-18.3847763108502));
#47796=CARTESIAN_POINT('',(-14.,26.5165042944955,-18.031222920257));
#47797=CARTESIAN_POINT('',(-14.,26.5165042944955,-18.031222920257));
#47798=CARTESIAN_POINT('',(-14.,25.809397513309,-18.031222920257));
#47799=CARTESIAN_POINT('Origin',(-14.,26.1629509039023,-18.3847763108502));
#47800=CARTESIAN_POINT('',(-14.,25.809397513309,-18.031222920257));
#47801=CARTESIAN_POINT('Origin',(-6.70710678118655,29.645451801246,-21.867277208194));
#47802=CARTESIAN_POINT('',(-6.35355339059327,30.0899061660723,-21.8117315730203));
#47803=CARTESIAN_POINT('',(-6.35355339059327,29.895451801246,-21.617277208194));
#47804=CARTESIAN_POINT('',(-6.70710678118655,30.1934595566656,-21.708178182427));
#47805=CARTESIAN_POINT('Origin',(-6.70710678118655,29.8399061660723,-22.0617315730203));
#47806=CARTESIAN_POINT('',(-6.70710678118655,29.9990051918393,-21.5137238176007));
#47807=CARTESIAN_POINT('Origin',(-5.52973785412436,26.1629509039023,-20.0498274154182));
#47808=CARTESIAN_POINT('',(-6.14644660940673,25.9129509039023,-18.4276695296637));
#47809=CARTESIAN_POINT('',(-5.17618446353109,25.9129509039023,-19.7998274154182));
#47810=CARTESIAN_POINT('',(-6.14644660940673,26.4129509039023,-18.4276695296637));
#47811=CARTESIAN_POINT('Origin',(-6.5,26.1629509039023,-18.6776695296637));
#47812=CARTESIAN_POINT('',(-5.17618446353109,26.4129509039023,-19.7998274154182));
#47813=CARTESIAN_POINT('Origin',(-6.25,24.2184072556392,-19.97576656852));
#47814=CARTESIAN_POINT('',(-6.14644660940673,18.4276695296637,-25.9129509039023));
#47815=CARTESIAN_POINT('',(-4.69285113019775,20.4833639705652,-25.9129509039023));
#47816=CARTESIAN_POINT('',(-6.14644660940673,23.2309703885628,-21.1096500450032));
#47817=CARTESIAN_POINT('Origin',(-5.04640452079103,20.7333639705652,-26.1629509039023));
#47818=CARTESIAN_POINT('',(-6.14644660940673,18.4276695296637,-26.4129509039023));
#47819=CARTESIAN_POINT('',(-4.69285113019775,20.4833639705652,-26.4129509039023));
#47820=CARTESIAN_POINT('Origin',(-6.5,18.6776695296637,-26.1629509039023));
#47821=CARTESIAN_POINT('Origin',(-6.5,19.8216927959224,-27.306974170161));
#47822=CARTESIAN_POINT('',(-6.14644660940673,21.8117315730203,-29.7970129472589));
#47823=CARTESIAN_POINT('',(-6.,22.0617315730203,-29.5470129472589));
#47824=CARTESIAN_POINT('Origin',(-6.5,22.0617315730203,-29.5470129472589));
#47825=CARTESIAN_POINT('',(-6.,18.6776695296637,-26.1629509039023));
#47826=CARTESIAN_POINT('',(-6.,19.8216927959224,-27.306974170161));
#47827=CARTESIAN_POINT('Origin',(-6.5,18.6776695296637,-26.1629509039023));
#47828=CARTESIAN_POINT('',(-6.14644660940673,19.5716927959224,-27.556974170161));
#47829=CARTESIAN_POINT('Origin',(-6.5,22.0617315730203,-29.5470129472589));
#47830=CARTESIAN_POINT('',(-6.14644660940673,22.3117315730203,-29.7970129472589));
#47831=CARTESIAN_POINT('Origin',(-6.5,22.0617315730203,-29.5470129472589));
#47832=CARTESIAN_POINT('Origin',(-6.5,22.0617315730203,-29.5470129472589));
#47833=CARTESIAN_POINT('Origin',(-6.5,18.6776695296637,-26.1629509039023));
#47834=CARTESIAN_POINT('Origin',(-6.5,18.6776695296637,-26.1629509039023));
#47835=CARTESIAN_POINT('Origin',(-5.25473785412437,22.0617315730203,-27.7859463318517));
#47836=CARTESIAN_POINT('',(-6.40272606668219,21.8703898568377,-30.2095499766867));
#47837=CARTESIAN_POINT('',(-6.35355339059327,22.3117315730203,-30.0899061660723));
#47838=CARTESIAN_POINT('Origin',(-6.70710678118655,22.0617315730203,-29.8399061660723));
#47839=CARTESIAN_POINT('',(-4.9011844635311,22.3117315730203,-28.0359463318517));
#47840=CARTESIAN_POINT('',(-6.35355339059327,21.8117315730203,-30.0899061660723));
#47841=CARTESIAN_POINT('',(-4.90118446353109,21.8117315730203,-28.0359463318517));
#47842=CARTESIAN_POINT('Origin',(-6.70710678118654,22.0617315730203,-29.8399061660723));
#47843=CARTESIAN_POINT('Origin',(-6.5,23.4809703885628,-21.3596500450032));
#47844=CARTESIAN_POINT('',(-6.,26.1629509039023,-18.6776695296637));
#47845=CARTESIAN_POINT('',(-6.,23.4809703885628,-21.3596500450032));
#47846=CARTESIAN_POINT('Origin',(-6.5,26.1629509039023,-18.6776695296637));
#47847=CARTESIAN_POINT('Origin',(-6.,24.1123412384613,-24.1123412384613));
#47848=CARTESIAN_POINT('',(-6.,29.5470129472589,-22.0617315730203));
#47849=CARTESIAN_POINT('',(-6.,24.7437120883597,-26.8650324319194));
#47850=CARTESIAN_POINT('',(-6.,28.4029896810001,-20.9177083067616));
#47851=CARTESIAN_POINT('Origin',(-6.5,24.7437120883597,-26.8650324319194));
#47852=CARTESIAN_POINT('',(-6.14644660940673,29.7970129472589,-22.3117315730203));
#47853=CARTESIAN_POINT('',(-6.14644660940673,24.9937120883597,-27.1150324319194));
#47854=CARTESIAN_POINT('Origin',(-6.5,29.5470129472589,-22.0617315730203));
#47855=CARTESIAN_POINT('Origin',(-6.25,24.0062752212833,-28.2489159084026));
#47856=CARTESIAN_POINT('',(-6.35355339059327,30.0899061660723,-22.3117315730203));
#47857=CARTESIAN_POINT('',(-6.35355339059327,23.0188383542068,-29.3827993848858));
#47858=CARTESIAN_POINT('',(-4.69285113019775,27.7413185063573,-22.3117315730203));
#47859=CARTESIAN_POINT('Origin',(-6.60355339059327,21.9885082683169,-29.766682861369));
#47860=CARTESIAN_POINT('',(-6.70710678118654,21.708178182427,-30.1934595566656));
#47861=CARTESIAN_POINT('Origin',(-6.70710678118654,22.0617315730203,-29.8399061660723));
#47862=CARTESIAN_POINT('Origin',(-6.70710678118654,22.0617315730203,-29.8399061660723));
#47863=CARTESIAN_POINT('Origin',(-6.70710678118654,18.5792306756765,-26.3574052687286));
#47864=CARTESIAN_POINT('',(-6.70710678118654,18.2256772850833,-26.7109586593218));
#47865=CARTESIAN_POINT('',(-6.35355339059327,18.3292306756765,-26.6074052687286));
#47866=CARTESIAN_POINT('Origin',(-6.25,18.9504617357995,-27.0821897194448));
#47867=CARTESIAN_POINT('Origin',(-14.,18.3847763108502,-26.1629509039023));
#47868=CARTESIAN_POINT('',(-14.,18.031222920257,-25.809397513309));
#47869=CARTESIAN_POINT('',(-14.,18.031222920257,-25.809397513309));
#47870=CARTESIAN_POINT('',(-14.,18.031222920257,-26.5165042944955));
#47871=CARTESIAN_POINT('Origin',(-14.,18.3847763108502,-26.1629509039023));
#47872=CARTESIAN_POINT('',(-14.,18.031222920257,-26.5165042944955));
#47873=CARTESIAN_POINT('Origin',(-14.,26.1629509039023,-17.6776695296637));
#47874=CARTESIAN_POINT('',(-14.,27.0416305603426,-16.7989898732233));
#47875=CARTESIAN_POINT('Origin',(-14.,22.0617315730203,-29.8399061660723));
#47876=CARTESIAN_POINT('',(-6.70710678118654,22.4152849636135,-30.1934595566656));
#47877=CARTESIAN_POINT('Origin',(-6.70710678118654,22.0617315730203,-29.8399061660723));
#47878=CARTESIAN_POINT('',(-10.5,21.708178182427,-30.1934595566656));
#47879=CARTESIAN_POINT('',(-14.,21.708178182427,-30.1934595566656));
#47880=CARTESIAN_POINT('Origin',(-10.,22.0617315730203,-29.8399061660723));
#47881=CARTESIAN_POINT('',(-14.,22.4152849636135,-30.1934595566656));
#47882=CARTESIAN_POINT('Origin',(-6.70710678118654,22.0617315730203,-29.8399061660723));
#47883=CARTESIAN_POINT('Origin',(-6.70710678118654,22.0617315730203,-29.8399061660723));
#47884=CARTESIAN_POINT('Origin',(-6.70710678118654,22.7688383542068,-29.1327993848858));
#47885=CARTESIAN_POINT('',(-6.70710678118654,30.1934595566656,-22.4152849636136));
#47886=CARTESIAN_POINT('',(-6.70710678118654,23.1223917448001,-29.486352775479));
#47887=CARTESIAN_POINT('Origin',(-6.70710678118654,29.8399061660723,-22.0617315730203));
#47888=CARTESIAN_POINT('Origin',(-14.,22.0617315730203,-30.5470129472589));
#47889=CARTESIAN_POINT('',(-10.0449101394378,30.1934595566656,-22.4152849636136));
#47890=CARTESIAN_POINT('Origin',(-10.5,30.0470129472588,-22.5617315730203));
#47891=CARTESIAN_POINT('',(-14.,30.1934595566656,-22.4152849636136));
#47892=CARTESIAN_POINT('Origin',(-14.,17.6776695296637,-26.1629509039023));
#47893=CARTESIAN_POINT('',(-14.,9.7175144212722,-18.2027957955108));
#47894=CARTESIAN_POINT('',(-10.5,20.8596500450031,-29.3449314192417));
#47895=CARTESIAN_POINT('Origin',(-10.25,21.0364267402998,-29.1681547239451));
#47896=CARTESIAN_POINT('Origin',(-10.7071067811865,30.6884343034962,-22.9102597104441));
#47897=CARTESIAN_POINT('',(-10.3535533905933,34.2946788875475,-26.0165042944955));
#47898=CARTESIAN_POINT('',(-10.7071067811865,34.2946788875475,-25.809397513309));
#47899=CARTESIAN_POINT('Origin',(-10.7071067811865,33.9411254969543,-26.1629509039023));
#47900=CARTESIAN_POINT('',(-10.7071067811865,30.1934595566656,-21.708178182427));
#47901=CARTESIAN_POINT('',(-10.7071067811865,31.0419876940894,-22.5567063198509));
#47902=CARTESIAN_POINT('',(-10.3535533905933,30.3399061660723,-22.0617315730203));
#47903=CARTESIAN_POINT('Origin',(-10.7071067811865,29.8399061660723,-22.0617315730203));
#47904=CARTESIAN_POINT('',(-10.3535533905933,30.9384343034962,-22.6602597104441));
#47905=CARTESIAN_POINT('Origin',(-14.,30.5470129472588,-22.0617315730203));
#47906=CARTESIAN_POINT('',(-14.,30.1934595566656,-21.708178182427));
#47907=CARTESIAN_POINT('',(-14.,34.2946788875475,-25.809397513309));
#47908=CARTESIAN_POINT('',(-14.,34.2946788875475,-25.809397513309));
#47909=CARTESIAN_POINT('',(-14.,20.3948268171891,-11.9095454429505));
#47910=CARTESIAN_POINT('Origin',(-9.70355339059327,33.231506089183,-25.453331496131));
#47911=CARTESIAN_POINT('',(-10.1464466094067,34.1263048569333,-26.1410234826947));
#47912=CARTESIAN_POINT('Origin',(-10.,33.4411254969543,-25.6629509039023));
#47913=CARTESIAN_POINT('Ctrl Pts',(-10.1464466094067,34.1263048569333,-26.1410234826947));
#47914=CARTESIAN_POINT('Ctrl Pts',(-10.1267754433189,34.1045114392619,-26.1470492948923));
#47915=CARTESIAN_POINT('Ctrl Pts',(-10.1087254771823,34.0818363093199,-26.1545897832218));
#47916=CARTESIAN_POINT('Ctrl Pts',(-10.0927098751134,34.0583901847326,-26.1629509039023));
#47917=CARTESIAN_POINT('Origin',(-10.7071067811865,33.9411254969543,-26.1629509039023));
#47918=CARTESIAN_POINT('Origin',(-10.7071067811865,33.9411254969543,-26.1629509039023));
#47919=CARTESIAN_POINT('Origin',(-10.7071067811865,33.9411254969543,-26.1629509039023));
#47920=CARTESIAN_POINT('Origin',(-10.5,31.5319371877506,-24.046655813512));
#47921=CARTESIAN_POINT('',(-10.1464466094067,30.2815079190291,-22.2962265447905));
#47922=CARTESIAN_POINT('',(-10.1464466094067,31.7819371877506,-23.796655813512));
#47923=CARTESIAN_POINT('Ctrl Pts',(-10.0449101394378,30.1934595566656,-22.4152849636136));
#47924=CARTESIAN_POINT('Ctrl Pts',(-10.0480783085823,30.1983821754277,-22.4103623448515));
#47925=CARTESIAN_POINT('Ctrl Pts',(-10.0513757505718,30.2031024097759,-22.4054361818559));
#47926=CARTESIAN_POINT('Ctrl Pts',(-10.0750196076115,30.2344766097183,-22.3713854144018));
#47927=CARTESIAN_POINT('Ctrl Pts',(-10.1022519938418,30.2576611364803,-22.3387765065044));
#47928=CARTESIAN_POINT('Ctrl Pts',(-10.1382848886043,30.2773930503804,-22.3038572286173));
#47929=CARTESIAN_POINT('Ctrl Pts',(-10.142333816408,30.279490590864,-22.3000255842635));
#47930=CARTESIAN_POINT('Ctrl Pts',(-10.1464466094067,30.2815079190291,-22.2962265447905));
#47931=CARTESIAN_POINT('Origin',(-6.5,26.1629509039023,-18.6776695296637));
#47932=CARTESIAN_POINT('Origin',(-6.5,26.1629509039023,-18.6776695296637));
#47933=CARTESIAN_POINT('Origin',(-14.,33.9411254969543,-26.1629509039023));
#47934=CARTESIAN_POINT('',(-14.025428935758,34.2946788875476,-26.5165042944955));
#47935=CARTESIAN_POINT('',(-14.,34.2946788875475,-26.5165042944955));
#47936=CARTESIAN_POINT('',(-14.,34.4335120598975,-26.0760286821578));
#47937=CARTESIAN_POINT('Ctrl Pts',(-14.,34.4335120598975,-26.0760286821577));
#47938=CARTESIAN_POINT('Ctrl Pts',(-14.,34.439576740978,-26.110383159214));
#47939=CARTESIAN_POINT('Ctrl Pts',(-14.0019573651892,34.4420465318245,-26.1453834686123));
#47940=CARTESIAN_POINT('Ctrl Pts',(-14.0094015207423,34.4388040888907,-26.2380233090204));
#47941=CARTESIAN_POINT('Ctrl Pts',(-14.0161612500454,34.4268763441737,-26.294845450991));
#47942=CARTESIAN_POINT('Ctrl Pts',(-14.0245143380439,34.3882911628533,-26.3913434645052));
#47943=CARTESIAN_POINT('Ctrl Pts',(-14.026804427637,34.3653919660536,-26.4315414345033));
#47944=CARTESIAN_POINT('Ctrl Pts',(-14.026804427637,34.3371305955527,-26.4682048340719));
#47945=CARTESIAN_POINT('Ctrl Pts',(-14.026804427637,34.3239946581065,-26.4852460502184));
#47946=CARTESIAN_POINT('Ctrl Pts',(-14.0263298822064,34.3098160327091,-26.501367149334));
#47947=CARTESIAN_POINT('Ctrl Pts',(-14.025428935758,34.2946788875475,-26.5165042944956));
#47948=CARTESIAN_POINT('Origin',(-14.,33.9411254969543,-26.1629509039023));
#47949=CARTESIAN_POINT('Origin',(-10.25,31.3601857456234,-23.2284577619781));
#47950=CARTESIAN_POINT('Origin',(-10.,29.8399061660723,-22.0617315730203));
#47951=CARTESIAN_POINT('Origin',(-5.04640452079103,27.4913185063573,-22.0617315730203));
#47952=CARTESIAN_POINT('',(-6.14644660940673,29.7970129472589,-21.8117315730203));
#47953=CARTESIAN_POINT('Origin',(-6.5,29.5470129472589,-22.0617315730203));
#47954=CARTESIAN_POINT('Origin',(-6.70710678118654,29.8399061660723,-22.0617315730203));
#47955=CARTESIAN_POINT('',(-4.69285113019775,27.7413185063573,-21.8117315730203));
#47956=CARTESIAN_POINT('Origin',(-6.70710678118654,29.8399061660723,-22.0617315730203));
#47957=CARTESIAN_POINT('Origin',(-6.70710678118654,29.8399061660723,-22.0617315730203));
#47958=CARTESIAN_POINT('Origin',(-14.,29.8399061660723,-22.0617315730203));
#47959=CARTESIAN_POINT('Origin',(-6.5,28.4029896810001,-20.9177083067616));
#47960=CARTESIAN_POINT('Origin',(-6.5,29.5470129472589,-22.0617315730203));
#47961=CARTESIAN_POINT('',(-6.14644660940673,28.6529896810001,-20.6677083067616));
#47962=CARTESIAN_POINT('Origin',(-6.5,29.5470129472589,-22.0617315730203));
#47963=CARTESIAN_POINT('Origin',(-6.25,29.2742207411231,-21.1424927574778));
#47964=CARTESIAN_POINT('Origin',(-76.,0.,0.));
#47965=CARTESIAN_POINT('',(-76.,-44.,-5.38844591624836E-15));
#47966=CARTESIAN_POINT('',(-76.,-5.38844591624836E-15,-44.));
#47967=CARTESIAN_POINT('Origin',(-76.,0.,0.));
#47968=CARTESIAN_POINT('',(-75.5,-5.32721357629099E-15,-43.5));
#47969=CARTESIAN_POINT('Origin',(-76.,-5.32721357629099E-15,-43.5));
#47970=CARTESIAN_POINT('Origin',(-75.5,0.,0.));
#47971=CARTESIAN_POINT('Origin',(-76.,0.,0.));
#47972=CARTESIAN_POINT('Origin',(-75.,0.,0.));
#47973=CARTESIAN_POINT('',(-81.9928932188135,-44.,-5.38844591624836E-15));
#47974=CARTESIAN_POINT('',(-75.,-44.,-5.38844591624836E-15));
#47975=CARTESIAN_POINT('',(-81.9928932188135,-28.792835000627,-33.2711985450881));
#47976=CARTESIAN_POINT('Origin',(-81.9928932188135,0.,0.));
#47977=CARTESIAN_POINT('',(-76.5,-28.7928350006269,-33.2711985450881));
#47978=CARTESIAN_POINT('',(-75.,-28.7928350006269,-33.2711985450881));
#47979=CARTESIAN_POINT('',(-76.5,-17.7850525803124,-40.2453960685632));
#47980=CARTESIAN_POINT('Origin',(-76.5,0.,0.));
#47981=CARTESIAN_POINT('',(-81.9928932188135,-17.7850525803124,-40.2453960685632));
#47982=CARTESIAN_POINT('',(-75.,-17.7850525803124,-40.2453960685632));
#47983=CARTESIAN_POINT('',(-81.9928932188135,33.2711985450881,-28.792835000627));
#47984=CARTESIAN_POINT('Origin',(-81.9928932188135,0.,0.));
#47985=CARTESIAN_POINT('',(-76.5,33.2711985450881,-28.792835000627));
#47986=CARTESIAN_POINT('',(-75.,33.2711985450881,-28.792835000627));
#47987=CARTESIAN_POINT('',(-76.5,40.2453960685632,-17.7850525803124));
#47988=CARTESIAN_POINT('Origin',(-76.5,0.,0.));
#47989=CARTESIAN_POINT('',(-81.9928932188135,40.2453960685632,-17.7850525803124));
#47990=CARTESIAN_POINT('',(-75.,40.2453960685632,-17.7850525803124));
#47991=CARTESIAN_POINT('',(-81.9928932188135,28.7928350006269,33.2711985450881));
#47992=CARTESIAN_POINT('Origin',(-81.9928932188135,0.,0.));
#47993=CARTESIAN_POINT('',(-76.5,28.7928350006269,33.2711985450881));
#47994=CARTESIAN_POINT('',(-75.,28.7928350006269,33.2711985450881));
#47995=CARTESIAN_POINT('',(-76.5,17.7850525803124,40.2453960685632));
#47996=CARTESIAN_POINT('Origin',(-76.5,0.,0.));
#47997=CARTESIAN_POINT('',(-81.9928932188135,17.7850525803124,40.2453960685632));
#47998=CARTESIAN_POINT('',(-75.,17.7850525803124,40.2453960685632));
#47999=CARTESIAN_POINT('',(-81.9928932188135,-33.2711985450881,28.7928350006269));
#48000=CARTESIAN_POINT('Origin',(-81.9928932188135,0.,0.));
#48001=CARTESIAN_POINT('',(-76.5,-33.2711985450881,28.7928350006269));
#48002=CARTESIAN_POINT('',(-75.,-33.2711985450881,28.7928350006269));
#48003=CARTESIAN_POINT('',(-76.5,-40.2453960685632,17.7850525803123));
#48004=CARTESIAN_POINT('Origin',(-76.5,0.,0.));
#48005=CARTESIAN_POINT('',(-81.9928932188135,-40.2453960685632,17.7850525803123));
#48006=CARTESIAN_POINT('',(-75.,-40.2453960685632,17.7850525803123));
#48007=CARTESIAN_POINT('Origin',(-81.9928932188135,0.,0.));
#48008=CARTESIAN_POINT('Origin',(-75.5,44.5,0.));
#48009=CARTESIAN_POINT('',(-75.5,-42.4,-5.19250242838478E-15));
#48010=CARTESIAN_POINT('Origin',(-75.5,0.,0.));
#48011=CARTESIAN_POINT('Origin',(-82.5,27.2681929349507,18.7607836329628));
#48012=CARTESIAN_POINT('',(-82.8535533905933,18.1725024134732,39.3532030423759));
#48013=CARTESIAN_POINT('',(-82.5,18.1497255644298,39.7527038317633));
#48014=CARTESIAN_POINT('Ctrl Pts',(-82.8535533905933,18.1725024134732,39.3532030423759));
#48015=CARTESIAN_POINT('Ctrl Pts',(-82.8366099658527,18.1852779971399,39.3659662456744));
#48016=CARTESIAN_POINT('Ctrl Pts',(-82.8190446071419,18.1949775258609,39.3808339631167));
#48017=CARTESIAN_POINT('Ctrl Pts',(-82.7677366682921,18.2164972638614,39.4274108400557));
#48018=CARTESIAN_POINT('Ctrl Pts',(-82.7337459048348,18.2211084931905,39.4627255203892));
#48019=CARTESIAN_POINT('Ctrl Pts',(-82.6671016739128,18.2188694611548,39.5371512535174));
#48020=CARTESIAN_POINT('Ctrl Pts',(-82.6344780878158,18.211893370137,39.5762852200451));
#48021=CARTESIAN_POINT('Ctrl Pts',(-82.5669046106341,18.1882818091273,39.661496926548));
#48022=CARTESIAN_POINT('Ctrl Pts',(-82.5323527761039,18.1704694163667,39.7076676112556));
#48023=CARTESIAN_POINT('Ctrl Pts',(-82.5,18.1497255644298,39.7527038317633));
#48024=CARTESIAN_POINT('',(-82.5,24.4987646471392,25.9685365994627));
#48025=CARTESIAN_POINT('',(-82.5,27.7223340063745,18.9699627123327));
#48026=CARTESIAN_POINT('',(-83.,24.0446235757154,25.7593575200928));
#48027=CARTESIAN_POINT('Origin',(-82.5,24.0446235757154,25.7593575200928));
#48028=CARTESIAN_POINT('',(-83.,17.9060450480377,39.0866015158896));
#48029=CARTESIAN_POINT('',(-83.,27.2681929349507,18.7607836329628));
#48030=CARTESIAN_POINT('Ctrl Pts',(-83.,17.9060450480377,39.0866015158896));
#48031=CARTESIAN_POINT('Ctrl Pts',(-83.,17.9068391651052,39.0873972685336));
#48032=CARTESIAN_POINT('Ctrl Pts',(-82.9999966660379,17.9076332865639,39.0881930147409));
#48033=CARTESIAN_POINT('Ctrl Pts',(-82.9996048777198,17.9542929979794,39.1349475530888));
#48034=CARTESIAN_POINT('Ctrl Pts',(-82.9880998337802,17.9999192181754,39.1806291884362));
#48035=CARTESIAN_POINT('Ctrl Pts',(-82.9422519329555,18.0884603751996,39.2692142985112));
#48036=CARTESIAN_POINT('Ctrl Pts',(-82.9069781960815,18.1305308491385,39.3112695307757));
#48037=CARTESIAN_POINT('Ctrl Pts',(-82.8587400616057,18.1685480689101,39.3492524644103));
#48038=CARTESIAN_POINT('Ctrl Pts',(-82.8561621144247,18.1705353985348,39.3512379336024));
#48039=CARTESIAN_POINT('Ctrl Pts',(-82.8535533905933,18.1725024134732,39.3532030423759));
#48040=CARTESIAN_POINT('Origin',(-82.5,27.2236110756821,27.2236110756821));
#48041=CARTESIAN_POINT('',(-82.5,29.9484575042249,28.4786855519015));
#48042=CARTESIAN_POINT('',(-83.,30.4025985756487,28.6878646312713));
#48043=CARTESIAN_POINT('Origin',(-82.5,30.4025985756487,28.6878646312713));
#48044=CARTESIAN_POINT('Origin',(-83.,27.2236110756821,27.2236110756821));
#48045=CARTESIAN_POINT('Origin',(-82.5,27.2236110756821,27.2236110756821));
#48046=CARTESIAN_POINT('Origin',(-82.5,36.9730332048023,14.4230336013604));
#48047=CARTESIAN_POINT('',(-82.5,28.5407738489008,31.5348562042458));
#48048=CARTESIAN_POINT('',(-83.,28.9949149203246,31.7440352836156));
#48049=CARTESIAN_POINT('Origin',(-82.5,28.9949149203246,31.7440352836156));
#48050=CARTESIAN_POINT('',(-83.,36.9730332048023,14.4230336013604));
#48051=CARTESIAN_POINT('',(-82.5,36.5188921333785,14.2138545219905));
#48052=CARTESIAN_POINT('Origin',(-82.5,28.9949149203246,31.7440352836156));
#48053=CARTESIAN_POINT('',(-82.8535533905933,29.2333555023034,32.0050833421521));
#48054=CARTESIAN_POINT('Origin',(-82.5,28.9949149203246,31.7440352836156));
#48055=CARTESIAN_POINT('Origin',(-82.5,28.9949149203246,31.7440352836156));
#48056=CARTESIAN_POINT('Origin',(-81.9928932188135,28.4656436938016,32.8931167434394));
#48057=CARTESIAN_POINT('',(-82.3464466094067,28.6970028856031,33.1604609492284));
#48058=CARTESIAN_POINT('',(-81.9928932188135,28.0115026223778,32.6839376640695));
#48059=CARTESIAN_POINT('Origin',(-81.9928932188135,28.4656436938016,32.8931167434394));
#48060=CARTESIAN_POINT('',(-81.9928932188135,27.9656436938016,32.8931167434394));
#48061=CARTESIAN_POINT('Origin',(-81.9928932188135,28.4656436938016,32.8931167434394));
#48062=CARTESIAN_POINT('',(-82.0504431038337,27.9740691453425,32.9641271232539));
#48063=CARTESIAN_POINT('Origin',(-81.9928932188135,28.4656436938016,32.8931167434394));
#48064=CARTESIAN_POINT('Origin',(-81.9928932188135,28.4656436938016,32.8931167434394));
#48065=CARTESIAN_POINT('Origin',(-81.9928932188135,28.4656436938016,32.8931167434394));
#48066=CARTESIAN_POINT('Ctrl Pts',(-82.3464466094067,28.6970028856031,33.1604609492284));
#48067=CARTESIAN_POINT('Ctrl Pts',(-82.5198916952181,28.8750299889571,32.777021537783));
#48068=CARTESIAN_POINT('Ctrl Pts',(-82.6890302423685,29.0538136387275,32.3919001753921));
#48069=CARTESIAN_POINT('Ctrl Pts',(-82.8535533905932,29.2333555023034,32.0050833421521));
#48070=CARTESIAN_POINT('Ctrl Pts',(-82.4107979354011,28.6107539071896,33.1499982741659));
#48071=CARTESIAN_POINT('Ctrl Pts',(-82.5847771257014,28.7890085398853,32.7663377509294));
#48072=CARTESIAN_POINT('Ctrl Pts',(-82.7544490809092,28.9680220426012,32.3809740568209));
#48073=CARTESIAN_POINT('Ctrl Pts',(-82.9195064441822,29.1478143532338,31.9938921294479));
#48074=CARTESIAN_POINT('Ctrl Pts',(-82.4878723202377,28.4047764122382,33.0901740387693));
#48075=CARTESIAN_POINT('Ctrl Pts',(-82.6627581651749,28.583033090945,32.7062483470394));
#48076=CARTESIAN_POINT('Ctrl Pts',(-82.8333405871198,28.7620735816751,32.3205905916121));
#48077=CARTESIAN_POINT('Ctrl Pts',(-82.9993073418929,28.9419061790346,31.9331823972077));
#48078=CARTESIAN_POINT('Ctrl Pts',(-82.402697304057,28.1204642389912,32.9204852331458));
#48079=CARTESIAN_POINT('Ctrl Pts',(-82.5777878858747,28.2977526404933,32.536956679965));
#48080=CARTESIAN_POINT('Ctrl Pts',(-82.7485753212377,28.4758222195063,32.1517086466974));
#48081=CARTESIAN_POINT('Ctrl Pts',(-82.9147495721166,28.6546921362081,31.764723584709));
#48082=CARTESIAN_POINT('Ctrl Pts',(-82.1928732504717,28.0005687726945,32.769842915114));
#48083=CARTESIAN_POINT('Ctrl Pts',(-82.3671797925051,28.17683463364,32.3873378092548));
#48084=CARTESIAN_POINT('Ctrl Pts',(-82.537183228921,28.3538706019485,32.0031656241164));
#48085=CARTESIAN_POINT('Ctrl Pts',(-82.7025711378507,28.5316782401504,31.6173102173229));
#48086=CARTESIAN_POINT('Ctrl Pts',(-82.0428577478797,28.002868743917,32.702682362758));
#48087=CARTESIAN_POINT('Ctrl Pts',(-82.2165175283878,28.178677124377,32.3209949026089));
#48088=CARTESIAN_POINT('Ctrl Pts',(-82.3858725432196,28.355232305031,31.9376749996291));
#48089=CARTESIAN_POINT('Ctrl Pts',(-82.5506111984385,28.5325481277584,31.5527147674639));
#48090=CARTESIAN_POINT('Ctrl Pts',(-81.9928932188135,28.0115026223778,32.6839376640695));
#48091=CARTESIAN_POINT('Ctrl Pts',(-82.1663383046248,28.1871793984968,32.3025322215592));
#48092=CARTESIAN_POINT('Ctrl Pts',(-82.3354768517752,28.3636014212964,31.9195088011564));
#48093=CARTESIAN_POINT('Ctrl Pts',(-82.5,28.5407738489008,31.5348562042457));
#48094=CARTESIAN_POINT('Ctrl Pts',(-82.3464466094067,28.6970028856031,33.1604609492284));
#48095=CARTESIAN_POINT('Ctrl Pts',(-82.5198916952181,28.8750299889571,32.777021537783));
#48096=CARTESIAN_POINT('Ctrl Pts',(-82.6890302423685,29.0538136387275,32.3919001753921));
#48097=CARTESIAN_POINT('Ctrl Pts',(-82.8535533905932,29.2333555023034,32.0050833421521));
#48098=CARTESIAN_POINT('Ctrl Pts',(-82.5,28.5407738489008,31.5348562042457));
#48099=CARTESIAN_POINT('Ctrl Pts',(-82.3354768517752,28.3636014212964,31.9195088011564));
#48100=CARTESIAN_POINT('Ctrl Pts',(-82.1663383046248,28.1871793984968,32.3025322215592));
#48101=CARTESIAN_POINT('Ctrl Pts',(-81.9928932188135,28.0115026223778,32.6839376640695));
#48102=CARTESIAN_POINT('Origin',(-83.,43.2,0.));
#48103=CARTESIAN_POINT('',(-83.,39.0866015158896,-17.9060450480377));
#48104=CARTESIAN_POINT('Origin',(-83.,0.,0.));
#48105=CARTESIAN_POINT('',(-83.,25.7593575200928,-24.0446235757154));
#48106=CARTESIAN_POINT('',(-83.,44.7879994647011,-15.2799597870972));
#48107=CARTESIAN_POINT('',(-83.,28.6878646312713,-30.4025985756487));
#48108=CARTESIAN_POINT('Origin',(-83.,27.2236110756821,-27.2236110756821));
#48109=CARTESIAN_POINT('',(-83.,31.7440352836156,-28.9949149203246));
#48110=CARTESIAN_POINT('',(-83.,40.4502494330987,-24.9848000569488));
#48111=CARTESIAN_POINT('',(-83.,-17.9060450480377,-39.0866015158896));
#48112=CARTESIAN_POINT('Origin',(-83.,0.,0.));
#48113=CARTESIAN_POINT('',(-83.,-24.0446235757154,-25.7593575200928));
#48114=CARTESIAN_POINT('',(-83.,-19.7071756188355,-35.1762326125546));
#48115=CARTESIAN_POINT('',(-83.,-30.4025985756487,-28.6878646312713));
#48116=CARTESIAN_POINT('Origin',(-83.,-27.2236110756821,-27.2236110756821));
#48117=CARTESIAN_POINT('',(-83.,-28.9949149203246,-31.7440352836156));
#48118=CARTESIAN_POINT('',(-83.,-29.4120158886871,-30.8384825809522));
#48119=CARTESIAN_POINT('',(-83.,-39.0866015158896,17.9060450480377));
#48120=CARTESIAN_POINT('Origin',(-83.,0.,0.));
#48121=CARTESIAN_POINT('',(-83.,-25.7593575200928,24.0446235757154));
#48122=CARTESIAN_POINT('',(-83.,-9.14901678081629,31.695408766689));
#48123=CARTESIAN_POINT('',(-83.,-28.6878646312713,30.4025985756487));
#48124=CARTESIAN_POINT('Origin',(-83.,-27.2236110756821,27.2236110756821));
#48125=CARTESIAN_POINT('',(-83.,-31.7440352836156,28.9949149203246));
#48126=CARTESIAN_POINT('',(-83.,-4.81126674921393,41.4002490365406));
#48127=CARTESIAN_POINT('Origin',(-83.,0.,0.));
#48128=CARTESIAN_POINT('',(-83.,-9.49971599022433E-16,-7.75710678118654));
#48129=CARTESIAN_POINT('Origin',(-83.,0.,0.));
#48130=CARTESIAN_POINT('Origin',(-82.5,0.,0.));
#48131=CARTESIAN_POINT('',(-82.8535533905933,39.4080313955299,-18.0532959647562));
#48132=CARTESIAN_POINT('Origin',(-82.8535533905933,4.44089209850063E-15,
-2.77555756156289E-15));
#48133=CARTESIAN_POINT('Origin',(-82.5,39.0866015158896,-17.9060450480377));
#48134=CARTESIAN_POINT('Origin',(-82.6,0.,0.));
#48135=CARTESIAN_POINT('',(-82.3464466129164,40.1114460228581,-17.7258580223676));
#48136=CARTESIAN_POINT('Origin',(-82.3464466094067,0.,-3.33066907387547E-15));
#48137=CARTESIAN_POINT('Ctrl Pts',(-82.8535533905933,39.4080313955299,-18.0532959647562));
#48138=CARTESIAN_POINT('Ctrl Pts',(-82.6854396980163,39.6430704046442,-17.9438814038579));
#48139=CARTESIAN_POINT('Ctrl Pts',(-82.5163877136628,39.8775346219,-17.8347386981006));
#48140=CARTESIAN_POINT('Ctrl Pts',(-82.3464466129164,40.1114460228581,-17.7258580223676));
#48141=CARTESIAN_POINT('Origin',(-81.9928932188135,0.,0.));
#48142=CARTESIAN_POINT('Origin',(-81.9928932188135,39.7880620223296,-17.5829497100815));
#48143=CARTESIAN_POINT('Origin',(-75.,28.4656436938016,32.8931167434394));
#48144=CARTESIAN_POINT('',(-77.,28.0115026223778,32.6839376640695));
#48145=CARTESIAN_POINT('',(-75.,28.0115026223778,32.6839376640695));
#48146=CARTESIAN_POINT('',(-77.,28.0856877263144,33.2181297628261));
#48147=CARTESIAN_POINT('Origin',(-77.,28.4656436938016,32.8931167434394));
#48148=CARTESIAN_POINT('Ctrl Pts',(-76.5,28.7928350006269,33.2711985450881));
#48149=CARTESIAN_POINT('Ctrl Pts',(-76.5009112946168,28.7921419638462,33.2717982978638));
#48150=CARTESIAN_POINT('Ctrl Pts',(-76.501822590879,28.7914472767631,33.2723961461826));
#48151=CARTESIAN_POINT('Ctrl Pts',(-76.5561204584075,28.749957410408,33.3079042591946));
#48152=CARTESIAN_POINT('Ctrl Pts',(-76.6098195625403,28.7032660033557,33.3364800964725));
#48153=CARTESIAN_POINT('Ctrl Pts',(-76.7122026008175,28.602334790547,33.3770567140054));
#48154=CARTESIAN_POINT('Ctrl Pts',(-76.7616726361357,28.5476297045157,33.3897295300249));
#48155=CARTESIAN_POINT('Ctrl Pts',(-76.850087254088,28.4352133445064,33.3951790166874));
#48156=CARTESIAN_POINT('Ctrl Pts',(-76.889996425565,28.3771217427946,33.3890059164672));
#48157=CARTESIAN_POINT('Ctrl Pts',(-76.9474081328341,28.27413553634,33.3573297979247));
#48158=CARTESIAN_POINT('Ctrl Pts',(-76.9678406878702,28.2296235623677,33.3368297278635));
#48159=CARTESIAN_POINT('Ctrl Pts',(-76.9935652964058,28.1501559864102,33.2835955472113));
#48160=CARTESIAN_POINT('Ctrl Pts',(-77.,28.1158074516949,33.253341181184));
#48161=CARTESIAN_POINT('Ctrl Pts',(-77.,28.0856877263144,33.2181297628261));
#48162=CARTESIAN_POINT('Origin',(-82.5,-9.14901678081629,31.695408766689));
#48163=CARTESIAN_POINT('',(-82.8535533905933,-39.3532030423759,18.1725024134732));
#48164=CARTESIAN_POINT('',(-82.5,-39.7527038317633,18.1497255644298));
#48165=CARTESIAN_POINT('Ctrl Pts',(-82.8535533905933,-39.3532030423759,
18.1725024134732));
#48166=CARTESIAN_POINT('Ctrl Pts',(-82.8366099658527,-39.3659662456744,
18.1852779971399));
#48167=CARTESIAN_POINT('Ctrl Pts',(-82.8190446071419,-39.3808339631167,
18.1949775258609));
#48168=CARTESIAN_POINT('Ctrl Pts',(-82.7677366682921,-39.4274108400557,
18.2164972638614));
#48169=CARTESIAN_POINT('Ctrl Pts',(-82.7337459048348,-39.4627255203892,
18.2211084931905));
#48170=CARTESIAN_POINT('Ctrl Pts',(-82.6671016739128,-39.5371512535175,
18.2188694611548));
#48171=CARTESIAN_POINT('Ctrl Pts',(-82.6344780878157,-39.5762852200451,
18.211893370137));
#48172=CARTESIAN_POINT('Ctrl Pts',(-82.5669046106341,-39.661496926548,18.1882818091273));
#48173=CARTESIAN_POINT('Ctrl Pts',(-82.5323527761039,-39.7076676112556,
18.1704694163667));
#48174=CARTESIAN_POINT('Ctrl Pts',(-82.5,-39.7527038317633,18.1497255644297));
#48175=CARTESIAN_POINT('',(-82.5,-25.9685365994627,24.4987646471392));
#48176=CARTESIAN_POINT('',(-82.5,-9.35819586018618,32.1495498381128));
#48177=CARTESIAN_POINT('Origin',(-82.5,-25.7593575200928,24.0446235757154));
#48178=CARTESIAN_POINT('Ctrl Pts',(-83.,-39.0866015158896,17.9060450480377));
#48179=CARTESIAN_POINT('Ctrl Pts',(-83.,-39.0873972740994,17.9068391706596));
#48180=CARTESIAN_POINT('Ctrl Pts',(-82.9999966659913,-39.0881930258708,
17.9076332976816));
#48181=CARTESIAN_POINT('Ctrl Pts',(-82.9996059304676,-39.1348216015621,
17.9541673017709));
#48182=CARTESIAN_POINT('Ctrl Pts',(-82.9881628075444,-39.1803794345047,
17.9996697609635));
#48183=CARTESIAN_POINT('Ctrl Pts',(-82.9424916603154,-39.2688855146336,
18.0881315731075));
#48184=CARTESIAN_POINT('Ctrl Pts',(-82.9072680988186,-39.3109720341272,
18.130233190386));
#48185=CARTESIAN_POINT('Ctrl Pts',(-82.8589631266987,-39.3490805827825,
18.1683760263469));
#48186=CARTESIAN_POINT('Ctrl Pts',(-82.8562750094044,-39.3511528916702,
18.1704502741115));
#48187=CARTESIAN_POINT('Ctrl Pts',(-82.8535533905933,-39.3532030423759,
18.1725024134732));
#48188=CARTESIAN_POINT('Origin',(-82.5,-27.2236110756821,27.2236110756821));
#48189=CARTESIAN_POINT('',(-82.5,-28.4786855519014,29.9484575042249));
#48190=CARTESIAN_POINT('Origin',(-82.5,-28.6878646312713,30.4025985756487));
#48191=CARTESIAN_POINT('Origin',(-82.5,-27.2236110756821,27.2236110756821));
#48192=CARTESIAN_POINT('Origin',(-82.5,-4.81126674921393,41.4002490365406));
#48193=CARTESIAN_POINT('',(-82.861919052854,-33.0775140978602,28.0008882573809));
#48194=CARTESIAN_POINT('Ctrl Pts',(-82.861919052854,-33.0775140978601,28.0008882573809));
#48195=CARTESIAN_POINT('Ctrl Pts',(-82.9506866114062,-32.7352615883927,
28.2610595985261));
#48196=CARTESIAN_POINT('Ctrl Pts',(-82.9991927191309,-32.2707133550685,
28.6098467819186));
#48197=CARTESIAN_POINT('Ctrl Pts',(-82.9999966796634,-31.7526069532298,
28.9886497095682));
#48198=CARTESIAN_POINT('Ctrl Pts',(-83.,-31.7483212454185,28.991782520556));
#48199=CARTESIAN_POINT('Ctrl Pts',(-83.,-31.7440352836157,28.9949149203247));
#48200=CARTESIAN_POINT('',(-82.5,-32.6839376640695,28.0115026223778));
#48201=CARTESIAN_POINT('',(-82.5,-4.60208766984403,40.9461079651168));
#48202=CARTESIAN_POINT('Origin',(-82.5,-32.8931167434394,28.4656436938016));
#48203=CARTESIAN_POINT('Origin',(-82.5,0.,0.));
#48204=CARTESIAN_POINT('',(-82.8535533905933,-29.2333555023034,-32.005083342152));
#48205=CARTESIAN_POINT('Origin',(-82.5,-28.9949149203246,-31.7440352836156));
#48206=CARTESIAN_POINT('Origin',(-82.8535533905933,0.,-1.11022302462516E-15));
#48207=CARTESIAN_POINT('Origin',(-82.5,0.,0.));
#48208=CARTESIAN_POINT('',(-82.8535533905844,-33.0858623853674,28.0042879552233));
#48209=CARTESIAN_POINT('Ctrl Pts',(-82.861919052854,-33.0775140978602,28.0008882573809));
#48210=CARTESIAN_POINT('Ctrl Pts',(-82.8591705016505,-33.0803421425098,
28.0020103183848));
#48211=CARTESIAN_POINT('Ctrl Pts',(-82.8563818305258,-33.0831248304814,
28.003144256925));
#48212=CARTESIAN_POINT('Ctrl Pts',(-82.8535533905865,-33.0858623853687,
28.0042879552254));
#48213=CARTESIAN_POINT('Origin',(-82.8535533905933,-1.66533453693773E-15,
0.));
#48214=CARTESIAN_POINT('Origin',(-83.,17.8050341073026,40.5010508850245));
#48215=CARTESIAN_POINT('',(-82.3464466094067,18.0515020953342,39.9659532237599));
#48216=CARTESIAN_POINT('Ctrl Pts',(-82.3464466094067,18.0515020953342,39.9659532237599));
#48217=CARTESIAN_POINT('Ctrl Pts',(-82.4235381014816,18.1006999631463,39.8591415269723));
#48218=CARTESIAN_POINT('Ctrl Pts',(-82.5,18.1497255644298,39.7527038317633));
#48219=CARTESIAN_POINT('',(-82.3223113642133,18.0370907815053,39.9972411016995));
#48220=CARTESIAN_POINT('Ctrl Pts',(-82.3223113642133,18.0370907815053,39.9972411016995));
#48221=CARTESIAN_POINT('Ctrl Pts',(-82.3305312270325,18.0416817288895,39.9872738632445));
#48222=CARTESIAN_POINT('Ctrl Pts',(-82.3386105716178,18.0465013314245,39.9768101999294));
#48223=CARTESIAN_POINT('Ctrl Pts',(-82.3464466094067,18.0515020953342,39.9659532237599));
#48224=CARTESIAN_POINT('',(-76.8294181454841,18.0370907815289,39.9972411016484));
#48225=CARTESIAN_POINT('',(-75.,18.0370907815053,39.9972411016995));
#48226=CARTESIAN_POINT('',(-77.,18.2783610671109,39.4734279826357));
#48227=CARTESIAN_POINT('Ctrl Pts',(-76.8294181454571,18.0370907815373,39.9972411016301));
#48228=CARTESIAN_POINT('Ctrl Pts',(-76.8802846591861,18.065500682451,39.9355614017345));
#48229=CARTESIAN_POINT('Ctrl Pts',(-76.9231860633659,18.1032378673816,39.8536315756326));
#48230=CARTESIAN_POINT('Ctrl Pts',(-76.9817250649226,18.1795903983193,39.6878653799385));
#48231=CARTESIAN_POINT('Ctrl Pts',(-77.,18.233218835034,39.5714346365688));
#48232=CARTESIAN_POINT('Ctrl Pts',(-77.,18.2783610671109,39.4734279826357));
#48233=CARTESIAN_POINT('',(-77.,24.4987646471392,25.9685365994627));
#48234=CARTESIAN_POINT('',(-77.,24.4987646471392,25.9685365994627));
#48235=CARTESIAN_POINT('',(-83.,24.4987646471392,25.9685365994627));
#48236=CARTESIAN_POINT('Origin',(-82.6,0.,0.));
#48237=CARTESIAN_POINT('',(-82.3464466094067,-33.3916700985745,28.4276364302343));
#48238=CARTESIAN_POINT('Ctrl Pts',(-82.3464466094069,-33.3916700985742,
28.4276364302344));
#48239=CARTESIAN_POINT('Ctrl Pts',(-82.3466452959177,-33.391648652821,28.427355119475));
#48240=CARTESIAN_POINT('Ctrl Pts',(-82.346844018298,-33.3916269832502,28.4270740141655));
#48241=CARTESIAN_POINT('Ctrl Pts',(-82.3957553456065,-33.3862395754527,
28.3579486596923));
#48242=CARTESIAN_POINT('Ctrl Pts',(-82.4545593255999,-33.36620626683,28.29064286912));
#48243=CARTESIAN_POINT('Ctrl Pts',(-82.5782395151542,-33.3038745068911,
28.1728689595436));
#48244=CARTESIAN_POINT('Ctrl Pts',(-82.64311889955,-33.2615715101842,28.1224065803701));
#48245=CARTESIAN_POINT('Ctrl Pts',(-82.7513471853223,-33.1789245718431,
28.0525292204883));
#48246=CARTESIAN_POINT('Ctrl Pts',(-82.8029335885286,-33.1348556429589,
28.0247564052626));
#48247=CARTESIAN_POINT('Ctrl Pts',(-82.8535533905865,-33.0858623853687,
28.0042879552254));
#48248=CARTESIAN_POINT('Origin',(-82.3464466094067,-3.33066907387547E-15,
0.));
#48249=CARTESIAN_POINT('Origin',(-75.,-32.8931167434394,28.4656436938016));
#48250=CARTESIAN_POINT('',(-77.,-32.6839376640695,28.0115026223778));
#48251=CARTESIAN_POINT('',(-75.,-32.6839376640695,28.0115026223778));
#48252=CARTESIAN_POINT('',(-77.,-33.2181297628261,28.0856877263144));
#48253=CARTESIAN_POINT('Origin',(-77.,-32.8931167434394,28.4656436938016));
#48254=CARTESIAN_POINT('Ctrl Pts',(-76.5,-33.2711985450881,28.7928350006269));
#48255=CARTESIAN_POINT('Ctrl Pts',(-76.500911294616,-33.2717982978633,28.7921419638468));
#48256=CARTESIAN_POINT('Ctrl Pts',(-76.5018225908806,-33.2723961461827,
28.791447276763));
#48257=CARTESIAN_POINT('Ctrl Pts',(-76.5561204584061,-33.3079042592076,
28.7499574103928));
#48258=CARTESIAN_POINT('Ctrl Pts',(-76.6098195625592,-33.3364800964826,
28.7032660033393));
#48259=CARTESIAN_POINT('Ctrl Pts',(-76.7122026008526,-33.3770567140169,
28.6023347905102));
#48260=CARTESIAN_POINT('Ctrl Pts',(-76.761672636178,-33.3897295300342,28.5476297044676));
#48261=CARTESIAN_POINT('Ctrl Pts',(-76.8500872541283,-33.3951790166836,
28.4352133444499));
#48262=CARTESIAN_POINT('Ctrl Pts',(-76.889996425598,-33.3890059164574,28.3771217427426));
#48263=CARTESIAN_POINT('Ctrl Pts',(-76.9474081328553,-33.3573297979066,
28.2741355362964));
#48264=CARTESIAN_POINT('Ctrl Pts',(-76.9678406878865,-33.336829727842,28.2296235623278));
#48265=CARTESIAN_POINT('Ctrl Pts',(-76.9935652964101,-33.2835955471917,
28.1501559863878));
#48266=CARTESIAN_POINT('Ctrl Pts',(-77.,-33.2533411811723,28.1158074516849));
#48267=CARTESIAN_POINT('Ctrl Pts',(-77.,-33.2181297628261,28.0856877263144));
#48268=CARTESIAN_POINT('Ctrl Pts',(-81.9928932188135,-33.2711985450881,
28.7928350006269));
#48269=CARTESIAN_POINT('Ctrl Pts',(-81.9939470017665,-33.2718920740956,
28.7920336019004));
#48270=CARTESIAN_POINT('Ctrl Pts',(-81.9950007872636,-33.2725830567574,
28.7912299961877));
#48271=CARTESIAN_POINT('Ctrl Pts',(-82.0576631913743,-33.3135201817406,
28.7433131970572));
#48272=CARTESIAN_POINT('Ctrl Pts',(-82.1197538127841,-33.3453729171763,
28.6882973488404));
#48273=CARTESIAN_POINT('Ctrl Pts',(-82.2343773913435,-33.3855972358229,
28.5708455441907));
#48274=CARTESIAN_POINT('Ctrl Pts',(-82.2882331858636,-33.3956551578982,
28.5081013386358));
#48275=CARTESIAN_POINT('Ctrl Pts',(-82.3395113735642,-33.3923414225311,
28.4373899351447));
#48276=CARTESIAN_POINT('Ctrl Pts',(-82.3429958929941,-33.3920425607612,
28.4325221351122));
#48277=CARTESIAN_POINT('Ctrl Pts',(-82.3464466094069,-33.3916700985742,
28.4276364302344));
#48278=CARTESIAN_POINT('Ctrl Pts',(-82.5,-28.5407738489008,-31.5348562042457));
#48279=CARTESIAN_POINT('Ctrl Pts',(-82.3354767269923,-28.3636012869196,
-31.9195090928971));
#48280=CARTESIAN_POINT('Ctrl Pts',(-82.1663384008616,-28.1871794959658,
-32.3025320099479));
#48281=CARTESIAN_POINT('Ctrl Pts',(-81.9928932185014,-28.0115026220617,
-32.6839376647557));
#48282=CARTESIAN_POINT('Ctrl Pts',(-82.601222396877,-28.5243224066161,-31.570573330682));
#48283=CARTESIAN_POINT('Ctrl Pts',(-82.4362685881547,-28.3468680421775,
-31.9558433587761));
#48284=CARTESIAN_POINT('Ctrl Pts',(-82.266696368842,-28.17016995578,-32.3394554481576));
#48285=CARTESIAN_POINT('Ctrl Pts',(-82.0928222766332,-27.9942348651397,
-32.7214270621338));
#48286=CARTESIAN_POINT('Ctrl Pts',(-82.8034223550171,-28.5581838001894,
-31.6726547394673));
#48287=CARTESIAN_POINT('Ctrl Pts',(-82.6376066813012,-28.3799605743899,
-32.0590647631586));
#48288=CARTESIAN_POINT('Ctrl Pts',(-82.4671755612215,-28.202520651421,-32.4437642807502));
#48289=CARTESIAN_POINT('Ctrl Pts',(-82.2924428677096,-28.0258606823619,
-32.8267719987384));
#48290=CARTESIAN_POINT('Ctrl Pts',(-82.9826254704188,-28.7876553692672,
-31.8549987460867));
#48291=CARTESIAN_POINT('Ctrl Pts',(-82.8163920970618,-28.6082163213685,
-32.2423197945722));
#48292=CARTESIAN_POINT('Ctrl Pts',(-82.6455413605155,-28.4295675026153,
-32.6278870365822));
#48293=CARTESIAN_POINT('Ctrl Pts',(-82.4703908997593,-28.2517145084275,
-33.0117234332617));
#48294=CARTESIAN_POINT('Ctrl Pts',(-82.9669916294052,-29.0496559660236,
-31.9689903150268));
#48295=CARTESIAN_POINT('Ctrl Pts',(-82.801451982201,-28.8697784920648,-32.3562635518781));
#48296=CARTESIAN_POINT('Ctrl Pts',(-82.6312976029413,-28.6906846360163,
-32.7417993726423));
#48297=CARTESIAN_POINT('Ctrl Pts',(-82.4568372372109,-28.5123652574907,
-33.1256165828682));
#48298=CARTESIAN_POINT('Ctrl Pts',(-82.8865299173878,-29.1905849277686,
-31.9994877358));
#48299=CARTESIAN_POINT('Ctrl Pts',(-82.7217411730814,-29.0109209132906,
-32.3864371172518));
#48300=CARTESIAN_POINT('Ctrl Pts',(-82.5523328602259,-28.832016226968,-32.771679559501));
#48301=CARTESIAN_POINT('Ctrl Pts',(-82.3786222720913,-28.6538783960759,
-33.1552296123872));
#48302=CARTESIAN_POINT('Ctrl Pts',(-82.8535533905933,-29.2333555023034,
-32.005083342152));
#48303=CARTESIAN_POINT('Ctrl Pts',(-82.6890301175855,-29.0538135025535,
-32.3919004687743));
#48304=CARTESIAN_POINT('Ctrl Pts',(-82.5198917914549,-28.87503008773,-32.7770213250434));
#48305=CARTESIAN_POINT('Ctrl Pts',(-82.3464466090947,-28.6970028852828,
-33.1604609499183));
#48306=CARTESIAN_POINT('',(-81.9928932185014,-28.0115026220617,-32.6839376647557));
#48307=CARTESIAN_POINT('',(-82.3464466090947,-28.6970028851807,-33.1604609498003));
#48308=CARTESIAN_POINT('Origin',(-81.9928932185014,-28.4656436934856,-32.8931167441256));
#48309=CARTESIAN_POINT('Ctrl Pts',(-82.3464466090947,-28.6970028852828,
-33.1604609499183));
#48310=CARTESIAN_POINT('Ctrl Pts',(-82.5198917914549,-28.87503008773,-32.7770213250434));
#48311=CARTESIAN_POINT('Ctrl Pts',(-82.6890301175855,-29.0538135025535,
-32.3919004687743));
#48312=CARTESIAN_POINT('Ctrl Pts',(-82.8535533905933,-29.2333555023034,
-32.005083342152));
#48313=CARTESIAN_POINT('',(-82.5,-28.5407738489008,-31.5348562042457));
#48314=CARTESIAN_POINT('Origin',(-82.5,-28.9949149203246,-31.7440352836156));
#48315=CARTESIAN_POINT('Ctrl Pts',(-82.5,-28.5407738489008,-31.5348562042457));
#48316=CARTESIAN_POINT('Ctrl Pts',(-82.3354767269923,-28.3636012869196,
-31.9195090928971));
#48317=CARTESIAN_POINT('Ctrl Pts',(-82.1663384008616,-28.1871794959658,
-32.3025320099479));
#48318=CARTESIAN_POINT('Ctrl Pts',(-81.9928932185014,-28.0115026220617,
-32.6839376647557));
#48319=CARTESIAN_POINT('Origin',(-82.5,-28.9949149203246,-31.7440352836156));
#48320=CARTESIAN_POINT('Origin',(-82.5,-28.9949149203246,-31.7440352836156));
#48321=CARTESIAN_POINT('Origin',(-75.,-28.4656436938016,-32.8931167434394));
#48322=CARTESIAN_POINT('',(-77.,-28.0856877263144,-33.2181297628261));
#48323=CARTESIAN_POINT('Ctrl Pts',(-76.5,-28.7928350006269,-33.2711985450881));
#48324=CARTESIAN_POINT('Ctrl Pts',(-76.5009112946178,-28.7921419638454,
-33.2717982978645));
#48325=CARTESIAN_POINT('Ctrl Pts',(-76.501822590878,-28.791447276762,-33.2723961461835));
#48326=CARTESIAN_POINT('Ctrl Pts',(-76.5561204584386,-28.7499574104089,
-33.3079042591934));
#48327=CARTESIAN_POINT('Ctrl Pts',(-76.6098195625684,-28.7032660033313,
-33.3364800964874));
#48328=CARTESIAN_POINT('Ctrl Pts',(-76.7122026008691,-28.602334790493,-33.3770567140222));
#48329=CARTESIAN_POINT('Ctrl Pts',(-76.7616726361978,-28.5476297044451,
-33.3897295300385));
#48330=CARTESIAN_POINT('Ctrl Pts',(-76.8500872541471,-28.4352133444235,
-33.3951790166818));
#48331=CARTESIAN_POINT('Ctrl Pts',(-76.8899964256134,-28.3771217427184,
-33.3890059164528));
#48332=CARTESIAN_POINT('Ctrl Pts',(-76.9474081328652,-28.2741355362761,
-33.3573297978981));
#48333=CARTESIAN_POINT('Ctrl Pts',(-76.9678406878941,-28.2296235623091,
-33.3368297278319));
#48334=CARTESIAN_POINT('Ctrl Pts',(-76.9935652964121,-28.1501559863774,
-33.2835955471825));
#48335=CARTESIAN_POINT('Ctrl Pts',(-77.,-28.1158074516803,-33.2533411811668));
#48336=CARTESIAN_POINT('Ctrl Pts',(-77.,-28.0856877263144,-33.2181297628261));
#48337=CARTESIAN_POINT('',(-81.9928932188135,-27.9656436938016,-32.8931167438896));
#48338=CARTESIAN_POINT('Origin',(-81.9928932188135,-28.4656436938016,-32.8931167434394));
#48339=CARTESIAN_POINT('Origin',(-81.9928932188135,-28.4656436938016,-32.8931167434394));
#48340=CARTESIAN_POINT('',(-77.,-28.0115026223778,-32.6839376640695));
#48341=CARTESIAN_POINT('',(-75.,-28.0115026223778,-32.6839376640695));
#48342=CARTESIAN_POINT('Origin',(-77.,-28.4656436938016,-32.8931167434394));
#48343=CARTESIAN_POINT('Origin',(-81.9928932188135,-28.4656436932813,-32.8931167438896));
#48344=CARTESIAN_POINT('Origin',(-81.9928932188135,-28.4656436932813,-32.8931167438896));
#48345=CARTESIAN_POINT('',(-82.050443104264,-27.9740691449652,-32.9641271243453));
#48346=CARTESIAN_POINT('Origin',(-81.9928932188135,-28.4656436932813,-32.8931167438896));
#48347=CARTESIAN_POINT('Origin',(-83.,-40.5010508850245,17.8050341073026));
#48348=CARTESIAN_POINT('',(-82.3464466094067,-39.9659532237599,18.0515020953342));
#48349=CARTESIAN_POINT('Ctrl Pts',(-82.3464466094067,-39.9659532237599,
18.0515020953342));
#48350=CARTESIAN_POINT('Ctrl Pts',(-82.4235381014816,-39.8591415269723,
18.1006999631463));
#48351=CARTESIAN_POINT('Ctrl Pts',(-82.5,-39.7527038317633,18.1497255644298));
#48352=CARTESIAN_POINT('',(-82.3223113642133,-39.9972411016995,18.0370907815053));
#48353=CARTESIAN_POINT('Ctrl Pts',(-82.3223113642133,-39.9972411016995,
18.0370907815053));
#48354=CARTESIAN_POINT('Ctrl Pts',(-82.3305312270325,-39.9872738632445,
18.0416817288895));
#48355=CARTESIAN_POINT('Ctrl Pts',(-82.3386105716178,-39.9768101999294,
18.0465013314245));
#48356=CARTESIAN_POINT('Ctrl Pts',(-82.3464466094067,-39.9659532237599,
18.0515020953341));
#48357=CARTESIAN_POINT('',(-76.8294181454841,-39.9972411016484,18.0370907815288));
#48358=CARTESIAN_POINT('',(-75.,-39.9972411016995,18.0370907815053));
#48359=CARTESIAN_POINT('',(-77.,-39.4734279826357,18.2783610671109));
#48360=CARTESIAN_POINT('Ctrl Pts',(-76.8294181454571,-39.9972411016301,
18.0370907815373));
#48361=CARTESIAN_POINT('Ctrl Pts',(-76.8802846591861,-39.9355614017345,
18.065500682451));
#48362=CARTESIAN_POINT('Ctrl Pts',(-76.9231860633659,-39.8536315756326,
18.1032378673816));
#48363=CARTESIAN_POINT('Ctrl Pts',(-76.9817250649226,-39.6878653799385,
18.1795903983192));
#48364=CARTESIAN_POINT('Ctrl Pts',(-77.,-39.5714346365688,18.233218835034));
#48365=CARTESIAN_POINT('Ctrl Pts',(-77.,-39.4734279826357,18.2783610671109));
#48366=CARTESIAN_POINT('',(-77.,-25.9685365994627,24.4987646471392));
#48367=CARTESIAN_POINT('',(-77.,-25.9685365994627,24.4987646471392));
#48368=CARTESIAN_POINT('',(-83.,-25.9685365994627,24.4987646471392));
#48369=CARTESIAN_POINT('Origin',(-82.6,0.,0.));
#48370=CARTESIAN_POINT('Origin',(-82.3464466094067,0.,1.11022302462516E-15));
#48371=CARTESIAN_POINT('Origin',(-81.9928932188135,0.,0.));
#48372=CARTESIAN_POINT('Ctrl Pts',(-81.9928932188135,-40.2453960685632,
17.7850525803124));
#48373=CARTESIAN_POINT('Ctrl Pts',(-81.9939472381724,-40.2449675863739,
17.7860221830357));
#48374=CARTESIAN_POINT('Ctrl Pts',(-81.9950012600764,-40.2445360196401,
17.7869904254498));
#48375=CARTESIAN_POINT('Ctrl Pts',(-82.0547007770009,-40.2199175482614,
17.8417542131912));
#48376=CARTESIAN_POINT('Ctrl Pts',(-82.1137599900357,-40.186017191161,17.891710645152));
#48377=CARTESIAN_POINT('Ctrl Pts',(-82.2236189798636,-40.1028545535996,
17.9756182289286));
#48378=CARTESIAN_POINT('Ctrl Pts',(-82.2755452949045,-40.0539486860789,
18.0109710556312));
#48379=CARTESIAN_POINT('Ctrl Pts',(-82.3223113642133,-39.9972411016995,
18.0370907815053));
#48380=CARTESIAN_POINT('Origin',(-75.,-39.7880620223296,17.5829497100815));
#48381=CARTESIAN_POINT('Ctrl Pts',(-76.829418145442,-39.9972411016484,18.0370907815288));
#48382=CARTESIAN_POINT('Ctrl Pts',(-76.7894304995805,-40.0457293076422,
18.0147569321475));
#48383=CARTESIAN_POINT('Ctrl Pts',(-76.7456834207506,-40.088484052965,17.9856744463975));
#48384=CARTESIAN_POINT('Ctrl Pts',(-76.6365588529939,-40.1769760907868,
17.9049698494587));
#48385=CARTESIAN_POINT('Ctrl Pts',(-76.5686581389593,-40.2173075134492,
17.8481334281707));
#48386=CARTESIAN_POINT('Ctrl Pts',(-76.5009411428971,-40.2450128585448,
17.7859180752662));
#48387=CARTESIAN_POINT('Ctrl Pts',(-76.5004705713342,-40.2452047709046,
17.7854854634878));
#48388=CARTESIAN_POINT('Ctrl Pts',(-76.5,-40.2453960685632,17.7850525803123));
#48389=CARTESIAN_POINT('Origin',(-83.,-28.4786855519014,29.9484575042249));
#48390=CARTESIAN_POINT('',(-77.,-28.4786855519014,29.9484575042249));
#48391=CARTESIAN_POINT('',(-83.,-28.4786855519014,29.9484575042249));
#48392=CARTESIAN_POINT('',(-77.,-43.0111998374632,23.2547269643883));
#48393=CARTESIAN_POINT('Origin',(-81.9928932188135,0.,0.));
#48394=CARTESIAN_POINT('Ctrl Pts',(-81.9928932188135,17.7850525803123,40.2453960685632));
#48395=CARTESIAN_POINT('Ctrl Pts',(-81.9939472381728,17.786022183036,40.2449675863738));
#48396=CARTESIAN_POINT('Ctrl Pts',(-81.9950012600754,17.7869904254506,40.2445360196398));
#48397=CARTESIAN_POINT('Ctrl Pts',(-82.0547007770136,17.84175421318,40.2199175482663));
#48398=CARTESIAN_POINT('Ctrl Pts',(-82.1137599900355,17.8917106451519,40.1860171911611));
#48399=CARTESIAN_POINT('Ctrl Pts',(-82.2236189798635,17.9756182289286,40.1028545535997));
#48400=CARTESIAN_POINT('Ctrl Pts',(-82.2755452949045,18.0109710556312,40.0539486860789));
#48401=CARTESIAN_POINT('Ctrl Pts',(-82.3223113642133,18.0370907815053,39.9972411016995));
#48402=CARTESIAN_POINT('Origin',(-75.,17.5829497100815,39.7880620223296));
#48403=CARTESIAN_POINT('Ctrl Pts',(-76.829418145442,18.0370907815289,39.9972411016484));
#48404=CARTESIAN_POINT('Ctrl Pts',(-76.7894304995805,18.0147569321475,40.0457293076422));
#48405=CARTESIAN_POINT('Ctrl Pts',(-76.7456834207506,17.9856744463976,40.088484052965));
#48406=CARTESIAN_POINT('Ctrl Pts',(-76.6365588529938,17.9049698494586,40.176976090787));
#48407=CARTESIAN_POINT('Ctrl Pts',(-76.5686581389664,17.8481334281635,40.2173075134524));
#48408=CARTESIAN_POINT('Ctrl Pts',(-76.5009411428974,17.7859180752668,40.2450128585445));
#48409=CARTESIAN_POINT('Ctrl Pts',(-76.5004705713336,17.7854854634873,40.2452047709049));
#48410=CARTESIAN_POINT('Ctrl Pts',(-76.5,17.7850525803123,40.2453960685632));
#48411=CARTESIAN_POINT('Origin',(-83.,29.9484575042249,28.4786855519015));
#48412=CARTESIAN_POINT('',(-77.,29.9484575042249,28.4786855519015));
#48413=CARTESIAN_POINT('',(-83.,29.9484575042249,28.4786855519015));
#48414=CARTESIAN_POINT('',(-77.,23.2547269643883,43.0111998374633));
#48415=CARTESIAN_POINT('Ctrl Pts',(-81.9928932223231,39.9972410968818,-18.0370907837244));
#48416=CARTESIAN_POINT('Ctrl Pts',(-82.1628343230695,39.7639623455707,-18.1445398507793));
#48417=CARTESIAN_POINT('Ctrl Pts',(-82.331886307423,39.530149144004,-18.2522350876248));
#48418=CARTESIAN_POINT('Ctrl Pts',(-82.5,39.2957805952595,-18.3601861194615));
#48419=CARTESIAN_POINT('Ctrl Pts',(-82.1335529082636,40.0817756848435,-17.9981538357199));
#48420=CARTESIAN_POINT('Ctrl Pts',(-82.303363849546,39.8479876918321,-18.1058233857611));
#48421=CARTESIAN_POINT('Ctrl Pts',(-82.4723016542503,39.6136883508133,-18.2137706610956));
#48422=CARTESIAN_POINT('Ctrl Pts',(-82.6402844586922,39.3787952697101,-18.321949249316));
#48423=CARTESIAN_POINT('Ctrl Pts',(-82.2718712658937,40.1264553236608,-17.87639229832));
#48424=CARTESIAN_POINT('Ctrl Pts',(-82.4415798928791,39.8923864524203,-17.9847127214014));
#48425=CARTESIAN_POINT('Ctrl Pts',(-82.6104201587052,39.6578020933961,-18.0933094953168));
#48426=CARTESIAN_POINT('Ctrl Pts',(-82.7782997031823,39.422614172472,-18.2021497484197));
#48427=CARTESIAN_POINT('Ctrl Pts',(-82.3464466129164,40.1114460228581,-17.7258580223676));
#48428=CARTESIAN_POINT('Ctrl Pts',(-82.5163877136628,39.8775346219,-17.8347386981006));
#48429=CARTESIAN_POINT('Ctrl Pts',(-82.6854396980163,39.6430704046442,-17.9438814038579));
#48430=CARTESIAN_POINT('Ctrl Pts',(-82.8535533905933,39.4080313955299,-18.0532959647562));
#48431=CARTESIAN_POINT('',(-82.5,39.2957805952595,-18.3601861194615));
#48432=CARTESIAN_POINT('Origin',(-82.5,39.0866015158896,-17.9060450480377));
#48433=CARTESIAN_POINT('',(-81.9928932223231,39.9972410992906,-18.0370907826149));
#48434=CARTESIAN_POINT('Origin',(-81.9928932223231,39.7880620175119,-17.5829497123006));
#48435=CARTESIAN_POINT('Ctrl Pts',(-81.9928932223231,39.9972410968818,-18.0370907837244));
#48436=CARTESIAN_POINT('Ctrl Pts',(-82.1628343230695,39.7639623455707,-18.1445398507793));
#48437=CARTESIAN_POINT('Ctrl Pts',(-82.331886307423,39.530149144004,-18.2522350876248));
#48438=CARTESIAN_POINT('Ctrl Pts',(-82.5,39.2957805952595,-18.3601861194615));
#48439=CARTESIAN_POINT('Origin',(-82.5,39.0866015158896,-17.9060450480377));
#48440=CARTESIAN_POINT('Origin',(-82.5,39.0866015158896,-17.9060450480377));
#48441=CARTESIAN_POINT('Origin',(-81.9928932223231,39.7880620223296,-17.5829497100815));
#48442=CARTESIAN_POINT('Origin',(-81.9928932223231,39.7880620223296,-17.5829497100815));
#48443=CARTESIAN_POINT('Origin',(-82.5,44.7879994647011,-15.2799597870972));
#48444=CARTESIAN_POINT('',(-82.5,25.9685365994627,-24.4987646471392));
#48445=CARTESIAN_POINT('',(-82.5,44.997178544071,-15.734100858521));
#48446=CARTESIAN_POINT('Origin',(-82.5,25.7593575200928,-24.0446235757154));
#48447=CARTESIAN_POINT('Origin',(-83.,40.5010508850245,-17.8050341073026));
#48448=CARTESIAN_POINT('',(-76.8294181454841,39.9972411016484,-18.0370907815289));
#48449=CARTESIAN_POINT('',(-75.,39.9972411016995,-18.0370907815054));
#48450=CARTESIAN_POINT('',(-77.,39.4734279826357,-18.2783610671109));
#48451=CARTESIAN_POINT('Ctrl Pts',(-76.8294181454571,39.99724110163,-18.0370907815373));
#48452=CARTESIAN_POINT('Ctrl Pts',(-76.8802846591861,39.9355614017345,-18.065500682451));
#48453=CARTESIAN_POINT('Ctrl Pts',(-76.9231860633659,39.8536315756326,-18.1032378673816));
#48454=CARTESIAN_POINT('Ctrl Pts',(-76.9817250649226,39.6878653799385,-18.1795903983193));
#48455=CARTESIAN_POINT('Ctrl Pts',(-77.,39.5714346365688,-18.233218835034));
#48456=CARTESIAN_POINT('Ctrl Pts',(-77.,39.4734279826357,-18.2783610671109));
#48457=CARTESIAN_POINT('',(-77.,25.9685365994627,-24.4987646471392));
#48458=CARTESIAN_POINT('',(-77.,25.9685365994627,-24.4987646471392));
#48459=CARTESIAN_POINT('',(-83.,25.9685365994627,-24.4987646471392));
#48460=CARTESIAN_POINT('Origin',(-75.,39.7880620223296,-17.5829497100815));
#48461=CARTESIAN_POINT('Ctrl Pts',(-76.829418145442,39.9972411016484,-18.0370907815289));
#48462=CARTESIAN_POINT('Ctrl Pts',(-76.7894304995805,40.0457293076422,-18.0147569321475));
#48463=CARTESIAN_POINT('Ctrl Pts',(-76.7456834207506,40.088484052965,-17.9856744463975));
#48464=CARTESIAN_POINT('Ctrl Pts',(-76.6365588529939,40.1769760907868,-17.9049698494588));
#48465=CARTESIAN_POINT('Ctrl Pts',(-76.5686581389598,40.2173075134493,-17.8481334281704));
#48466=CARTESIAN_POINT('Ctrl Pts',(-76.5009411428979,40.2450128585444,-17.785918075267));
#48467=CARTESIAN_POINT('Ctrl Pts',(-76.5004705713334,40.245204770905,-17.7854854634871));
#48468=CARTESIAN_POINT('Ctrl Pts',(-76.5,40.2453960685632,-17.7850525803124));
#48469=CARTESIAN_POINT('Origin',(-75.,-17.5829497100816,-39.7880620223296));
#48470=CARTESIAN_POINT('',(-81.9928932188135,-18.0370907815054,-39.9972411016994));
#48471=CARTESIAN_POINT('Origin',(-81.9928932188135,-17.5829497100816,-39.7880620223296));
#48472=CARTESIAN_POINT('',(-76.8294181454841,-18.0370907815289,-39.9972411016484));
#48473=CARTESIAN_POINT('Ctrl Pts',(-76.829418145442,-18.0370907815289,-39.9972411016484));
#48474=CARTESIAN_POINT('Ctrl Pts',(-76.7894304995805,-18.0147569321475,
-40.0457293076422));
#48475=CARTESIAN_POINT('Ctrl Pts',(-76.7456834207506,-17.9856744463976,
-40.088484052965));
#48476=CARTESIAN_POINT('Ctrl Pts',(-76.6365588529926,-17.9049698494578,
-40.1769760907878));
#48477=CARTESIAN_POINT('Ctrl Pts',(-76.5686581390476,-17.8481334280872,
-40.2173075134863));
#48478=CARTESIAN_POINT('Ctrl Pts',(-76.5009411428928,-17.7859180752669,
-40.2450128585444));
#48479=CARTESIAN_POINT('Ctrl Pts',(-76.5004705713346,-17.7854854634883,
-40.2452047709044));
#48480=CARTESIAN_POINT('Ctrl Pts',(-76.5,-17.7850525803124,-40.2453960685632));
#48481=CARTESIAN_POINT('',(-75.,-18.0370907815054,-39.9972411016994));
#48482=CARTESIAN_POINT('Ctrl Pts',(-81.9928932188135,-18.0370907815054,
-39.9972411016994));
#48483=CARTESIAN_POINT('Ctrl Pts',(-82.162834320742,-18.1445398492965,-39.7639623487899));
#48484=CARTESIAN_POINT('Ctrl Pts',(-82.3318863062657,-18.2522350868817,
-39.5301491456174));
#48485=CARTESIAN_POINT('Ctrl Pts',(-82.5,-18.3601861194615,-39.2957805952595));
#48486=CARTESIAN_POINT('Ctrl Pts',(-82.1335529047565,-17.9981538334961,
-40.0817756896715));
#48487=CARTESIAN_POINT('Ctrl Pts',(-82.3033638472202,-18.105823384275,-39.8479876950582));
#48488=CARTESIAN_POINT('Ctrl Pts',(-82.4723016530939,-18.2137706603509,
-39.6136883524303));
#48489=CARTESIAN_POINT('Ctrl Pts',(-82.6402844586922,-18.321949249316,-39.3787952697101));
#48490=CARTESIAN_POINT('Ctrl Pts',(-82.2718712623887,-17.8763922960829,
-40.1264553284945));
#48491=CARTESIAN_POINT('Ctrl Pts',(-82.4415798905547,-17.9847127199064,
-39.8923864556503));
#48492=CARTESIAN_POINT('Ctrl Pts',(-82.6104201575495,-18.0933094945676,
-39.6578020950152));
#48493=CARTESIAN_POINT('Ctrl Pts',(-82.7782997031823,-18.2021497484197,
-39.422614172472));
#48494=CARTESIAN_POINT('Ctrl Pts',(-82.3464466094067,-17.725858020119,-40.1114460276889));
#48495=CARTESIAN_POINT('Ctrl Pts',(-82.5163877113353,-17.834738696598,-39.8775346251281));
#48496=CARTESIAN_POINT('Ctrl Pts',(-82.6854396968589,-17.9438814031046,
-39.6430704062622));
#48497=CARTESIAN_POINT('Ctrl Pts',(-82.8535533905932,-18.0532959647562,
-39.4080313955299));
#48498=CARTESIAN_POINT('',(-82.5,-18.3601861194615,-39.2957805952595));
#48499=CARTESIAN_POINT('',(-82.8535533905932,-18.0532959647562,-39.4080313955299));
#48500=CARTESIAN_POINT('Origin',(-82.5,-17.9060450480377,-39.0866015158896));
#48501=CARTESIAN_POINT('',(-82.3464466094067,-17.725858020119,-40.1114460276889));
#48502=CARTESIAN_POINT('Ctrl Pts',(-82.8535533905932,-18.0532959647562,
-39.4080313955299));
#48503=CARTESIAN_POINT('Ctrl Pts',(-82.6854396968589,-17.9438814031046,
-39.6430704062622));
#48504=CARTESIAN_POINT('Ctrl Pts',(-82.5163877113353,-17.834738696598,-39.8775346251281));
#48505=CARTESIAN_POINT('Ctrl Pts',(-82.3464466094067,-17.725858020119,-40.1114460276889));
#48506=CARTESIAN_POINT('Origin',(-81.9928932188135,-17.5829497100816,-39.7880620223296));
#48507=CARTESIAN_POINT('Ctrl Pts',(-81.9928932188135,-18.0370907815054,
-39.9972411016994));
#48508=CARTESIAN_POINT('Ctrl Pts',(-82.162834320742,-18.1445398492965,-39.7639623487899));
#48509=CARTESIAN_POINT('Ctrl Pts',(-82.3318863062657,-18.2522350868817,
-39.5301491456174));
#48510=CARTESIAN_POINT('Ctrl Pts',(-82.5,-18.3601861194615,-39.2957805952595));
#48511=CARTESIAN_POINT('Origin',(-82.5,-17.9060450480377,-39.0866015158896));
#48512=CARTESIAN_POINT('Origin',(-82.5,-17.9060450480377,-39.0866015158896));
#48513=CARTESIAN_POINT('Origin',(-82.5,-17.9060450480377,-39.0866015158896));
#48514=CARTESIAN_POINT('Origin',(-81.9928932188135,-17.5829497100816,-39.7880620223295));
#48515=CARTESIAN_POINT('Origin',(-81.9928932188135,-17.5829497100816,-39.7880620223295));
#48516=CARTESIAN_POINT('Origin',(-81.9928932188135,0.,0.));
#48517=CARTESIAN_POINT('',(-82.3464466094067,33.1604609492284,-28.6970028856031));
#48518=CARTESIAN_POINT('Origin',(-82.3464466094067,2.22044604925031E-15,
0.));
#48519=CARTESIAN_POINT('Origin',(-81.9928932188135,32.8931167434394,-28.4656436938016));
#48520=CARTESIAN_POINT('Origin',(-82.6,0.,0.));
#48521=CARTESIAN_POINT('',(-82.8535533905933,32.005083342152,-29.2333555023034));
#48522=CARTESIAN_POINT('Origin',(-82.8535533905933,2.22044604925031E-15,
0.));
#48523=CARTESIAN_POINT('Ctrl Pts',(-82.3464466094067,33.1604609492285,-28.6970028856031));
#48524=CARTESIAN_POINT('Ctrl Pts',(-82.519891807541,32.777021289468,-28.8750301042473));
#48525=CARTESIAN_POINT('Ctrl Pts',(-82.6890303136401,32.3919000078227,-29.0538137165052));
#48526=CARTESIAN_POINT('Ctrl Pts',(-82.8535533905933,32.005083342152,-29.2333555023034));
#48527=CARTESIAN_POINT('Origin',(-76.5,0.,0.));
#48528=CARTESIAN_POINT('',(-77.,-18.2783610671109,-39.4734279826357));
#48529=CARTESIAN_POINT('Origin',(-77.,0.,0.));
#48530=CARTESIAN_POINT('Ctrl Pts',(-76.8294181454571,-18.0370907815373,
-39.99724110163));
#48531=CARTESIAN_POINT('Ctrl Pts',(-76.8802846591861,-18.065500682451,-39.9355614017345));
#48532=CARTESIAN_POINT('Ctrl Pts',(-76.9231860633659,-18.1032378673816,
-39.8536315756326));
#48533=CARTESIAN_POINT('Ctrl Pts',(-76.9817250649226,-18.1795903983193,
-39.6878653799385));
#48534=CARTESIAN_POINT('Ctrl Pts',(-77.,-18.233218835034,-39.5714346365688));
#48535=CARTESIAN_POINT('Ctrl Pts',(-77.,-18.2783610671109,-39.4734279826356));
#48536=CARTESIAN_POINT('Origin',(-77.,-23.8767458057638,-34.489868218463));
#48537=CARTESIAN_POINT('',(-77.,-29.9484575042249,-28.4786855519014));
#48538=CARTESIAN_POINT('',(-77.,-23.2547269643883,-43.0111998374633));
#48539=CARTESIAN_POINT('',(-77.,-24.4987646471392,-25.9685365994627));
#48540=CARTESIAN_POINT('Origin',(-77.,-27.2236110756821,-27.2236110756821));
#48541=CARTESIAN_POINT('',(-77.,-24.4987646471392,-25.9685365994627));
#48542=CARTESIAN_POINT('',(-77.,-27.2236110756821,-25.4736110756821));
#48543=CARTESIAN_POINT('Origin',(-77.,-27.2236110756821,-27.2236110756821));
#48544=CARTESIAN_POINT('Origin',(-81.9928932188135,32.8931167434394,-28.4656436938016));
#48545=CARTESIAN_POINT('',(-81.9928932188135,32.6839376640695,-28.0115026223778));
#48546=CARTESIAN_POINT('Origin',(-81.9928932188135,32.8931167434394,-28.4656436938016));
#48547=CARTESIAN_POINT('Origin',(-81.9928932188135,32.8931167434394,-28.4656436938016));
#48548=CARTESIAN_POINT('Ctrl Pts',(-82.5,31.5348562042457,-28.5407738489008));
#48549=CARTESIAN_POINT('Ctrl Pts',(-82.3354769230468,31.9195086345245,-28.3636014980477));
#48550=CARTESIAN_POINT('Ctrl Pts',(-82.1663384169477,32.3025319745614,-28.187179512265));
#48551=CARTESIAN_POINT('Ctrl Pts',(-81.9928932188134,32.6839376640695,-28.0115026223778));
#48552=CARTESIAN_POINT('Ctrl Pts',(-82.601222396877,31.5705733306819,-28.5243224066161));
#48553=CARTESIAN_POINT('Ctrl Pts',(-82.4362687847223,31.9558428996681,-28.3468682536414));
#48554=CARTESIAN_POINT('Ctrl Pts',(-82.2666963849679,32.3394554127185,-28.1701699721031));
#48555=CARTESIAN_POINT('Ctrl Pts',(-82.092822276946,32.7214270614466,-27.9942348654562));
#48556=CARTESIAN_POINT('Ctrl Pts',(-82.8034223550171,31.6726547394673,-28.5581838001894));
#48557=CARTESIAN_POINT('Ctrl Pts',(-82.6376068788958,32.0590643026922,-28.3799607867701));
#48558=CARTESIAN_POINT('Ctrl Pts',(-82.4671755774271,32.4437642452149,-28.2025206678114));
#48559=CARTESIAN_POINT('Ctrl Pts',(-82.292442868024,32.8267719980494,-28.0258606826798));
#48560=CARTESIAN_POINT('Ctrl Pts',(-82.9826254704188,31.8549987460867,-28.7876553692672));
#48561=CARTESIAN_POINT('Ctrl Pts',(-82.8163922951542,32.2423193330201,-28.6082165351974));
#48562=CARTESIAN_POINT('Ctrl Pts',(-82.6455413767597,32.62788700097,-28.4295675191164));
#48563=CARTESIAN_POINT('Ctrl Pts',(-82.4703909000744,33.0117234325711,-28.2517145087475));
#48564=CARTESIAN_POINT('Ctrl Pts',(-82.9669916294051,31.9689903150268,-29.0496559660236));
#48565=CARTESIAN_POINT('Ctrl Pts',(-82.8014521794668,32.356263090383,-28.8697787064162));
#48566=CARTESIAN_POINT('Ctrl Pts',(-82.6312976191216,32.7417993370319,-28.6906846525606));
#48567=CARTESIAN_POINT('Ctrl Pts',(-82.4568372375248,33.1256165821777,-28.5123652578115));
#48568=CARTESIAN_POINT('Ctrl Pts',(-82.8865299173878,31.9994877358,-29.1905849277686));
#48569=CARTESIAN_POINT('Ctrl Pts',(-82.7217413694523,32.3864366561427,-29.0109211273876));
#48570=CARTESIAN_POINT('Ctrl Pts',(-82.5523328763366,32.7716795239154,-28.8320162434955));
#48571=CARTESIAN_POINT('Ctrl Pts',(-82.3786222724039,33.1552296116972,-28.6538783963964));
#48572=CARTESIAN_POINT('Ctrl Pts',(-82.8535533905933,32.005083342152,-29.2333555023034));
#48573=CARTESIAN_POINT('Ctrl Pts',(-82.6890303136401,32.3919000078227,-29.0538137165052));
#48574=CARTESIAN_POINT('Ctrl Pts',(-82.519891807541,32.777021289468,-28.8750301042473));
#48575=CARTESIAN_POINT('Ctrl Pts',(-82.3464466094067,33.1604609492285,-28.6970028856031));
#48576=CARTESIAN_POINT('',(-82.5,31.5348562042457,-28.5407738489008));
#48577=CARTESIAN_POINT('Origin',(-82.5,31.7440352836156,-28.9949149203246));
#48578=CARTESIAN_POINT('Ctrl Pts',(-82.5,31.5348562042457,-28.5407738489008));
#48579=CARTESIAN_POINT('Ctrl Pts',(-82.3354769230468,31.9195086345245,-28.3636014980477));
#48580=CARTESIAN_POINT('Ctrl Pts',(-82.1663384169477,32.3025319745614,-28.187179512265));
#48581=CARTESIAN_POINT('Ctrl Pts',(-81.9928932188134,32.6839376640695,-28.0115026223778));
#48582=CARTESIAN_POINT('Origin',(-75.,32.8931167434394,-28.4656436938016));
#48583=CARTESIAN_POINT('',(-77.,33.2181297628261,-28.0856877263144));
#48584=CARTESIAN_POINT('Ctrl Pts',(-76.5,33.2711985450881,-28.792835000627));
#48585=CARTESIAN_POINT('Ctrl Pts',(-76.500911294617,33.2717982978639,-28.7921419638461));
#48586=CARTESIAN_POINT('Ctrl Pts',(-76.5018225908797,33.272396146182,-28.7914472767637));
#48587=CARTESIAN_POINT('Ctrl Pts',(-76.5561204583968,33.3079042592016,-28.7499574103998));
#48588=CARTESIAN_POINT('Ctrl Pts',(-76.6098195625408,33.3364800964727,-28.7032660033553));
#48589=CARTESIAN_POINT('Ctrl Pts',(-76.712202600818,33.3770567140056,-28.6023347905465));
#48590=CARTESIAN_POINT('Ctrl Pts',(-76.7616726361363,33.389729530025,-28.5476297045151));
#48591=CARTESIAN_POINT('Ctrl Pts',(-76.8500872540886,33.3951790166874,-28.4352133445057));
#48592=CARTESIAN_POINT('Ctrl Pts',(-76.8899964255655,33.3890059164671,-28.377121742794));
#48593=CARTESIAN_POINT('Ctrl Pts',(-76.9474081328343,33.3573297979245,-28.2741355363395));
#48594=CARTESIAN_POINT('Ctrl Pts',(-76.9678406878704,33.3368297278632,-28.2296235623672));
#48595=CARTESIAN_POINT('Ctrl Pts',(-76.9935652964059,33.283595547211,-28.1501559864099));
#48596=CARTESIAN_POINT('Ctrl Pts',(-77.,33.2533411811838,-28.1158074516948));
#48597=CARTESIAN_POINT('Ctrl Pts',(-77.,33.2181297628261,-28.0856877263145));
#48598=CARTESIAN_POINT('',(-77.,32.6839376640695,-28.0115026223778));
#48599=CARTESIAN_POINT('',(-75.,32.6839376640695,-28.0115026223778));
#48600=CARTESIAN_POINT('Origin',(-77.,32.8931167434394,-28.4656436938016));
#48601=CARTESIAN_POINT('Origin',(-82.5,0.,0.));
#48602=CARTESIAN_POINT('Origin',(-82.5,31.7440352836156,-28.9949149203246));
#48603=CARTESIAN_POINT('Origin',(-82.5,-19.7071756188355,-35.1762326125546));
#48604=CARTESIAN_POINT('',(-82.5,-24.4987646471392,-25.9685365994627));
#48605=CARTESIAN_POINT('',(-82.5,-20.1613166902593,-35.3854116919245));
#48606=CARTESIAN_POINT('Origin',(-82.5,-24.0446235757154,-25.7593575200928));
#48607=CARTESIAN_POINT('Origin',(-82.5,-27.2236110756821,-27.2236110756821));
#48608=CARTESIAN_POINT('',(-82.5,-29.9484575042249,-28.4786855519014));
#48609=CARTESIAN_POINT('Origin',(-82.5,-30.4025985756487,-28.6878646312713));
#48610=CARTESIAN_POINT('Origin',(-82.5,-27.2236110756821,-27.2236110756821));
#48611=CARTESIAN_POINT('Origin',(-82.5,-29.4120158886871,-30.8384825809522));
#48612=CARTESIAN_POINT('',(-82.5,-28.9578748172633,-30.6293035015823));
#48613=CARTESIAN_POINT('Origin',(-82.5,31.7440352836156,-28.9949149203246));
#48614=CARTESIAN_POINT('Origin',(-82.5,31.7440352836156,-28.9949149203246));
#48615=CARTESIAN_POINT('Origin',(-83.,-17.8050341073026,-40.5010508850245));
#48616=CARTESIAN_POINT('',(-83.,-24.4987646471392,-25.9685365994627));
#48617=CARTESIAN_POINT('Origin',(-83.,28.4786855519014,-29.9484575042249));
#48618=CARTESIAN_POINT('',(-82.5,28.4786855519014,-29.9484575042249));
#48619=CARTESIAN_POINT('',(-82.5,40.2410703537288,-24.530658985525));
#48620=CARTESIAN_POINT('',(-77.,28.4786855519014,-29.9484575042249));
#48621=CARTESIAN_POINT('',(-83.,28.4786855519014,-29.9484575042249));
#48622=CARTESIAN_POINT('',(-77.,43.0111998374633,-23.2547269643883));
#48623=CARTESIAN_POINT('Origin',(-82.5,40.4502494330987,-24.9848000569488));
#48624=CARTESIAN_POINT('Origin',(-82.5,28.6878646312713,-30.4025985756487));
#48625=CARTESIAN_POINT('Origin',(-82.5,27.2236110756821,-27.2236110756821));
#48626=CARTESIAN_POINT('Origin',(-82.5,27.2236110756821,-27.2236110756821));
#48627=CARTESIAN_POINT('Origin',(-83.,27.2236110756821,-27.2236110756821));
#48628=CARTESIAN_POINT('Origin',(-77.,27.2236110756821,-27.2236110756821));
#48629=CARTESIAN_POINT('Origin',(-76.5,-27.2236110756821,-27.2236110756821));
#48630=CARTESIAN_POINT('',(-76.5,-27.2236110756821,-25.9736110756821));
#48631=CARTESIAN_POINT('Origin',(-76.5,-27.2236110756821,-25.4736110756821));
#48632=CARTESIAN_POINT('Origin',(-76.5,-27.2236110756821,-27.2236110756821));
#48633=CARTESIAN_POINT('Origin',(-83.,-27.2236110756821,-27.2236110756821));
#48634=CARTESIAN_POINT('',(-67.5,-27.2236110756821,-25.9736110756821));
#48635=CARTESIAN_POINT('',(-83.,-27.2236110756821,-25.9736110756821));
#48636=CARTESIAN_POINT('',(-67.5,-27.2236110756821,-28.4736110756821));
#48637=CARTESIAN_POINT('Origin',(-67.5,-27.2236110756821,-27.2236110756821));
#48638=CARTESIAN_POINT('Origin',(-67.5,-27.2236110756821,-27.2236110756821));
#48639=CARTESIAN_POINT('Origin',(-10.5,-26.1629509039023,-33.9411254969543));
#48640=CARTESIAN_POINT('',(-10.5,-25.809397513309,-34.2946788875476));
#48641=CARTESIAN_POINT('',(-10.,-26.1629509039023,-33.9411254969543));
#48642=CARTESIAN_POINT('Origin',(-10.5,-26.1629509039023,-33.9411254969543));
#48643=CARTESIAN_POINT('',(-10.5,-26.5165042944955,-34.2946788875476));
#48644=CARTESIAN_POINT('Origin',(-10.5,-26.1629509039023,-33.9411254969543));
#48645=CARTESIAN_POINT('Origin',(-10.5,-26.1629509039023,-33.9411254969543));
#48646=CARTESIAN_POINT('Origin',(-10.5,-23.4052344572747,-31.1834090503267));
#48647=CARTESIAN_POINT('',(-10.5,-21.708178182427,-30.1934595566656));
#48648=CARTESIAN_POINT('',(-10.,-22.4152849636136,-30.1934595566656));
#48649=CARTESIAN_POINT('Origin',(-10.5,-22.0617315730203,-29.8399061660723));
#48650=CARTESIAN_POINT('',(-10.,-23.4052344572747,-31.1834090503267));
#48651=CARTESIAN_POINT('',(-10.5,-23.0516810666815,-31.53696244092));
#48652=CARTESIAN_POINT('Origin',(-14.,-22.0617315730203,-30.5470129472589));
#48653=CARTESIAN_POINT('',(-6.70710678118655,-21.708178182427,-30.1934595566656));
#48654=CARTESIAN_POINT('',(-14.,-21.708178182427,-30.1934595566656));
#48655=CARTESIAN_POINT('',(-14.,-25.809397513309,-34.2946788875476));
#48656=CARTESIAN_POINT('',(-14.,-25.809397513309,-34.2946788875476));
#48657=CARTESIAN_POINT('',(-14.,-18.031222920257,-26.5165042944955));
#48658=CARTESIAN_POINT('',(-14.,-5.90954544295051,-14.3948268171891));
#48659=CARTESIAN_POINT('',(-6.70710678118654,-18.031222920257,-26.5165042944955));
#48660=CARTESIAN_POINT('',(-14.,-18.031222920257,-26.5165042944955));
#48661=CARTESIAN_POINT('',(-6.70710678118654,-21.5137238176007,-29.9990051918393));
#48662=CARTESIAN_POINT('Origin',(-14.,-26.1629509039023,-33.9411254969543));
#48663=CARTESIAN_POINT('',(-14.,-26.5165042944955,-34.2946788875476));
#48664=CARTESIAN_POINT('',(-14.,-26.5165042944955,-34.2946788875476));
#48665=CARTESIAN_POINT('Origin',(-14.,-26.1629509039023,-33.9411254969543));
#48666=CARTESIAN_POINT('Origin',(-6.5,-20.9177083067616,-28.4029896810001));
#48667=CARTESIAN_POINT('',(-6.01703708685547,-22.0617315730203,-29.7300256491511));
#48668=CARTESIAN_POINT('',(-6.14644660940673,-21.8117315730203,-29.7970129472589));
#48669=CARTESIAN_POINT('Origin',(-6.5,-22.0617315730203,-29.5470129472589));
#48670=CARTESIAN_POINT('',(-6.14644660940673,-18.4276695296637,-26.4129509039022));
#48671=CARTESIAN_POINT('',(-6.14644660940673,-20.6677083067616,-28.6529896810001));
#48672=CARTESIAN_POINT('',(-6.01703708685546,-18.4946568277715,-26.1629509039023));
#48673=CARTESIAN_POINT('Origin',(-6.5,-18.6776695296637,-26.1629509039023));
#48674=CARTESIAN_POINT('',(-6.,-18.6776695296637,-26.1629509039023));
#48675=CARTESIAN_POINT('Origin',(-6.5,-18.6776695296637,-26.1629509039023));
#48676=CARTESIAN_POINT('',(-6.,-22.0617315730203,-29.5470129472589));
#48677=CARTESIAN_POINT('',(-6.,-20.9177083067616,-28.4029896810001));
#48678=CARTESIAN_POINT('Origin',(-6.5,-22.0617315730203,-29.5470129472589));
#48679=CARTESIAN_POINT('Origin',(-5.80473785412436,-19.6609186857656,-26.1629509039022));
#48680=CARTESIAN_POINT('',(-6.35355339059327,-18.1347763108502,-26.4129509039023));
#48681=CARTESIAN_POINT('',(-5.45118446353109,-19.4109186857656,-26.4129509039022));
#48682=CARTESIAN_POINT('',(-6.35355339059327,-18.1347763108502,-25.9129509039023));
#48683=CARTESIAN_POINT('Origin',(-6.70710678118655,-18.3847763108502,-26.1629509039023));
#48684=CARTESIAN_POINT('',(-6.14644660940673,-18.4276695296637,-25.9129509039023));
#48685=CARTESIAN_POINT('',(-5.45118446353109,-19.4109186857656,-25.9129509039023));
#48686=CARTESIAN_POINT('Origin',(-6.5,-18.6776695296637,-26.1629509039022));
#48687=CARTESIAN_POINT('Origin',(-6.25,-21.1424927574778,-29.2742207411231));
#48688=CARTESIAN_POINT('',(-6.35355339059327,-21.8117315730203,-30.0899061660723));
#48689=CARTESIAN_POINT('',(-5.93451779686442,-21.8117315730203,-29.4973003463039));
#48690=CARTESIAN_POINT('',(-6.35355339059327,-21.617277208194,-29.895451801246));
#48691=CARTESIAN_POINT('Origin',(-6.2880711874577,-22.0617315730203,-29.2473003463039));
#48692=CARTESIAN_POINT('',(-6.14644660940672,-22.3117315730203,-29.7970129472588));
#48693=CARTESIAN_POINT('Origin',(-6.5,-22.0617315730203,-29.5470129472589));
#48694=CARTESIAN_POINT('',(-6.35355339059327,-22.3117315730203,-30.0899061660723));
#48695=CARTESIAN_POINT('',(-5.93451779686442,-22.3117315730203,-29.4973003463039));
#48696=CARTESIAN_POINT('Origin',(-6.70710678118654,-22.0617315730203,-29.8399061660723));
#48697=CARTESIAN_POINT('Origin',(-6.70710678118654,-21.867277208194,-29.645451801246));
#48698=CARTESIAN_POINT('Origin',(-6.70710678118654,-22.0617315730203,-29.8399061660723));
#48699=CARTESIAN_POINT('Origin',(-6.70710678118654,-18.3847763108502,-26.1629509039023));
#48700=CARTESIAN_POINT('Origin',(-6.25,-19.97576656852,-24.2184072556392));
#48701=CARTESIAN_POINT('',(-6.35355339059327,-25.9129509039023,-18.1347763108502));
#48702=CARTESIAN_POINT('',(-6.35355339059327,-18.8418830920368,-25.2058441227157));
#48703=CARTESIAN_POINT('',(-6.14644660940673,-25.9129509039023,-18.4276695296637));
#48704=CARTESIAN_POINT('',(-4.69285113019775,-25.9129509039023,-20.4833639705652));
#48705=CARTESIAN_POINT('',(-6.14644660940673,-21.1096500450032,-23.2309703885628));
#48706=CARTESIAN_POINT('Origin',(-6.25,-28.2489159084026,-24.0062752212833));
#48707=CARTESIAN_POINT('',(-6.14644660940672,-30.0250855260513,-22.0836589942278));
#48708=CARTESIAN_POINT('',(-6.14644660940672,-27.1150324319194,-24.9937120883597));
#48709=CARTESIAN_POINT('',(-6.35355339059327,-30.1934595566656,-22.208178182427));
#48710=CARTESIAN_POINT('Origin',(-6.,-29.3399061660723,-22.5617315730203));
#48711=CARTESIAN_POINT('',(-6.35355339059327,-29.3827993848858,-23.0188383542068));
#48712=CARTESIAN_POINT('Origin',(-6.5,-26.8650324319194,-24.7437120883597));
#48713=CARTESIAN_POINT('',(-6.,-29.5470129472589,-22.0617315730203));
#48714=CARTESIAN_POINT('',(-6.,-26.8650324319194,-24.7437120883597));
#48715=CARTESIAN_POINT('',(-6.09270987511341,-29.9571708538506,-22.0617315730203));
#48716=CARTESIAN_POINT('Origin',(-6.5,-29.5470129472589,-22.0617315730203));
#48717=CARTESIAN_POINT('Ctrl Pts',(-6.09270987511341,-29.9571708538506,
-22.0617315730203));
#48718=CARTESIAN_POINT('Ctrl Pts',(-6.10696729553699,-29.9780430792037,
-22.0691748156934));
#48719=CARTESIAN_POINT('Ctrl Pts',(-6.12280773614487,-29.9982570735517,
-22.0759673093509));
#48720=CARTESIAN_POINT('Ctrl Pts',(-6.14208599488146,-30.0202233077774,
-22.0822967086671));
#48721=CARTESIAN_POINT('Ctrl Pts',(-6.14425676103634,-30.0226594227913,
-22.0829881842228));
#48722=CARTESIAN_POINT('Ctrl Pts',(-6.14644660940672,-30.0250855260513,
-22.0836589942278));
#48723=CARTESIAN_POINT('Origin',(-76.5,0.,0.));
#48724=CARTESIAN_POINT('Origin',(-77.,0.,0.));
#48725=CARTESIAN_POINT('Origin',(-77.,23.8767458057638,34.489868218463));
#48726=CARTESIAN_POINT('Origin',(-77.,27.2236110756821,27.2236110756821));
#48727=CARTESIAN_POINT('',(-77.,27.2236110756821,28.9736110756821));
#48728=CARTESIAN_POINT('Origin',(-77.,27.2236110756821,27.2236110756821));
#48729=CARTESIAN_POINT('Origin',(-76.5,27.2236110756821,27.2236110756821));
#48730=CARTESIAN_POINT('',(-76.5,27.2236110756821,28.4736110756821));
#48731=CARTESIAN_POINT('Origin',(-76.5,27.2236110756821,28.9736110756821));
#48732=CARTESIAN_POINT('Origin',(-76.5,27.2236110756821,27.2236110756821));
#48733=CARTESIAN_POINT('Origin',(-83.,27.2236110756821,27.2236110756821));
#48734=CARTESIAN_POINT('',(-67.5,27.2236110756821,28.4736110756821));
#48735=CARTESIAN_POINT('',(-83.,27.2236110756821,28.4736110756821));
#48736=CARTESIAN_POINT('',(-67.5,27.2236110756821,25.9736110756821));
#48737=CARTESIAN_POINT('Origin',(-67.5,27.2236110756821,27.2236110756821));
#48738=CARTESIAN_POINT('Origin',(-67.5,27.2236110756821,27.2236110756821));
#48739=CARTESIAN_POINT('Origin',(-14.,-18.3847763108502,-26.1629509039023));
#48740=CARTESIAN_POINT('',(-6.70710678118654,-18.031222920257,-25.809397513309));
#48741=CARTESIAN_POINT('Origin',(-6.70710678118654,-18.3847763108502,-26.1629509039023));
#48742=CARTESIAN_POINT('',(-14.,-18.031222920257,-25.809397513309));
#48743=CARTESIAN_POINT('Origin',(-14.,-18.3847763108502,-26.1629509039023));
#48744=CARTESIAN_POINT('',(-14.,-18.031222920257,-25.809397513309));
#48745=CARTESIAN_POINT('Origin',(-6.70710678118654,-18.3847763108502,-26.1629509039023));
#48746=CARTESIAN_POINT('Origin',(-6.70710678118654,-18.3847763108502,-26.1629509039023));
#48747=CARTESIAN_POINT('Origin',(-14.,-22.0617315730203,-29.8399061660723));
#48748=CARTESIAN_POINT('',(-6.70710678118655,-22.4152849636136,-30.1934595566656));
#48749=CARTESIAN_POINT('Origin',(-6.70710678118655,-22.0617315730203,-29.8399061660723));
#48750=CARTESIAN_POINT('',(-14.,-22.4152849636136,-30.1934595566656));
#48751=CARTESIAN_POINT('Origin',(-6.70710678118655,-22.0617315730203,-29.8399061660723));
#48752=CARTESIAN_POINT('Origin',(-6.70710678118655,-22.0617315730203,-29.8399061660723));
#48753=CARTESIAN_POINT('Origin',(-6.70710678118654,-19.0918830920368,-25.4558441227157));
#48754=CARTESIAN_POINT('',(-6.70710678118654,-25.809397513309,-18.031222920257));
#48755=CARTESIAN_POINT('',(-6.70710678118654,-18.7383297014435,-25.1022907321224));
#48756=CARTESIAN_POINT('Origin',(-6.70710678118655,-26.1629509039023,-18.3847763108502));
#48757=CARTESIAN_POINT('Origin',(-6.70710678118654,-26.1629509039023,-18.3847763108502));
#48758=CARTESIAN_POINT('',(-6.35355339059327,-26.4129509039023,-18.1347763108502));
#48759=CARTESIAN_POINT('',(-6.70710678118655,-26.5165042944955,-18.031222920257));
#48760=CARTESIAN_POINT('Origin',(-6.70710678118655,-26.1629509039023,-18.3847763108502));
#48761=CARTESIAN_POINT('Origin',(-6.70710678118654,-26.1629509039023,-18.3847763108502));
#48762=CARTESIAN_POINT('Origin',(-6.70710678118654,-26.1629509039023,-18.3847763108502));
#48763=CARTESIAN_POINT('Origin',(-14.,-26.1629509039023,-18.3847763108502));
#48764=CARTESIAN_POINT('',(-14.,-25.809397513309,-18.031222920257));
#48765=CARTESIAN_POINT('',(-14.,-25.809397513309,-18.031222920257));
#48766=CARTESIAN_POINT('',(-14.,-26.5165042944955,-18.031222920257));
#48767=CARTESIAN_POINT('Origin',(-14.,-26.1629509039023,-18.3847763108502));
#48768=CARTESIAN_POINT('',(-14.,-26.5165042944955,-18.031222920257));
#48769=CARTESIAN_POINT('Origin',(-14.,-17.6776695296637,-26.1629509039023));
#48770=CARTESIAN_POINT('',(-14.,-16.7989898732233,-27.0416305603426));
#48771=CARTESIAN_POINT('Origin',(-6.5,-21.3596500450032,-23.4809703885628));
#48772=CARTESIAN_POINT('',(-6.,-26.1629509039023,-18.6776695296637));
#48773=CARTESIAN_POINT('Origin',(-6.5,-26.1629509039023,-18.6776695296637));
#48774=CARTESIAN_POINT('',(-6.,-21.3596500450032,-23.4809703885628));
#48775=CARTESIAN_POINT('Origin',(-5.04640452079102,-26.1629509039023,-20.7333639705652));
#48776=CARTESIAN_POINT('',(-6.14644660940673,-26.4129509039023,-18.4276695296637));
#48777=CARTESIAN_POINT('',(-4.69285113019775,-26.4129509039023,-20.4833639705652));
#48778=CARTESIAN_POINT('Origin',(-6.5,-26.1629509039023,-18.6776695296637));
#48779=CARTESIAN_POINT('Origin',(-6.5,-26.1629509039023,-18.6776695296637));
#48780=CARTESIAN_POINT('Origin',(-6.5,-26.1629509039023,-18.6776695296637));
#48781=CARTESIAN_POINT('Origin',(-6.,-24.1123412384613,-24.1123412384613));
#48782=CARTESIAN_POINT('',(-6.,-27.306974170161,-19.8216927959224));
#48783=CARTESIAN_POINT('Origin',(-6.5,-27.306974170161,-19.8216927959224));
#48784=CARTESIAN_POINT('',(-6.14644660940673,-29.9434595566656,-21.958178182427));
#48785=CARTESIAN_POINT('',(-6.14644660940673,-27.556974170161,-19.5716927959224));
#48786=CARTESIAN_POINT('Origin',(-6.5,-29.6934595566656,-22.208178182427));
#48787=CARTESIAN_POINT('Origin',(-6.25,-27.0821897194448,-18.9504617357995));
#48788=CARTESIAN_POINT('',(-6.35355339059327,-30.0899061660723,-21.8117315730203));
#48789=CARTESIAN_POINT('',(-6.35355339059327,-26.6074052687286,-18.3292306756765));
#48790=CARTESIAN_POINT('',(-10.25,-32.8451099861151,-19.0565277529775));
#48791=CARTESIAN_POINT('Origin',(-73.,0.,0.));
#48792=CARTESIAN_POINT('',(-73.,-44.,5.38844591624836E-15));
#48793=CARTESIAN_POINT('',(-73.,-5.38844591624836E-15,44.));
#48794=CARTESIAN_POINT('Origin',(-73.,0.,0.));
#48795=CARTESIAN_POINT('',(-73.5,-5.32721357629099E-15,43.5));
#48796=CARTESIAN_POINT('Origin',(-73.,-5.32721357629099E-15,43.5));
#48797=CARTESIAN_POINT('Origin',(-73.5,0.,0.));
#48798=CARTESIAN_POINT('Origin',(-73.,0.,0.));
#48799=CARTESIAN_POINT('Origin',(-75.,0.,0.));
#48800=CARTESIAN_POINT('',(-68.0071067811866,-44.,-5.38844591624836E-15));
#48801=CARTESIAN_POINT('',(-68.0071067811866,-5.38844591624836E-15,44.));
#48802=CARTESIAN_POINT('Origin',(-68.0071067811866,0.,0.));
#48803=CARTESIAN_POINT('',(-75.,-44.,-5.38844591624836E-15));
#48804=CARTESIAN_POINT('Origin',(-68.0071067811866,0.,0.));
#48805=CARTESIAN_POINT('Origin',(-73.5,42.4,0.));
#48806=CARTESIAN_POINT('',(-73.5,-42.4,-5.19250242838478E-15));
#48807=CARTESIAN_POINT('Origin',(-73.5,0.,0.));
#48808=CARTESIAN_POINT('Origin',(-68.0071067811866,0.,0.));
#48809=CARTESIAN_POINT('',(-67.6535533905933,-5.37051137910276E-15,43.8535533905933));
#48810=CARTESIAN_POINT('',(-67.6535533905933,-43.8535533905933,-5.37051137910276E-15));
#48811=CARTESIAN_POINT('Origin',(-67.6535533905933,0.,-6.71313922387845E-15));
#48812=CARTESIAN_POINT('Origin',(-67.6535533905933,0.,-6.71313922387845E-15));
#48813=CARTESIAN_POINT('Origin',(-68.0071067811866,-5.32721357629099E-15,
43.5));
#48814=CARTESIAN_POINT('Origin',(-67.4,0.,0.));
#48815=CARTESIAN_POINT('',(-67.1464466094067,-43.3464466094067,-5.30840870946216E-15));
#48816=CARTESIAN_POINT('',(-67.1464466094067,-5.30840870946216E-15,43.3464466094067));
#48817=CARTESIAN_POINT('Origin',(-67.1464466094067,0.,-6.6355108868277E-15));
#48818=CARTESIAN_POINT('',(-67.4,-43.6,-5.33946004428246E-15));
#48819=CARTESIAN_POINT('Origin',(-67.1464466094067,0.,-6.6355108868277E-15));
#48820=CARTESIAN_POINT('Origin',(-76.5,0.,0.));
#48821=CARTESIAN_POINT('Origin',(-77.,0.,0.));
#48822=CARTESIAN_POINT('Origin',(-77.,-34.489868218463,23.8767458057638));
#48823=CARTESIAN_POINT('Origin',(-77.,-27.2236110756821,27.2236110756821));
#48824=CARTESIAN_POINT('',(-77.,-27.2236110756821,28.9736110756821));
#48825=CARTESIAN_POINT('Origin',(-77.,-27.2236110756821,27.2236110756821));
#48826=CARTESIAN_POINT('Origin',(-76.5,0.,0.));
#48827=CARTESIAN_POINT('Origin',(-77.,0.,0.));
#48828=CARTESIAN_POINT('Origin',(-77.,34.489868218463,-23.8767458057638));
#48829=CARTESIAN_POINT('',(-77.,27.2236110756821,-25.4736110756821));
#48830=CARTESIAN_POINT('Origin',(-77.,27.2236110756821,-27.2236110756821));
#48831=CARTESIAN_POINT('Origin',(-10.6035533905933,-32.5951099861151,-19.3065277529775));
#48832=CARTESIAN_POINT('',(-6.70710678118655,-30.1934595566656,-22.4152849636136));
#48833=CARTESIAN_POINT('Origin',(-6.70710678118655,-29.8399061660723,-22.0617315730203));
#48834=CARTESIAN_POINT('Origin',(-6.70710678118655,-29.8399061660723,-22.0617315730203));
#48835=CARTESIAN_POINT('Origin',(-6.70710678118655,-29.1327993848858,-22.7688383542068));
#48836=CARTESIAN_POINT('',(-6.70710678118655,-29.486352775479,-23.1223917448001));
#48837=CARTESIAN_POINT('Origin',(-14.,-30.5470129472589,-22.0617315730203));
#48838=CARTESIAN_POINT('',(-10.,-30.1934595566656,-22.4152849636136));
#48839=CARTESIAN_POINT('',(-14.,-30.1934595566656,-22.4152849636136));
#48840=CARTESIAN_POINT('',(-10.,-28.4256926036992,-24.1830519165799));
#48841=CARTESIAN_POINT('Origin',(-6.70710678118655,-26.3574052687286,-18.5792306756765));
#48842=CARTESIAN_POINT('',(-6.70710678118655,-30.1934595566656,-21.708178182427));
#48843=CARTESIAN_POINT('',(-6.70710678118655,-26.7109586593218,-18.2256772850833));
#48844=CARTESIAN_POINT('Origin',(-6.70710678118655,-29.8399061660723,-22.0617315730203));
#48845=CARTESIAN_POINT('Origin',(-6.70710678118655,-29.8399061660723,-22.0617315730203));
#48846=CARTESIAN_POINT('Origin',(-6.70710678118655,-29.8399061660723,-22.0617315730203));
#48847=CARTESIAN_POINT('Origin',(-14.,-26.1629509039023,-17.6776695296637));
#48848=CARTESIAN_POINT('',(-14.,-34.2946788875476,-25.809397513309));
#48849=CARTESIAN_POINT('',(-14.,-12.2027957955108,-3.7175144212722));
#48850=CARTESIAN_POINT('',(-10.5,-34.2946788875476,-25.809397513309));
#48851=CARTESIAN_POINT('',(-14.,-34.2946788875476,-25.809397513309));
#48852=CARTESIAN_POINT('',(-10.5,-30.1934595566656,-21.708178182427));
#48853=CARTESIAN_POINT('',(-10.5,-29.3449314192417,-20.8596500450031));
#48854=CARTESIAN_POINT('',(-14.,-30.1934595566656,-21.708178182427));
#48855=CARTESIAN_POINT('Origin',(-14.,-29.8399061660723,-22.0617315730203));
#48856=CARTESIAN_POINT('Origin',(-10.5,-29.8399061660723,-22.0617315730203));
#48857=CARTESIAN_POINT('Origin',(-76.5,27.2236110756821,-27.2236110756821));
#48858=CARTESIAN_POINT('',(-76.5,27.2236110756821,-25.9736110756821));
#48859=CARTESIAN_POINT('Origin',(-76.5,27.2236110756821,-25.4736110756821));
#48860=CARTESIAN_POINT('Origin',(-76.5,27.2236110756821,-27.2236110756821));
#48861=CARTESIAN_POINT('Origin',(-83.,27.2236110756821,-27.2236110756821));
#48862=CARTESIAN_POINT('',(-67.5,27.2236110756821,-25.9736110756821));
#48863=CARTESIAN_POINT('',(-83.,27.2236110756821,-25.9736110756821));
#48864=CARTESIAN_POINT('',(-67.5,27.2236110756821,-28.4736110756821));
#48865=CARTESIAN_POINT('Origin',(-67.5,27.2236110756821,-27.2236110756821));
#48866=CARTESIAN_POINT('Origin',(-67.5,27.2236110756821,-27.2236110756821));
#48867=CARTESIAN_POINT('Origin',(-76.5,-27.2236110756821,27.2236110756821));
#48868=CARTESIAN_POINT('',(-76.5,-27.2236110756821,28.4736110756821));
#48869=CARTESIAN_POINT('Origin',(-76.5,-27.2236110756821,28.9736110756821));
#48870=CARTESIAN_POINT('Origin',(-76.5,-27.2236110756821,27.2236110756821));
#48871=CARTESIAN_POINT('Origin',(-83.,-27.2236110756821,27.2236110756821));
#48872=CARTESIAN_POINT('',(-67.5,-27.2236110756821,28.4736110756821));
#48873=CARTESIAN_POINT('',(-83.,-27.2236110756821,28.4736110756821));
#48874=CARTESIAN_POINT('',(-67.5,-27.2236110756821,25.9736110756821));
#48875=CARTESIAN_POINT('Origin',(-67.5,-27.2236110756821,27.2236110756821));
#48876=CARTESIAN_POINT('Origin',(-67.5,-27.2236110756821,27.2236110756821));
#48877=CARTESIAN_POINT('Origin',(-67.5,-12.5,21.650635094611));
#48878=CARTESIAN_POINT('',(-67.,-12.5,18.150635094611));
#48879=CARTESIAN_POINT('Origin',(-67.,-12.5,21.650635094611));
#48880=CARTESIAN_POINT('',(-67.5,-12.5,18.650635094611));
#48881=CARTESIAN_POINT('Origin',(-67.5,-12.5,18.150635094611));
#48882=CARTESIAN_POINT('',(-67.5,-12.5,24.650635094611));
#48883=CARTESIAN_POINT('Origin',(-67.5,-12.5,21.650635094611));
#48884=CARTESIAN_POINT('Origin',(-67.5,-12.5,21.650635094611));
#48885=CARTESIAN_POINT('Origin',(-67.,7.05,0.));
#48886=CARTESIAN_POINT('',(-67.,-5.26511090665038E-15,42.9928932188134));
#48887=CARTESIAN_POINT('Origin',(-67.,0.,0.));
#48888=CARTESIAN_POINT('',(-67.,-12.5,-25.150635094611));
#48889=CARTESIAN_POINT('Origin',(-67.,-12.5,-21.650635094611));
#48890=CARTESIAN_POINT('',(-67.,27.2236110756821,25.4736110756821));
#48891=CARTESIAN_POINT('Origin',(-67.,27.2236110756821,27.2236110756821));
#48892=CARTESIAN_POINT('',(-67.,25.,-3.5));
#48893=CARTESIAN_POINT('Origin',(-67.,25.,0.));
#48894=CARTESIAN_POINT('',(-67.,27.2236110756821,-28.9736110756821));
#48895=CARTESIAN_POINT('Origin',(-67.,27.2236110756821,-27.2236110756821));
#48896=CARTESIAN_POINT('',(-67.,12.,-16.2846096908265));
#48897=CARTESIAN_POINT('Origin',(-67.,12.,-20.7846096908265));
#48898=CARTESIAN_POINT('',(-67.,-24.,4.5));
#48899=CARTESIAN_POINT('Origin',(-67.,-24.,2.93915231795365E-15));
#48900=CARTESIAN_POINT('',(-67.,12.,25.2846096908265));
#48901=CARTESIAN_POINT('Origin',(-67.,12.,20.7846096908265));
#48902=CARTESIAN_POINT('',(-67.,-9.24608333356252E-16,7.55));
#48903=CARTESIAN_POINT('Origin',(-67.,0.,0.));
#48904=CARTESIAN_POINT('',(-67.,-27.2236110756821,25.4736110756821));
#48905=CARTESIAN_POINT('Origin',(-67.,-27.2236110756821,27.2236110756821));
#48906=CARTESIAN_POINT('',(-67.,-27.2236110756821,-28.9736110756821));
#48907=CARTESIAN_POINT('Origin',(-67.,-27.2236110756821,-27.2236110756821));
#48908=CARTESIAN_POINT('Origin',(-80.,-12.5,21.650635094611));
#48909=CARTESIAN_POINT('',(-80.,-12.5,24.650635094611));
#48910=CARTESIAN_POINT('Origin',(-80.,-12.5,21.650635094611));
#48911=CARTESIAN_POINT('',(-80.,-12.5,24.650635094611));
#48912=CARTESIAN_POINT('Origin',(-67.5,-12.5,-21.650635094611));
#48913=CARTESIAN_POINT('',(-67.5,-12.5,-24.650635094611));
#48914=CARTESIAN_POINT('Origin',(-67.5,-12.5,-25.150635094611));
#48915=CARTESIAN_POINT('',(-67.5,-12.5,-18.650635094611));
#48916=CARTESIAN_POINT('Origin',(-67.5,-12.5,-21.650635094611));
#48917=CARTESIAN_POINT('Origin',(-67.5,-12.5,-21.650635094611));
#48918=CARTESIAN_POINT('Origin',(-80.,-12.5,-21.650635094611));
#48919=CARTESIAN_POINT('',(-80.,-12.5,-18.650635094611));
#48920=CARTESIAN_POINT('Origin',(-80.,-12.5,-21.650635094611));
#48921=CARTESIAN_POINT('',(-80.,-12.5,-18.650635094611));
#48922=CARTESIAN_POINT('Origin',(-67.5,0.,0.));
#48923=CARTESIAN_POINT('Origin',(-67.5,-5.26511090665038E-15,42.9928932188134));
#48924=CARTESIAN_POINT('Origin',(-67.5,27.2236110756821,27.2236110756821));
#48925=CARTESIAN_POINT('Origin',(-67.5,27.2236110756821,25.4736110756821));
#48926=CARTESIAN_POINT('Origin',(-67.5,-27.2236110756821,-27.2236110756821));
#48927=CARTESIAN_POINT('Origin',(-67.5,-27.2236110756821,-28.9736110756821));
#48928=CARTESIAN_POINT('Origin',(-67.5,25.,0.));
#48929=CARTESIAN_POINT('',(-67.5,25.,-3.));
#48930=CARTESIAN_POINT('Origin',(-67.5,25.,-3.5));
#48931=CARTESIAN_POINT('',(-67.5,25.,3.));
#48932=CARTESIAN_POINT('Origin',(-67.5,25.,0.));
#48933=CARTESIAN_POINT('Origin',(-67.5,25.,0.));
#48934=CARTESIAN_POINT('Origin',(-80.,25.,0.));
#48935=CARTESIAN_POINT('',(-80.,25.,3.));
#48936=CARTESIAN_POINT('Origin',(-80.,25.,0.));
#48937=CARTESIAN_POINT('',(-80.,25.,3.));
#48938=CARTESIAN_POINT('Origin',(-67.5,-27.2236110756821,27.2236110756821));
#48939=CARTESIAN_POINT('Origin',(-67.5,-27.2236110756821,25.4736110756821));
#48940=CARTESIAN_POINT('Origin',(-67.5,27.2236110756821,-27.2236110756821));
#48941=CARTESIAN_POINT('Origin',(-67.5,27.2236110756821,-28.9736110756821));
#48942=CARTESIAN_POINT('Origin',(-16.,25.,0.));
#48943=CARTESIAN_POINT('',(-16.,25.,3.));
#48944=CARTESIAN_POINT('Origin',(-16.,25.,0.));
#48945=CARTESIAN_POINT('',(-15.5,25.,3.5));
#48946=CARTESIAN_POINT('Origin',(-16.,25.,3.5));
#48947=CARTESIAN_POINT('Origin',(-15.5,25.,0.));
#48948=CARTESIAN_POINT('Origin',(-80.,25.,0.));
#48949=CARTESIAN_POINT('',(-19.5,25.,3.));
#48950=CARTESIAN_POINT('Origin',(-19.5,25.,0.));
#48951=CARTESIAN_POINT('',(-80.,25.,3.));
#48952=CARTESIAN_POINT('Origin',(-15.5,25.,0.));
#48953=CARTESIAN_POINT('',(-15.5,25.,5.));
#48954=CARTESIAN_POINT('Origin',(-15.5,25.,0.));
#48955=CARTESIAN_POINT('Origin',(-16.,-12.5,21.650635094611));
#48956=CARTESIAN_POINT('',(-16.,-12.5,24.650635094611));
#48957=CARTESIAN_POINT('Origin',(-16.,-12.5,21.650635094611));
#48958=CARTESIAN_POINT('',(-15.5,-12.5,25.150635094611));
#48959=CARTESIAN_POINT('Origin',(-16.,-12.5,25.150635094611));
#48960=CARTESIAN_POINT('Origin',(-15.5,-12.5,21.650635094611));
#48961=CARTESIAN_POINT('Origin',(-80.,-12.5,21.650635094611));
#48962=CARTESIAN_POINT('',(-19.5,-12.5,24.650635094611));
#48963=CARTESIAN_POINT('Origin',(-19.5,-12.5,21.650635094611));
#48964=CARTESIAN_POINT('',(-80.,-12.5,24.650635094611));
#48965=CARTESIAN_POINT('Origin',(-15.5,-12.5,21.650635094611));
#48966=CARTESIAN_POINT('',(-15.5,-12.5,26.650635094611));
#48967=CARTESIAN_POINT('Origin',(-15.5,-12.5,21.650635094611));
#48968=CARTESIAN_POINT('Origin',(-16.,-12.5,-21.650635094611));
#48969=CARTESIAN_POINT('',(-16.,-12.5,-18.650635094611));
#48970=CARTESIAN_POINT('Origin',(-16.,-12.5,-21.650635094611));
#48971=CARTESIAN_POINT('',(-15.5,-12.5,-18.150635094611));
#48972=CARTESIAN_POINT('Origin',(-16.,-12.5,-18.150635094611));
#48973=CARTESIAN_POINT('Origin',(-15.5,-12.5,-21.650635094611));
#48974=CARTESIAN_POINT('Origin',(-80.,-12.5,-21.650635094611));
#48975=CARTESIAN_POINT('',(-19.5,-12.5,-18.650635094611));
#48976=CARTESIAN_POINT('Origin',(-19.5,-12.5,-21.650635094611));
#48977=CARTESIAN_POINT('',(-80.,-12.5,-18.650635094611));
#48978=CARTESIAN_POINT('Origin',(-15.5,-12.5,-21.650635094611));
#48979=CARTESIAN_POINT('',(-15.5,-12.5,-16.650635094611));
#48980=CARTESIAN_POINT('Origin',(-15.5,-12.5,-21.650635094611));
#48981=CARTESIAN_POINT('Origin',(-10.5,-32.1733585439879,-27.9307178568686));
#48982=CARTESIAN_POINT('',(-10.,-33.9411254969543,-26.1629509039023));
#48983=CARTESIAN_POINT('',(-10.,-32.1733585439879,-27.9307178568686));
#48984=CARTESIAN_POINT('',(-10.5,-34.2946788875476,-26.5165042944955));
#48985=CARTESIAN_POINT('Origin',(-10.5,-33.9411254969543,-26.1629509039023));
#48986=CARTESIAN_POINT('',(-10.5,-32.5269119345812,-28.2842712474619));
#48987=CARTESIAN_POINT('Origin',(-10.5,-28.9913780286485,-21.2132034355964));
#48988=CARTESIAN_POINT('Origin',(-10.5,-33.9411254969543,-26.1629509039023));
#48989=CARTESIAN_POINT('',(-10.,-28.9913780286485,-21.2132034355964));
#48990=CARTESIAN_POINT('Origin',(-10.5,-33.9411254969543,-26.1629509039023));
#48991=CARTESIAN_POINT('Origin',(-10.5,-33.9411254969543,-26.1629509039023));
#48992=CARTESIAN_POINT('Origin',(-14.,-34.6482322781408,-26.1629509039023));
#48993=CARTESIAN_POINT('',(-14.,-26.2486696528563,-34.5625135291868));
#48994=CARTESIAN_POINT('',(-14.,-29.5269119345812,-31.2842712474619));
#48995=CARTESIAN_POINT('',(-14.025428935758,-34.2946788875476,-26.5165042944955));
#48996=CARTESIAN_POINT('',(-14.,-34.2946788875476,-26.5165042944955));
#48997=CARTESIAN_POINT('',(-14.,-33.2888210834328,-27.5223620986103));
#48998=CARTESIAN_POINT('Ctrl Pts',(-14.025428935758,-34.2946788875476,-26.5165042944955));
#48999=CARTESIAN_POINT('Ctrl Pts',(-14.0048893955981,-33.9495862335655,
-26.8615969484776));
#49000=CARTESIAN_POINT('Ctrl Pts',(-14.,-33.6061320240591,-27.205051157984));
#49001=CARTESIAN_POINT('Ctrl Pts',(-14.,-33.2888210834328,-27.5223620986103));
#49002=CARTESIAN_POINT('',(-14.,-27.5223620986103,-33.2888210834328));
#49003=CARTESIAN_POINT('',(-14.,-29.5269119345812,-31.2842712474619));
#49004=CARTESIAN_POINT('',(-14.1464466094067,-25.5428242561643,-35.2683589258788));
#49005=CARTESIAN_POINT('Ctrl Pts',(-14.,-27.5223620986103,-33.2888210834328));
#49006=CARTESIAN_POINT('Ctrl Pts',(-14.,-27.1477600534413,-33.6634231286018));
#49007=CARTESIAN_POINT('Ctrl Pts',(-14.006470104281,-26.7367117564975,-34.0744714255456));
#49008=CARTESIAN_POINT('Ctrl Pts',(-14.0541139337517,-26.1259981746158,
-34.6851850074273));
#49009=CARTESIAN_POINT('Ctrl Pts',(-14.0762586162872,-25.9236817936235,
-34.8875013884196));
#49010=CARTESIAN_POINT('Ctrl Pts',(-14.1209183378663,-25.6651436792899,
-35.1460395027532));
#49011=CARTESIAN_POINT('Ctrl Pts',(-14.1328725146262,-25.6036027751564,
-35.2075804068867));
#49012=CARTESIAN_POINT('Ctrl Pts',(-14.1464466094065,-25.5428242561655,
-35.2683589258776));
#49013=CARTESIAN_POINT('Ctrl Pts',(-14.1464466094067,-25.5428242561643,
-35.2683589258788));
#49014=CARTESIAN_POINT('Ctrl Pts',(-14.0674931369572,-25.8963413932067,
-34.9148417888364));
#49015=CARTESIAN_POINT('Ctrl Pts',(-14.,-26.2486696528563,-34.5625135291868));
#49016=CARTESIAN_POINT('Origin',(-14.,-33.9411254969543,-26.1629509039023));
#49017=CARTESIAN_POINT('',(-14.,-34.4335120598975,-26.0760286821578));
#49018=CARTESIAN_POINT('Origin',(-14.,-33.9411254969543,-26.1629509039023));
#49019=CARTESIAN_POINT('Ctrl Pts',(-14.0254289357581,-34.2946788875476,
-26.5165042944955));
#49020=CARTESIAN_POINT('Ctrl Pts',(-14.0263293530702,-34.3098071424901,
-26.501376039553));
#49021=CARTESIAN_POINT('Ctrl Pts',(-14.0268044276371,-34.3239877839475,
-26.4852549680463));
#49022=CARTESIAN_POINT('Ctrl Pts',(-14.0268044276371,-34.3371305955528,
-26.4682048340719));
#49023=CARTESIAN_POINT('Ctrl Pts',(-14.0268044276371,-34.3619967163995,
-26.4359460827031));
#49024=CARTESIAN_POINT('Ctrl Pts',(-14.0250516964297,-34.3827322393151,
-26.4009212026149));
#49025=CARTESIAN_POINT('Ctrl Pts',(-14.0179720411043,-34.4215374836554,
-26.3124348467826));
#49026=CARTESIAN_POINT('Ctrl Pts',(-14.0115803121848,-34.4352140696344,
-26.2577402477615));
#49027=CARTESIAN_POINT('Ctrl Pts',(-14.0028573458318,-34.4429028780862,
-26.1599875313315));
#49028=CARTESIAN_POINT('Ctrl Pts',(-14.,-34.4408500788191,-26.1175962104965));
#49029=CARTESIAN_POINT('Ctrl Pts',(-14.,-34.4335120598975,-26.0760286821578));
#49030=CARTESIAN_POINT('Origin',(-19.1928932188134,0.,0.));
#49031=CARTESIAN_POINT('',(-19.1928932188134,-5.38844591624836E-15,44.));
#49032=CARTESIAN_POINT('',(-19.1928932188134,-44.,-5.38844591624836E-15));
#49033=CARTESIAN_POINT('Origin',(-19.1928932188134,0.,0.));
#49034=CARTESIAN_POINT('Origin',(-19.1928932188134,0.,0.));
#49035=CARTESIAN_POINT('',(-19.5464466094067,-5.37051137910276E-15,43.8535533905933));
#49036=CARTESIAN_POINT('Origin',(-19.1928932188134,-5.32721357629099E-15,
43.5));
#49037=CARTESIAN_POINT('',(-19.5464466094067,-43.8535533905933,-5.37051137910276E-15));
#49038=CARTESIAN_POINT('Origin',(-19.5464466094067,0.,-6.71313922387845E-15));
#49039=CARTESIAN_POINT('Origin',(-19.5464466094067,0.,-6.71313922387845E-15));
#49040=CARTESIAN_POINT('Origin',(-19.7,0.,0.));
#49041=CARTESIAN_POINT('',(-19.8535533905933,-43.5464466094067,-5.33290164544511E-15));
#49042=CARTESIAN_POINT('',(-19.7,-43.7,-5.35170651227393E-15));
#49043=CARTESIAN_POINT('',(-19.8535533905933,-5.3329016454451E-15,43.5464466094067));
#49044=CARTESIAN_POINT('Origin',(-19.8535533905933,0.,-6.66612705680638E-15));
#49045=CARTESIAN_POINT('Origin',(-19.8535533905933,0.,-6.66612705680638E-15));
#49046=CARTESIAN_POINT('Origin',(-17.,0.,0.));
#49047=CARTESIAN_POINT('',(-14.8071067811865,-44.,-5.38844591624836E-15));
#49048=CARTESIAN_POINT('',(-14.8071067811865,-5.38844591624836E-15,44.));
#49049=CARTESIAN_POINT('Origin',(-14.8071067811865,0.,0.));
#49050=CARTESIAN_POINT('',(-17.,-44.,-5.38844591624836E-15));
#49051=CARTESIAN_POINT('Origin',(-14.8071067811865,0.,0.));
#49052=CARTESIAN_POINT('Origin',(-19.5,0.,0.));
#49053=CARTESIAN_POINT('',(-20.,-5.28960384263333E-15,43.1928932188135));
#49054=CARTESIAN_POINT('Origin',(-19.5,-5.28960384263333E-15,43.1928932188135));
#49055=CARTESIAN_POINT('Origin',(-20.,0.,0.));
#49056=CARTESIAN_POINT('Origin',(-20.,43.4,0.));
#49057=CARTESIAN_POINT('',(-20.,-12.5,-18.150635094611));
#49058=CARTESIAN_POINT('Origin',(-20.,-12.5,-21.650635094611));
#49059=CARTESIAN_POINT('',(-20.,25.,3.5));
#49060=CARTESIAN_POINT('Origin',(-20.,25.,0.));
#49061=CARTESIAN_POINT('',(-20.,12.,-16.2846096908265));
#49062=CARTESIAN_POINT('Origin',(-20.,12.,-20.7846096908265));
#49063=CARTESIAN_POINT('',(-20.,-24.,4.5));
#49064=CARTESIAN_POINT('Origin',(-20.,-24.,2.93915231795365E-15));
#49065=CARTESIAN_POINT('',(-20.,12.,25.2846096908265));
#49066=CARTESIAN_POINT('Origin',(-20.,12.,20.7846096908265));
#49067=CARTESIAN_POINT('',(-20.,-1.53080849893419E-15,12.5));
#49068=CARTESIAN_POINT('Origin',(-20.,0.,0.));
#49069=CARTESIAN_POINT('',(-20.,-12.5,25.150635094611));
#49070=CARTESIAN_POINT('Origin',(-20.,-12.5,21.650635094611));
#49071=CARTESIAN_POINT('Origin',(-19.5,-12.5,-21.650635094611));
#49072=CARTESIAN_POINT('Origin',(-19.5,-12.5,-18.150635094611));
#49073=CARTESIAN_POINT('Origin',(-19.5,-12.5,21.650635094611));
#49074=CARTESIAN_POINT('Origin',(-19.5,-12.5,25.150635094611));
#49075=CARTESIAN_POINT('Origin',(-19.5,25.,0.));
#49076=CARTESIAN_POINT('Origin',(-19.5,25.,3.5));
#49077=CARTESIAN_POINT('Origin',(-67.5,0.,0.));
#49078=CARTESIAN_POINT('',(-67.5,-8.63375993398884E-16,7.05));
#49079=CARTESIAN_POINT('',(-67.5,-7.05,-8.63375993398884E-16));
#49080=CARTESIAN_POINT('Origin',(-67.5,0.,0.));
#49081=CARTESIAN_POINT('Origin',(-67.5,0.,0.));
#49082=CARTESIAN_POINT('Origin',(-67.5,-9.24608333356252E-16,7.55));
#49083=CARTESIAN_POINT('Origin',(-75.,0.,0.));
#49084=CARTESIAN_POINT('',(-82.2928932188135,-7.05,-8.63375993398884E-16));
#49085=CARTESIAN_POINT('',(-75.,-7.05,-8.63375993398884E-16));
#49086=CARTESIAN_POINT('',(-82.2928932188135,-8.63375993398884E-16,7.05));
#49087=CARTESIAN_POINT('Origin',(-82.2928932188135,0.,0.));
#49088=CARTESIAN_POINT('Origin',(-82.2928932188135,0.,0.));
#49089=CARTESIAN_POINT('Origin',(-82.5,0.,0.));
#49090=CARTESIAN_POINT('',(-82.8535533905933,7.40355339059327,0.));
#49091=CARTESIAN_POINT('',(-82.8535533905933,-9.06673796210658E-16,-7.40355339059327));
#49092=CARTESIAN_POINT('Origin',(-82.8535533905933,0.,-4.53336898105329E-16));
#49093=CARTESIAN_POINT('Origin',(-82.5,-9.49971599022433E-16,-7.75710678118654));
#49094=CARTESIAN_POINT('Origin',(-82.8535533905933,0.,-4.53336898105329E-16));
#49095=CARTESIAN_POINT('Origin',(-82.75,0.,0.));
#49096=CARTESIAN_POINT('',(-82.6464466094067,7.19644660940673,-1.76262106108895E-15));
#49097=CARTESIAN_POINT('',(-82.75,7.3,-8.93992163377568E-16));
#49098=CARTESIAN_POINT('',(-82.6464466094068,-8.81310530544477E-16,7.19644660940673));
#49099=CARTESIAN_POINT('Origin',(-82.6464466094067,0.,-4.40655265272239E-16));
#49100=CARTESIAN_POINT('Origin',(-82.6464466094067,0.,-4.40655265272239E-16));
#49101=CARTESIAN_POINT('Origin',(-82.2928932188135,0.,0.));
#49102=CARTESIAN_POINT('Origin',(-82.2928932188135,-9.24608333356252E-16,
7.55));
#49103=CARTESIAN_POINT('Origin',(-19.5,0.,0.));
#49104=CARTESIAN_POINT('',(-19.5,-1.46957615897682E-15,12.));
#49105=CARTESIAN_POINT('Origin',(-19.5,-1.53080849893419E-15,12.5));
#49106=CARTESIAN_POINT('',(-19.5,-12.,-1.46957615897682E-15));
#49107=CARTESIAN_POINT('Origin',(-19.5,0.,0.));
#49108=CARTESIAN_POINT('Origin',(-19.5,0.,0.));
#49109=CARTESIAN_POINT('Origin',(-17.,0.,0.));
#49110=CARTESIAN_POINT('',(-14.7071067811865,-12.,-1.46957615897682E-15));
#49111=CARTESIAN_POINT('',(-14.7071067811865,-1.46957615897682E-15,-12.));
#49112=CARTESIAN_POINT('Origin',(-14.7071067811865,0.,0.));
#49113=CARTESIAN_POINT('',(-17.,-12.,-1.46957615897682E-15));
#49114=CARTESIAN_POINT('Origin',(-14.7071067811865,0.,0.));
#49115=CARTESIAN_POINT('Origin',(-14.8071067811865,0.,0.));
#49116=CARTESIAN_POINT('',(-14.4535533905933,-5.37051137910276E-15,43.8535533905933));
#49117=CARTESIAN_POINT('',(-14.4535533905933,-43.8535533905933,-5.37051137910276E-15));
#49118=CARTESIAN_POINT('Origin',(-14.4535533905933,0.,-6.71313922387845E-15));
#49119=CARTESIAN_POINT('Origin',(-14.4535533905933,0.,-6.71313922387845E-15));
#49120=CARTESIAN_POINT('Origin',(-14.8071067811865,-5.32721357629099E-15,
43.5));
#49121=CARTESIAN_POINT('Origin',(-14.3,0.,0.));
#49122=CARTESIAN_POINT('',(-14.1464466094067,-43.5464466094067,-5.33290164544511E-15));
#49123=CARTESIAN_POINT('Origin',(-14.1464466094067,0.,4.44089209850063E-15));
#49124=CARTESIAN_POINT('',(-14.3,-43.7,-5.35170651227393E-15));
#49125=CARTESIAN_POINT('',(-14.1464466094067,25.5428242561642,-35.2683589258789));
#49126=CARTESIAN_POINT('Origin',(-14.1464466094067,0.,4.44089209850063E-15));
#49127=CARTESIAN_POINT('',(-14.,26.2486696528562,-34.5625135291869));
#49128=CARTESIAN_POINT('Ctrl Pts',(-14.,26.2486696528562,-34.5625135291869));
#49129=CARTESIAN_POINT('Ctrl Pts',(-14.0674931369565,25.8963413932104,-34.9148417888327));
#49130=CARTESIAN_POINT('Ctrl Pts',(-14.1464466094067,25.5428242561642,-35.2683589258789));
#49131=CARTESIAN_POINT('Origin',(-14.,0.,0.));
#49132=CARTESIAN_POINT('Origin',(-14.5,0.,0.));
#49133=CARTESIAN_POINT('Origin',(-14.,0.,0.));
#49134=CARTESIAN_POINT('Origin',(-14.,0.,0.));
#49135=CARTESIAN_POINT('Origin',(-14.,0.,0.));
#49136=CARTESIAN_POINT('Origin',(-14.,0.,0.));
#49137=CARTESIAN_POINT('Origin',(-14.,0.,0.));
#49138=CARTESIAN_POINT('',(-14.,33.2888210834329,-27.5223620986102));
#49139=CARTESIAN_POINT('Ctrl Pts',(-14.,33.2888210834329,-27.5223620986102));
#49140=CARTESIAN_POINT('Ctrl Pts',(-14.,33.6061320240592,-27.2050511579839));
#49141=CARTESIAN_POINT('Ctrl Pts',(-14.0048893955981,33.9495862335655,-26.8615969484775));
#49142=CARTESIAN_POINT('Ctrl Pts',(-14.025428935758,34.2946788875476,-26.5165042944955));
#49143=CARTESIAN_POINT('',(-14.,27.5223620986102,-33.2888210834329));
#49144=CARTESIAN_POINT('Origin',(-14.,0.,0.));
#49145=CARTESIAN_POINT('Ctrl Pts',(-14.1464466094073,25.5428242561618,-35.2683589258813));
#49146=CARTESIAN_POINT('Ctrl Pts',(-14.1328725146267,25.6036027751539,-35.2075804068892));
#49147=CARTESIAN_POINT('Ctrl Pts',(-14.1209183378665,25.6651436792886,-35.1460395027545));
#49148=CARTESIAN_POINT('Ctrl Pts',(-14.0762586162872,25.9236817936235,-34.8875013884196));
#49149=CARTESIAN_POINT('Ctrl Pts',(-14.0541139337517,26.1259981746158,-34.6851850074273));
#49150=CARTESIAN_POINT('Ctrl Pts',(-14.006470104281,26.7367117564975,-34.0744714255456));
#49151=CARTESIAN_POINT('Ctrl Pts',(-14.,27.1477600534412,-33.6634231286019));
#49152=CARTESIAN_POINT('Ctrl Pts',(-14.,27.5223620986102,-33.2888210834329));
#49153=CARTESIAN_POINT('Origin',(-14.,0.,0.));
#49154=CARTESIAN_POINT('Origin',(-14.5,-12.5,-21.650635094611));
#49155=CARTESIAN_POINT('',(-14.,-12.5,-27.150635094611));
#49156=CARTESIAN_POINT('Origin',(-14.,-12.5,-21.650635094611));
#49157=CARTESIAN_POINT('',(-14.5,-12.5,-26.650635094611));
#49158=CARTESIAN_POINT('Origin',(-14.5,-12.5,-27.150635094611));
#49159=CARTESIAN_POINT('',(-14.5,-12.5,-16.650635094611));
#49160=CARTESIAN_POINT('Origin',(-14.5,-12.5,-21.650635094611));
#49161=CARTESIAN_POINT('Origin',(-14.5,-12.5,-21.650635094611));
#49162=CARTESIAN_POINT('Origin',(-14.,12.,0.));
#49163=CARTESIAN_POINT('',(-14.,31.2842712474619,-29.5269119345812));
#49164=CARTESIAN_POINT('',(-14.,-21.0416305603426,22.7989898732233));
#49165=CARTESIAN_POINT('',(-14.,-12.5,16.150635094611));
#49166=CARTESIAN_POINT('Origin',(-14.,-12.5,21.650635094611));
#49167=CARTESIAN_POINT('',(-14.,-1.55617176460037E-15,12.7071067811865));
#49168=CARTESIAN_POINT('Origin',(-14.,0.,0.));
#49169=CARTESIAN_POINT('',(-14.,25.,-5.5));
#49170=CARTESIAN_POINT('Origin',(-14.,25.,0.));
#49171=CARTESIAN_POINT('Origin',(-15.5,-12.5,-21.650635094611));
#49172=CARTESIAN_POINT('',(-15.5,-12.5,-16.650635094611));
#49173=CARTESIAN_POINT('Origin',(-14.5,-12.5,21.650635094611));
#49174=CARTESIAN_POINT('',(-14.5,-12.5,16.650635094611));
#49175=CARTESIAN_POINT('Origin',(-14.5,-12.5,16.150635094611));
#49176=CARTESIAN_POINT('',(-14.5,-12.5,26.650635094611));
#49177=CARTESIAN_POINT('Origin',(-14.5,-12.5,21.650635094611));
#49178=CARTESIAN_POINT('Origin',(-14.5,-12.5,21.650635094611));
#49179=CARTESIAN_POINT('Origin',(-15.5,-12.5,21.650635094611));
#49180=CARTESIAN_POINT('',(-15.5,-12.5,26.650635094611));
#49181=CARTESIAN_POINT('Origin',(-14.5,25.,0.));
#49182=CARTESIAN_POINT('',(-14.5,25.,-5.));
#49183=CARTESIAN_POINT('Origin',(-14.5,25.,-5.5));
#49184=CARTESIAN_POINT('',(-14.5,25.,5.));
#49185=CARTESIAN_POINT('Origin',(-14.5,25.,0.));
#49186=CARTESIAN_POINT('Origin',(-14.5,25.,0.));
#49187=CARTESIAN_POINT('Origin',(-15.5,25.,0.));
#49188=CARTESIAN_POINT('',(-15.5,25.,5.));
#49189=CARTESIAN_POINT('Origin',(-14.7071067811865,0.,0.));
#49190=CARTESIAN_POINT('',(-14.3535533905933,12.1464466094067,2.46519032881566E-31));
#49191=CARTESIAN_POINT('',(-14.3535533905933,-1.48751069612242E-15,-12.1464466094067));
#49192=CARTESIAN_POINT('Origin',(-14.3535533905933,0.,-7.43755348061208E-16));
#49193=CARTESIAN_POINT('Origin',(-14.7071067811865,-1.53080849893419E-15,
-12.5));
#49194=CARTESIAN_POINT('Origin',(-14.3535533905933,0.,-7.43755348061208E-16));
#49195=CARTESIAN_POINT('Origin',(-14.25,0.,0.));
#49196=CARTESIAN_POINT('',(-14.1464466094067,12.3535533905933,-3.0257479235772E-15));
#49197=CARTESIAN_POINT('',(-14.25,12.25,-1.50019232895551E-15));
#49198=CARTESIAN_POINT('',(-14.1464466094067,-1.5128739617886E-15,12.3535533905933));
#49199=CARTESIAN_POINT('Origin',(-14.1464466094067,0.,-7.56436980894299E-16));
#49200=CARTESIAN_POINT('Origin',(-14.1464466094067,0.,-7.56436980894299E-16));
#49201=CARTESIAN_POINT('Origin',(-14.5,0.,0.));
#49202=CARTESIAN_POINT('Origin',(-14.5,-1.55617176460037E-15,12.7071067811865));
#49203=CARTESIAN_POINT('Origin',(-83.,-29.9484575042249,-28.4786855519014));
#49204=CARTESIAN_POINT('',(-83.,-29.9484575042249,-28.4786855519014));
#49205=CARTESIAN_POINT('Origin',(-83.,-27.2236110756821,-27.2236110756821));
#49206=CARTESIAN_POINT('Origin',(-83.,-27.2236110756821,27.2236110756821));
#49207=CARTESIAN_POINT('Origin',(-83.,27.2236110756821,27.2236110756821));
#49208=CARTESIAN_POINT('Origin',(-80.,25.,0.));
#49209=CARTESIAN_POINT('Origin',(-80.,-12.5,21.650635094611));
#49210=CARTESIAN_POINT('Origin',(-80.,-12.5,-21.650635094611));
#49211=CARTESIAN_POINT('Origin',(-14.,26.1629509039022,-34.6482322781408));
#49212=CARTESIAN_POINT('',(-14.,31.2842712474619,-29.5269119345812));
#49213=CARTESIAN_POINT('Origin',(-14.,12.,0.));
#49214=CARTESIAN_POINT('Origin',(-14.,12.,0.));
#49215=CARTESIAN_POINT('Origin',(-14.,12.,0.));
#49216=CARTESIAN_POINT('Origin',(-10.,-28.2842712474619,-28.2842712474619));
#49217=CARTESIAN_POINT('Origin',(-14.,12.,0.));
#49218=CARTESIAN_POINT('Origin',(-14.,-26.1629509039023,17.6776695296637));
#49219=CARTESIAN_POINT('Origin',(-74.5,0.,0.));
#49220=CARTESIAN_POINT('',(-74.5,-42.4,-5.19250242838478E-15));
#49221=CARTESIAN_POINT('Origin',(-67.5,12.,-20.7846096908265));
#49222=CARTESIAN_POINT('',(-67.5,12.,-16.2846096908265));
#49223=CARTESIAN_POINT('Origin',(-67.5,-24.,2.93915231795365E-15));
#49224=CARTESIAN_POINT('',(-67.5,-24.,4.5));
#49225=CARTESIAN_POINT('Origin',(-67.5,12.,20.7846096908265));
#49226=CARTESIAN_POINT('',(-67.5,12.,25.2846096908265));
#49227=CARTESIAN_POINT('',(0.,0.,0.));
#49228=CARTESIAN_POINT('Origin',(-21.15,0.,0.));
#49229=CARTESIAN_POINT('',(-21.3,3.03,-3.71067980141648E-16));
#49230=CARTESIAN_POINT('',(-21.3,-3.03,-3.71067980141648E-16));
#49231=CARTESIAN_POINT('Origin',(-21.3,0.,0.));
#49232=CARTESIAN_POINT('Origin',(-21.3,0.,0.));
#49233=CARTESIAN_POINT('',(-21.,3.33,4.07807384116069E-16));
#49234=CARTESIAN_POINT('',(-21.15,3.18,-3.89437682128858E-16));
#49235=CARTESIAN_POINT('Origin',(-21.,0.,0.));
#49236=CARTESIAN_POINT('Origin',(-43.5,0.,0.));
#49237=CARTESIAN_POINT('',(-65.7,-3.03,-3.71067980141648E-16));
#49238=CARTESIAN_POINT('',(-43.5,-3.03,-3.71067980141648E-16));
#49239=CARTESIAN_POINT('',(-65.7,3.03,3.71067980141648E-16));
#49240=CARTESIAN_POINT('Origin',(-65.7,0.,0.));
#49241=CARTESIAN_POINT('Origin',(-65.7,0.,0.));
#49242=CARTESIAN_POINT('Origin',(-21.,3.03,0.));
#49243=CARTESIAN_POINT('',(-21.,8.83189477299562,-3.49966208636385));
#49244=CARTESIAN_POINT('',(-21.,6.8122671513043,-2.29198004120026));
#49245=CARTESIAN_POINT('Ctrl Pts',(-21.,8.83189477299562,-3.49966208636385));
#49246=CARTESIAN_POINT('Ctrl Pts',(-21.,8.82094392654054,-3.48448547507508));
#49247=CARTESIAN_POINT('Ctrl Pts',(-21.,8.7936907445869,-3.44793862615663));
#49248=CARTESIAN_POINT('Ctrl Pts',(-21.,8.74934377286772,-3.39315507789778));
#49249=CARTESIAN_POINT('Ctrl Pts',(-21.,8.68667704834295,-3.32467389681987));
#49250=CARTESIAN_POINT('Ctrl Pts',(-21.,8.60460841273967,-3.24456764186082));
#49251=CARTESIAN_POINT('Ctrl Pts',(-21.,8.51516539363766,-3.16038325236223));
#49252=CARTESIAN_POINT('Ctrl Pts',(-21.,8.4243384303954,-3.07426635319921));
#49253=CARTESIAN_POINT('Ctrl Pts',(-21.,8.33184183835821,-2.98721060740199));
#49254=CARTESIAN_POINT('Ctrl Pts',(-21.,8.2370828133169,-2.90227874531213));
#49255=CARTESIAN_POINT('Ctrl Pts',(-21.,8.13939365460193,-2.82329483425037));
#49256=CARTESIAN_POINT('Ctrl Pts',(-21.,8.03835937937461,-2.75296659957235));
#49257=CARTESIAN_POINT('Ctrl Pts',(-21.,7.93399262158453,-2.69188736687836));
#49258=CARTESIAN_POINT('Ctrl Pts',(-21.,7.82659266808561,-2.63932460382938));
#49259=CARTESIAN_POINT('Ctrl Pts',(-21.,7.71666617412861,-2.59365833862295));
#49260=CARTESIAN_POINT('Ctrl Pts',(-21.,7.60482241577417,-2.55297760756074));
#49261=CARTESIAN_POINT('Ctrl Pts',(-21.,7.49168859641892,-2.51552733857386));
#49262=CARTESIAN_POINT('Ctrl Pts',(-21.,7.37786505179862,-2.47974127678492));
#49263=CARTESIAN_POINT('Ctrl Pts',(-21.,7.26387759821705,-2.44432136933076));
#49264=CARTESIAN_POINT('Ctrl Pts',(-21.,7.15012820840451,-2.4083053284885));
#49265=CARTESIAN_POINT('Ctrl Pts',(-21.,7.03685278876406,-2.37112767623027));
#49266=CARTESIAN_POINT('Ctrl Pts',(-21.,6.94670492800217,-2.3402328805745));
#49267=CARTESIAN_POINT('Ctrl Pts',(-21.,6.8793763726903,-2.31637371632821));
#49268=CARTESIAN_POINT('Ctrl Pts',(-21.,6.83461600336474,-2.30016217089616));
#49269=CARTESIAN_POINT('Ctrl Pts',(-21.,6.8122671513043,-2.29198004120026));
#49270=CARTESIAN_POINT('',(-21.,7.13209349341826,-0.890729280500487));
#49271=CARTESIAN_POINT('Origin',(-21.,0.,0.));
#49272=CARTESIAN_POINT('',(-21.,9.47665840807863,-0.665541446186862));
#49273=CARTESIAN_POINT('Ctrl Pts',(-21.,7.13209349341826,-0.890729280500493));
#49274=CARTESIAN_POINT('Ctrl Pts',(-21.,7.15211036864424,-0.892482057440589));
#49275=CARTESIAN_POINT('Ctrl Pts',(-21.,7.19212249719958,-0.896150298874621));
#49276=CARTESIAN_POINT('Ctrl Pts',(-21.,7.25207582250743,-0.902140734147995));
#49277=CARTESIAN_POINT('Ctrl Pts',(-21.,7.33188369780814,-0.9111053356665));
#49278=CARTESIAN_POINT('Ctrl Pts',(-21.,7.43143474677318,-0.923884053007732));
#49279=CARTESIAN_POINT('Ctrl Pts',(-21.,7.53080214904746,-0.938052795086853));
#49280=CARTESIAN_POINT('Ctrl Pts',(-21.,7.63003710778607,-0.953237934402832));
#49281=CARTESIAN_POINT('Ctrl Pts',(-21.,7.7292275500742,-0.968799418422936));
#49282=CARTESIAN_POINT('Ctrl Pts',(-21.,7.82850348500033,-0.983785216334556));
#49283=CARTESIAN_POINT('Ctrl Pts',(-21.,7.92800888935854,-0.997080466154163));
#49284=CARTESIAN_POINT('Ctrl Pts',(-21.,8.02787639670185,-1.00753800115478));
#49285=CARTESIAN_POINT('Ctrl Pts',(-21.,8.12820273854248,-1.01410892133532));
#49286=CARTESIAN_POINT('Ctrl Pts',(-21.,8.2290192302709,-1.01599010763451));
#49287=CARTESIAN_POINT('Ctrl Pts',(-21.,8.33027821569813,-1.01271355471894));
#49288=CARTESIAN_POINT('Ctrl Pts',(-21.,8.43188165539955,-1.00407739851957));
#49289=CARTESIAN_POINT('Ctrl Pts',(-21.,8.53370212161309,-0.990109101007578));
#49290=CARTESIAN_POINT('Ctrl Pts',(-21.,8.63560512714608,-0.971017102543952));
#49291=CARTESIAN_POINT('Ctrl Pts',(-21.,8.73747423363077,-0.947150867813171));
#49292=CARTESIAN_POINT('Ctrl Pts',(-21.,8.83922276353739,-0.91895289219465));
#49293=CARTESIAN_POINT('Ctrl Pts',(-21.,8.94078425956014,-0.886903960171006));
#49294=CARTESIAN_POINT('Ctrl Pts',(-21.,9.04210805084257,-0.851468211346448));
#49295=CARTESIAN_POINT('Ctrl Pts',(-21.,9.14315312384119,-0.813043722977556));
#49296=CARTESIAN_POINT('Ctrl Pts',(-21.,9.24388219451327,-0.771898853704204));
#49297=CARTESIAN_POINT('Ctrl Pts',(-21.,9.33073157135268,-0.734052451290808));
#49298=CARTESIAN_POINT('Ctrl Pts',(-21.,9.39728977570677,-0.703536138917769));
#49299=CARTESIAN_POINT('Ctrl Pts',(-21.,9.44372410361834,-0.681495939481608));
#49300=CARTESIAN_POINT('Ctrl Pts',(-21.,9.47015861118831,-0.668702181892299));
#49301=CARTESIAN_POINT('Ctrl Pts',(-21.,9.47665840807863,-0.665541446186862));
#49302=CARTESIAN_POINT('',(-21.,9.47570870673866,0.678928939607903));
#49303=CARTESIAN_POINT('Origin',(-21.,0.,0.));
#49304=CARTESIAN_POINT('',(-21.,7.13209349341826,0.890729280500491));
#49305=CARTESIAN_POINT('Ctrl Pts',(-21.,9.47570870673866,0.678928939607903));
#49306=CARTESIAN_POINT('Ctrl Pts',(-21.,9.45925745015235,0.687851199692914));
#49307=CARTESIAN_POINT('Ctrl Pts',(-21.,9.41884609819914,0.708954060299467));
#49308=CARTESIAN_POINT('Ctrl Pts',(-21.,9.35512116653373,0.739070901845868));
#49309=CARTESIAN_POINT('Ctrl Pts',(-21.,9.26894752777823,0.773580241279191));
#49310=CARTESIAN_POINT('Ctrl Pts',(-21.,9.1602494406401,0.810145236641718));
#49311=CARTESIAN_POINT('Ctrl Pts',(-21.,9.04313782728701,0.847184879177382));
#49312=CARTESIAN_POINT('Ctrl Pts',(-21.,8.92394083882956,0.885365181899305));
#49313=CARTESIAN_POINT('Ctrl Pts',(-21.,8.80283221651881,0.923666931425907));
#49314=CARTESIAN_POINT('Ctrl Pts',(-21.,8.68060673111004,0.95907349496179));
#49315=CARTESIAN_POINT('Ctrl Pts',(-21.,8.55832200571467,0.987849802439111));
#49316=CARTESIAN_POINT('Ctrl Pts',(-21.,8.43677899171613,1.00737622330388));
#49317=CARTESIAN_POINT('Ctrl Pts',(-21.,8.31624650623966,1.017123671327));
#49318=CARTESIAN_POINT('Ctrl Pts',(-21.,8.19667636355292,1.01788199103989));
#49319=CARTESIAN_POINT('Ctrl Pts',(-21.,8.0778221648407,1.01133055607812));
#49320=CARTESIAN_POINT('Ctrl Pts',(-21.,7.95940371279084,0.999455440216893));
#49321=CARTESIAN_POINT('Ctrl Pts',(-21.,7.84122460090589,0.984110042106143));
#49322=CARTESIAN_POINT('Ctrl Pts',(-21.,7.72314614047142,0.966965984543333));
#49323=CARTESIAN_POINT('Ctrl Pts',(-21.,7.60507887157754,0.949420915891057));
#49324=CARTESIAN_POINT('Ctrl Pts',(-21.,7.4869674381447,0.932516236860827));
#49325=CARTESIAN_POINT('Ctrl Pts',(-21.,7.36877903277666,0.916863781503487));
#49326=CARTESIAN_POINT('Ctrl Pts',(-21.,7.27415386726379,0.90558533966873));
#49327=CARTESIAN_POINT('Ctrl Pts',(-21.,7.20314083161155,0.897868938540711));
#49328=CARTESIAN_POINT('Ctrl Pts',(-21.,7.15577920638447,0.893054239868309));
#49329=CARTESIAN_POINT('Ctrl Pts',(-21.,7.13209349341826,0.890729280500491));
#49330=CARTESIAN_POINT('',(-21.,6.8122671513043,2.29198004120026));
#49331=CARTESIAN_POINT('Origin',(-21.,0.,0.));
#49332=CARTESIAN_POINT('',(-21.,8.82694180863381,3.51213586112388));
#49333=CARTESIAN_POINT('Ctrl Pts',(-21.,6.8122671513043,2.29198004120026));
#49334=CARTESIAN_POINT('Ctrl Pts',(-21.,6.8310622341282,2.29908584041335));
#49335=CARTESIAN_POINT('Ctrl Pts',(-21.,6.86870350660446,2.31314148102898));
#49336=CARTESIAN_POINT('Ctrl Pts',(-21.,6.92531873868941,2.33375705829959));
#49337=CARTESIAN_POINT('Ctrl Pts',(-21.,7.00111274457534,2.36030757076476));
#49338=CARTESIAN_POINT('Ctrl Pts',(-21.,7.09634961812101,2.39198792562662));
#49339=CARTESIAN_POINT('Ctrl Pts',(-21.,7.19202414084635,2.42233623016115));
#49340=CARTESIAN_POINT('Ctrl Pts',(-21.,7.28802033430286,2.45171132733138));
#49341=CARTESIAN_POINT('Ctrl Pts',(-21.,7.3841397096708,2.4807280346756));
#49342=CARTESIAN_POINT('Ctrl Pts',(-21.,7.4800863304027,2.5103005111467));
#49343=CARTESIAN_POINT('Ctrl Pts',(-21.,7.57550619462173,2.54149568187359));
#49344=CARTESIAN_POINT('Ctrl Pts',(-21.,7.67002106404108,2.5754046559055));
#49345=CARTESIAN_POINT('Ctrl Pts',(-21.,7.76326299008741,2.61301442971916));
#49346=CARTESIAN_POINT('Ctrl Pts',(-21.,7.85491172665132,2.65506217582471));
#49347=CARTESIAN_POINT('Ctrl Pts',(-21.,7.94472127708621,2.70194887521209));
#49348=CARTESIAN_POINT('Ctrl Pts',(-21.,8.03251572538561,2.75381386341092));
#49349=CARTESIAN_POINT('Ctrl Pts',(-21.,8.11819217840571,2.81057710920625));
#49350=CARTESIAN_POINT('Ctrl Pts',(-21.,8.201719906256,2.87199246251599));
#49351=CARTESIAN_POINT('Ctrl Pts',(-21.,8.28314562863609,2.93769454582461));
#49352=CARTESIAN_POINT('Ctrl Pts',(-21.,8.36258324333989,3.00724707660037));
#49353=CARTESIAN_POINT('Ctrl Pts',(-21.,8.44018147897284,3.08018804824792));
#49354=CARTESIAN_POINT('Ctrl Pts',(-21.,8.51609606529771,3.15607730017284));
#49355=CARTESIAN_POINT('Ctrl Pts',(-21.,8.59046276963722,3.23453838205034));
#49356=CARTESIAN_POINT('Ctrl Pts',(-21.,8.66336443667969,3.31531333416059));
#49357=CARTESIAN_POINT('Ctrl Pts',(-21.,8.72519208281745,3.38709429686028));
#49358=CARTESIAN_POINT('Ctrl Pts',(-21.,8.77191842112748,3.44346706684567));
#49359=CARTESIAN_POINT('Ctrl Pts',(-21.,8.80419142083552,3.4834717001977));
#49360=CARTESIAN_POINT('Ctrl Pts',(-21.,8.82245708581418,3.50646798047534));
#49361=CARTESIAN_POINT('Ctrl Pts',(-21.,8.82694180863381,3.51213586112388));
#49362=CARTESIAN_POINT('',(-21.,8.24274231917123,4.72304976257329));
#49363=CARTESIAN_POINT('Origin',(-21.,0.,0.));
#49364=CARTESIAN_POINT('',(-21.,6.03932124977421,3.89701874412038));
#49365=CARTESIAN_POINT('Ctrl Pts',(-21.,8.24274231917123,4.72304976257329));
#49366=CARTESIAN_POINT('Ctrl Pts',(-21.,8.22404902558203,4.72395050842036));
#49367=CARTESIAN_POINT('Ctrl Pts',(-21.,8.17848346749629,4.7254297003623));
#49368=CARTESIAN_POINT('Ctrl Pts',(-21.,8.10800208013598,4.72491482536916));
#49369=CARTESIAN_POINT('Ctrl Pts',(-21.,8.0153892731556,4.71861732525386));
#49370=CARTESIAN_POINT('Ctrl Pts',(-21.,7.9015907237349,4.70439891524807));
#49371=CARTESIAN_POINT('Ctrl Pts',(-21.,7.78000590743498,4.68695765535521));
#49372=CARTESIAN_POINT('Ctrl Pts',(-21.,7.65604731918147,4.66963928443128));
#49373=CARTESIAN_POINT('Ctrl Pts',(-21.,7.53031371454558,4.65160090645339));
#49374=CARTESIAN_POINT('Ctrl Pts',(-21.,7.40483002515176,4.63046946729401));
#49375=CARTESIAN_POINT('Ctrl Pts',(-21.,7.28216972266428,4.60333867057275));
#49376=CARTESIAN_POINT('Ctrl Pts',(-21.,7.16419105444418,4.56819583049617));
#49377=CARTESIAN_POINT('Ctrl Pts',(-21.,7.05136577826386,4.52468089222283));
#49378=CARTESIAN_POINT('Ctrl Pts',(-21.,6.94330777957998,4.47348457408032));
#49379=CARTESIAN_POINT('Ctrl Pts',(-21.,6.83906640781858,4.4160130309926));
#49380=CARTESIAN_POINT('Ctrl Pts',(-21.,6.73752748880879,4.35393408054299));
#49381=CARTESIAN_POINT('Ctrl Pts',(-21.,6.63770990687462,4.2888323596294));
#49382=CARTESIAN_POINT('Ctrl Pts',(-21.,6.53876341785232,4.22215377357323));
#49383=CARTESIAN_POINT('Ctrl Pts',(-21.,6.44000100425059,4.15511874483725));
#49384=CARTESIAN_POINT('Ctrl Pts',(-21.,6.34092094513049,4.08864152493875));
#49385=CARTESIAN_POINT('Ctrl Pts',(-21.,6.24122821720367,4.02325912271413));
#49386=CARTESIAN_POINT('Ctrl Pts',(-21.,6.16086742147114,3.97204127711522));
#49387=CARTESIAN_POINT('Ctrl Pts',(-21.,6.10023490810719,3.93427763849175));
#49388=CARTESIAN_POINT('Ctrl Pts',(-21.,6.05965257770704,3.90939030583537));
#49389=CARTESIAN_POINT('Ctrl Pts',(-21.,6.03932124977421,3.89701874412038));
#49390=CARTESIAN_POINT('',(-21.,5.14318775290069,5.02073460645077));
#49391=CARTESIAN_POINT('Origin',(-21.,0.,0.));
#49392=CARTESIAN_POINT('',(-21.,6.42894112865204,6.99419158761942));
#49393=CARTESIAN_POINT('Ctrl Pts',(-21.,5.14318775290069,5.02073460645076));
#49394=CARTESIAN_POINT('Ctrl Pts',(-21.,5.15703844666268,5.03529159113598));
#49395=CARTESIAN_POINT('Ctrl Pts',(-21.,5.18485354740602,5.06428722179623));
#49396=CARTESIAN_POINT('Ctrl Pts',(-21.,5.22691734521339,5.10742564369892));
#49397=CARTESIAN_POINT('Ctrl Pts',(-21.,5.28368554926634,5.16423261553338));
#49398=CARTESIAN_POINT('Ctrl Pts',(-21.,5.35574541658332,5.23409735978387));
#49399=CARTESIAN_POINT('Ctrl Pts',(-21.,5.42877754716296,5.30295185702147));
#49400=CARTESIAN_POINT('Ctrl Pts',(-21.,5.50252175190725,5.37106909242141));
#49401=CARTESIAN_POINT('Ctrl Pts',(-21.,5.57653243923659,5.43891687637388));
#49402=CARTESIAN_POINT('Ctrl Pts',(-21.,5.65014634083023,5.50719043557996));
#49403=CARTESIAN_POINT('Ctrl Pts',(-21.,5.72258159055366,5.57669744070723));
#49404=CARTESIAN_POINT('Ctrl Pts',(-21.,5.79302399301176,5.64825683559838));
#49405=CARTESIAN_POINT('Ctrl Pts',(-21.,5.86071379627312,5.72259822644884));
#49406=CARTESIAN_POINT('Ctrl Pts',(-21.,5.92504262139805,5.80024683316115));
#49407=CARTESIAN_POINT('Ctrl Pts',(-21.,5.98561485393513,5.88145719317904));
#49408=CARTESIAN_POINT('Ctrl Pts',(-21.,6.04221154361855,5.96627851638222));
#49409=CARTESIAN_POINT('Ctrl Pts',(-21.,6.09477471117184,6.05459405347559));
#49410=CARTESIAN_POINT('Ctrl Pts',(-21.,6.14338347043832,6.14616869769857));
#49411=CARTESIAN_POINT('Ctrl Pts',(-21.,6.18823844577549,6.2406935262026));
#49412=CARTESIAN_POINT('Ctrl Pts',(-21.,6.22963155144596,6.33782488040965));
#49413=CARTESIAN_POINT('Ctrl Pts',(-21.,6.2678972444421,6.43721103768399));
#49414=CARTESIAN_POINT('Ctrl Pts',(-21.,6.30336681095649,6.53852299564495));
#49415=CARTESIAN_POINT('Ctrl Pts',(-21.,6.33632590879467,6.64148049150319));
#49416=CARTESIAN_POINT('Ctrl Pts',(-21.,6.36696110296949,6.74588705654512));
#49417=CARTESIAN_POINT('Ctrl Pts',(-21.,6.3915212948217,6.8373854795327));
#49418=CARTESIAN_POINT('Ctrl Pts',(-21.,6.40916104272443,6.90844938866819));
#49419=CARTESIAN_POINT('Ctrl Pts',(-21.,6.42088065083439,6.95849504767608));
#49420=CARTESIAN_POINT('Ctrl Pts',(-21.,6.42735973425904,6.98713915530221));
#49421=CARTESIAN_POINT('Ctrl Pts',(-21.,6.42894112865204,6.99419158761942));
#49422=CARTESIAN_POINT('',(-21.,5.37719972469147,7.83171265565699));
#49423=CARTESIAN_POINT('Origin',(-21.,0.,0.));
#49424=CARTESIAN_POINT('',(-21.,3.75038736519793,6.13145585166881));
#49425=CARTESIAN_POINT('Ctrl Pts',(-21.,5.37719972469147,7.83171265565699));
#49426=CARTESIAN_POINT('Ctrl Pts',(-21.,5.35996683015292,7.82441348350419));
#49427=CARTESIAN_POINT('Ctrl Pts',(-21.,5.31827188353843,7.80597603467631));
#49428=CARTESIAN_POINT('Ctrl Pts',(-21.,5.25499374364742,7.77493142045055));
#49429=CARTESIAN_POINT('Ctrl Pts',(-21.,5.17428487068616,7.72907437791822));
#49430=CARTESIAN_POINT('Ctrl Pts',(-21.,5.07792505734327,7.66688869302314));
#49431=CARTESIAN_POINT('Ctrl Pts',(-21.,4.97594840210465,7.59842098612655));
#49432=CARTESIAN_POINT('Ctrl Pts',(-21.,4.87177973271099,7.52903405731413));
#49433=CARTESIAN_POINT('Ctrl Pts',(-21.,4.76632422816958,7.45822827381644));
#49434=CARTESIAN_POINT('Ctrl Pts',(-21.,4.66243591843161,7.38474417264741));
#49435=CARTESIAN_POINT('Ctrl Pts',(-21.,4.56369441608956,7.30707985875561));
#49436=CARTESIAN_POINT('Ctrl Pts',(-21.,4.4726472158023,7.22422822821349));
#49437=CARTESIAN_POINT('Ctrl Pts',(-21.,4.38987557857684,7.13606957084443));
#49438=CARTESIAN_POINT('Ctrl Pts',(-21.,4.31473193577955,7.04305867353628));
#49439=CARTESIAN_POINT('Ctrl Pts',(-21.,4.24574967308284,6.94604996627335));
#49440=CARTESIAN_POINT('Ctrl Pts',(-21.,4.18120131531612,6.84606267872027));
#49441=CARTESIAN_POINT('Ctrl Pts',(-21.,4.11951535961712,6.74409882925098));
#49442=CARTESIAN_POINT('Ctrl Pts',(-21.,4.05929840765689,6.64109222642907));
#49443=CARTESIAN_POINT('Ctrl Pts',(-21.,3.99940195660266,6.53784434718121));
#49444=CARTESIAN_POINT('Ctrl Pts',(-21.,3.93897729264122,6.43496121510494));
#49445=CARTESIAN_POINT('Ctrl Pts',(-21.,3.87752560957259,6.33279865263617));
#49446=CARTESIAN_POINT('Ctrl Pts',(-21.,3.82734562477572,6.25178572573963));
#49447=CARTESIAN_POINT('Ctrl Pts',(-21.,3.78910264658076,6.19145440139071));
#49448=CARTESIAN_POINT('Ctrl Pts',(-21.,3.7633374392529,6.15142367620606));
#49449=CARTESIAN_POINT('Ctrl Pts',(-21.,3.75038736519793,6.13145585166881));
#49450=CARTESIAN_POINT('',(-21.,2.45543694297674,6.75507110762463));
#49451=CARTESIAN_POINT('Origin',(-21.,0.,0.));
#49452=CARTESIAN_POINT('',(-21.,2.75760981235205,9.09096189205629));
#49453=CARTESIAN_POINT('Ctrl Pts',(-21.,2.45543694297675,6.75507110762463));
#49454=CARTESIAN_POINT('Ctrl Pts',(-21.,2.46159994790965,6.77419608843537));
#49455=CARTESIAN_POINT('Ctrl Pts',(-21.,2.47407975508802,6.8123887688799));
#49456=CARTESIAN_POINT('Ctrl Pts',(-21.,2.49326086758344,6.8695059418988));
#49457=CARTESIAN_POINT('Ctrl Pts',(-21.,2.5197596307744,6.94531805563895));
#49458=CARTESIAN_POINT('Ctrl Pts',(-21.,2.55437015138428,7.03952961984441));
#49459=CARTESIAN_POINT('Ctrl Pts',(-21.,2.59029498067661,7.13325283216217));
#49460=CARTESIAN_POINT('Ctrl Pts',(-21.,2.62718125254576,7.22662075191781));
#49461=CARTESIAN_POINT('Ctrl Pts',(-21.,2.66442452752942,7.31986152676826));
#49462=CARTESIAN_POINT('Ctrl Pts',(-21.,2.70112557395893,7.41331375298832));
#49463=CARTESIAN_POINT('Ctrl Pts',(-21.,2.73622951961898,7.50736587770304));
#49464=CARTESIAN_POINT('Ctrl Pts',(-21.,2.76864747338962,7.60240247767684));
#49465=CARTESIAN_POINT('Ctrl Pts',(-21.,2.79737835816915,7.69875126136884));
#49466=CARTESIAN_POINT('Ctrl Pts',(-21.,2.82164615909785,7.79662146983088));
#49467=CARTESIAN_POINT('Ctrl Pts',(-21.,2.84098400021345,7.89607078269802));
#49468=CARTESIAN_POINT('Ctrl Pts',(-21.,2.85517326277626,7.9970485375799));
#49469=CARTESIAN_POINT('Ctrl Pts',(-21.,2.86421236488386,8.099424390731));
#49470=CARTESIAN_POINT('Ctrl Pts',(-21.,2.8682745946465,8.20302084448955));
#49471=CARTESIAN_POINT('Ctrl Pts',(-21.,2.86767474496505,8.30764661663281));
#49472=CARTESIAN_POINT('Ctrl Pts',(-21.,2.86282492937103,8.41311873833255));
#49473=CARTESIAN_POINT('Ctrl Pts',(-21.,2.85417908993455,8.51926543389428));
#49474=CARTESIAN_POINT('Ctrl Pts',(-21.,2.84217845398458,8.62593402210748));
#49475=CARTESIAN_POINT('Ctrl Pts',(-21.,2.82720199177778,8.73299593720093));
#49476=CARTESIAN_POINT('Ctrl Pts',(-21.,2.80950303716262,8.84035511450549));
#49477=CARTESIAN_POINT('Ctrl Pts',(-21.,2.79193132752196,8.93344861295375));
#49478=CARTESIAN_POINT('Ctrl Pts',(-21.,2.77699071660796,9.0051285824934));
#49479=CARTESIAN_POINT('Ctrl Pts',(-21.,2.76583572100211,9.05530311062091));
#49480=CARTESIAN_POINT('Ctrl Pts',(-21.,2.75924496093974,9.08392172878324));
#49481=CARTESIAN_POINT('Ctrl Pts',(-21.,2.75760981235205,9.09096189205629));
#49482=CARTESIAN_POINT('',(-21.,1.44663677770972,9.38920880763537));
#49483=CARTESIAN_POINT('Origin',(-21.,0.,0.));
#49484=CARTESIAN_POINT('',(-21.,0.718643267461623,7.15148293042304));
#49485=CARTESIAN_POINT('Ctrl Pts',(-21.,1.44663677770972,9.38920880763537));
#49486=CARTESIAN_POINT('Ctrl Pts',(-21.,1.43427746833275,9.37515540804603));
#49487=CARTESIAN_POINT('Ctrl Pts',(-21.,1.40471132872148,9.34045308130916));
#49488=CARTESIAN_POINT('Ctrl Pts',(-21.,1.36116944796064,9.28502749443539));
#49489=CARTESIAN_POINT('Ctrl Pts',(-21.,1.30834989113785,9.2086934591593));
#49490=CARTESIAN_POINT('Ctrl Pts',(-21.,1.24851405668088,9.11085713692575));
#49491=CARTESIAN_POINT('Ctrl Pts',(-21.,1.18634328973517,9.00492385207762));
#49492=CARTESIAN_POINT('Ctrl Pts',(-21.,1.12259642171968,8.89721129760285));
#49493=CARTESIAN_POINT('Ctrl Pts',(-21.,1.05830577327405,8.78766206238304));
#49494=CARTESIAN_POINT('Ctrl Pts',(-21.,0.996589197042052,8.67637972666424));
#49495=CARTESIAN_POINT('Ctrl Pts',(-21.,0.941323460369316,8.56356426545847));
#49496=CARTESIAN_POINT('Ctrl Pts',(-21.,0.895240742652423,8.44941362598824));
#49497=CARTESIAN_POINT('Ctrl Pts',(-21.,0.858916682261844,8.33407215281038));
#49498=CARTESIAN_POINT('Ctrl Pts',(-21.,0.831570515383446,8.21766862525226));
#49499=CARTESIAN_POINT('Ctrl Pts',(-21.,0.811510144890448,8.10033651802127));
#49500=CARTESIAN_POINT('Ctrl Pts',(-21.,0.796736942256154,7.98224460192821));
#49501=CARTESIAN_POINT('Ctrl Pts',(-21.,0.785400272847098,7.86361381479518));
#49502=CARTESIAN_POINT('Ctrl Pts',(-21.,0.775839563797132,7.74468091618948));
#49503=CARTESIAN_POINT('Ctrl Pts',(-21.,0.766672302003445,7.62566969516693));
#49504=CARTESIAN_POINT('Ctrl Pts',(-21.,0.756870878958096,7.5067579169994));
#49505=CARTESIAN_POINT('Ctrl Pts',(-21.,0.745831500234843,7.38804974272502));
#49506=CARTESIAN_POINT('Ctrl Pts',(-21.,0.735771087779772,7.29328733826105));
#49507=CARTESIAN_POINT('Ctrl Pts',(-21.,0.72749213560466,7.22233768688913));
#49508=CARTESIAN_POINT('Ctrl Pts',(-21.,0.721647166649911,7.17509214524366));
#49509=CARTESIAN_POINT('Ctrl Pts',(-21.,0.718643267461623,7.15148293042304));
#49510=CARTESIAN_POINT('',(-21.,-0.718643267461628,7.15148293042304));
#49511=CARTESIAN_POINT('Origin',(-21.,0.,0.));
#49512=CARTESIAN_POINT('',(-21.,-1.45989994714919,9.38715570044056));
#49513=CARTESIAN_POINT('Ctrl Pts',(-21.,-0.718643267461623,7.15148293042304));
#49514=CARTESIAN_POINT('Ctrl Pts',(-21.,-0.721388610069065,7.17138797035723));
#49515=CARTESIAN_POINT('Ctrl Pts',(-21.,-0.726715875322121,7.21121317182152));
#49516=CARTESIAN_POINT('Ctrl Pts',(-21.,-0.734216502709279,7.2709963393441));
#49517=CARTESIAN_POINT('Ctrl Pts',(-21.,-0.743235585416284,7.35079807608913));
#49518=CARTESIAN_POINT('Ctrl Pts',(-21.,-0.752929449590466,7.45069670452966));
#49519=CARTESIAN_POINT('Ctrl Pts',(-21.,-0.761227274615912,7.55072560028829));
#49520=CARTESIAN_POINT('Ctrl Pts',(-21.,-0.768504714146027,7.65085154280962));
#49521=CARTESIAN_POINT('Ctrl Pts',(-21.,-0.775405338877351,7.75101782957587));
#49522=CARTESIAN_POINT('Ctrl Pts',(-21.,-0.782886239966145,7.85113936329068));
#49523=CARTESIAN_POINT('Ctrl Pts',(-21.,-0.792066365329069,7.95110843081948));
#49524=CARTESIAN_POINT('Ctrl Pts',(-21.,-0.804093633570273,8.05079907170372));
#49525=CARTESIAN_POINT('Ctrl Pts',(-21.,-0.82001217136434,8.15007218998677));
#49526=CARTESIAN_POINT('Ctrl Pts',(-21.,-0.840611930230858,8.24877960511329));
#49527=CARTESIAN_POINT('Ctrl Pts',(-21.,-0.86633857713272,8.34677071475058));
#49528=CARTESIAN_POINT('Ctrl Pts',(-21.,-0.897367099160985,8.4439050185459));
#49529=CARTESIAN_POINT('Ctrl Pts',(-21.,-0.933642367528788,8.5400643944807));
#49530=CARTESIAN_POINT('Ctrl Pts',(-21.,-0.974931241694467,8.63516410958082));
#49531=CARTESIAN_POINT('Ctrl Pts',(-21.,-1.02086710880846,8.72916840803945));
#49532=CARTESIAN_POINT('Ctrl Pts',(-21.,-1.07099928020948,8.82209124999857));
#49533=CARTESIAN_POINT('Ctrl Pts',(-21.,-1.12484423754393,8.91397482898789));
#49534=CARTESIAN_POINT('Ctrl Pts',(-21.,-1.18193820283021,9.00487302535333));
#49535=CARTESIAN_POINT('Ctrl Pts',(-21.,-1.24188395306769,9.09483443436949));
#49536=CARTESIAN_POINT('Ctrl Pts',(-21.,-1.30441156144786,9.18388242219763));
#49537=CARTESIAN_POINT('Ctrl Pts',(-21.,-1.36063487998417,9.26013268702205));
#49538=CARTESIAN_POINT('Ctrl Pts',(-21.,-1.40519667848884,9.3182316199014));
#49539=CARTESIAN_POINT('Ctrl Pts',(-21.,-1.43701689412372,9.35859733650268));
#49540=CARTESIAN_POINT('Ctrl Pts',(-21.,-1.45537211681237,9.38152219688984));
#49541=CARTESIAN_POINT('Ctrl Pts',(-21.,-1.45989994714919,9.38715570044056));
#49542=CARTESIAN_POINT('',(-21.,-2.77045032493322,9.08705700417233));
#49543=CARTESIAN_POINT('Origin',(-21.,0.,0.));
#49544=CARTESIAN_POINT('',(-21.,-2.45543694297674,6.75507110762463));
#49545=CARTESIAN_POINT('Ctrl Pts',(-21.,-2.77045032493322,9.08705700417233));
#49546=CARTESIAN_POINT('Ctrl Pts',(-21.,-2.7754881363495,9.06903282528875));
#49547=CARTESIAN_POINT('Ctrl Pts',(-21.,-2.78706953240265,9.02493884204925));
#49548=CARTESIAN_POINT('Ctrl Pts',(-21.,-2.8022511505425,8.95610999975804));
#49549=CARTESIAN_POINT('Ctrl Pts',(-21.,-2.81671983020872,8.86441786360011));
#49550=CARTESIAN_POINT('Ctrl Pts',(-21.,-2.8281804649272,8.7503085875302));
#49551=CARTESIAN_POINT('Ctrl Pts',(-21.,-2.838231660712,8.62789111098118));
#49552=CARTESIAN_POINT('Ctrl Pts',(-21.,-2.84893087833482,8.50318672326558));
#49553=CARTESIAN_POINT('Ctrl Pts',(-21.,-2.85932311928695,8.37659160589212));
#49554=CARTESIAN_POINT('Ctrl Pts',(-21.,-2.8666442371861,8.24955186700095));
#49555=CARTESIAN_POINT('Ctrl Pts',(-21.,-2.86748815125169,8.12392974416385));
#49556=CARTESIAN_POINT('Ctrl Pts',(-21.,-2.85947913898695,8.00108902987832));
#49557=CARTESIAN_POINT('Ctrl Pts',(-21.,-2.84216119689693,7.88140953422486));
#49558=CARTESIAN_POINT('Ctrl Pts',(-21.,-2.81629364412744,7.76466852264525));
#49559=CARTESIAN_POINT('Ctrl Pts',(-21.,-2.78345892001629,7.65025207826714));
#49560=CARTESIAN_POINT('Ctrl Pts',(-21.,-2.74553095355499,7.53744508591865));
#49561=CARTESIAN_POINT('Ctrl Pts',(-21.,-2.70427297026251,7.42564364342468));
#49562=CARTESIAN_POINT('Ctrl Pts',(-21.,-2.66128382072048,7.31434056822034));
#49563=CARTESIAN_POINT('Ctrl Pts',(-21.,-2.61790620462629,7.20313763732345));
#49564=CARTESIAN_POINT('Ctrl Pts',(-21.,-2.57514309471485,7.09174914908801));
#49565=CARTESIAN_POINT('Ctrl Pts',(-21.,-2.53358368474749,6.98000697278327));
#49566=CARTESIAN_POINT('Ctrl Pts',(-21.,-2.50153193679118,6.89026394714059));
#49567=CARTESIAN_POINT('Ctrl Pts',(-21.,-2.47820711493347,6.82274841734025));
#49568=CARTESIAN_POINT('Ctrl Pts',(-21.,-2.46297417772978,6.77764561818537));
#49569=CARTESIAN_POINT('Ctrl Pts',(-21.,-2.45543694297674,6.75507110762463));
#49570=CARTESIAN_POINT('',(-21.,-3.75038736519794,6.13145585166881));
#49571=CARTESIAN_POINT('Origin',(-21.,0.,0.));
#49572=CARTESIAN_POINT('',(-21.,-5.38825861761966,7.82410819644306));
#49573=CARTESIAN_POINT('Ctrl Pts',(-21.,-3.75038736519793,6.13145585166881));
#49574=CARTESIAN_POINT('Ctrl Pts',(-21.,-3.7614973065729,6.1481985134482));
#49575=CARTESIAN_POINT('Ctrl Pts',(-21.,-3.78357651403939,6.1817683663582));
#49576=CARTESIAN_POINT('Ctrl Pts',(-21.,-3.81627329006595,6.23237673886416));
#49577=CARTESIAN_POINT('Ctrl Pts',(-21.,-3.859023878729,6.30036238594766));
#49578=CARTESIAN_POINT('Ctrl Pts',(-21.,-3.91110213900011,6.38616193008433));
#49579=CARTESIAN_POINT('Ctrl Pts',(-21.,-3.96197913233089,6.47268455970493));
#49580=CARTESIAN_POINT('Ctrl Pts',(-21.,-4.01197889710939,6.55973735411151));
#49581=CARTESIAN_POINT('Ctrl Pts',(-21.,-4.06165666819706,6.64698999124062));
#49582=CARTESIAN_POINT('Ctrl Pts',(-21.,-4.11183783259628,6.73395053478792));
#49583=CARTESIAN_POINT('Ctrl Pts',(-21.,-4.16348379256721,6.82003644526658));
#49584=CARTESIAN_POINT('Ctrl Pts',(-21.,-4.21757413484033,6.90463617300865));
#49585=CARTESIAN_POINT('Ctrl Pts',(-21.,-4.27498923356982,6.98717136730191));
#49586=CARTESIAN_POINT('Ctrl Pts',(-21.,-4.33637651734857,7.06716577496009));
#49587=CARTESIAN_POINT('Ctrl Pts',(-21.,-4.40207217433237,7.14429034032177));
#49588=CARTESIAN_POINT('Ctrl Pts',(-21.,-4.47217290162416,7.21834255288981));
#49589=CARTESIAN_POINT('Ctrl Pts',(-21.,-4.54657777868016,7.28923990788708));
#49590=CARTESIAN_POINT('Ctrl Pts',(-21.,-4.62503998887083,7.35700721943171));
#49591=CARTESIAN_POINT('Ctrl Pts',(-21.,-4.70721371156899,7.42177134000892));
#49592=CARTESIAN_POINT('Ctrl Pts',(-21.,-4.79269894740031,7.48374039375355));
#49593=CARTESIAN_POINT('Ctrl Pts',(-21.,-4.88107836846757,7.54316218647348));
#49594=CARTESIAN_POINT('Ctrl Pts',(-21.,-4.9719575030537,7.60028648840776));
#49595=CARTESIAN_POINT('Ctrl Pts',(-21.,-5.06499955030094,7.65532943098672));
#49596=CARTESIAN_POINT('Ctrl Pts',(-21.,-5.15997145275563,7.70842918324715));
#49597=CARTESIAN_POINT('Ctrl Pts',(-21.,-5.24371066241773,7.75273391435114));
#49598=CARTESIAN_POINT('Ctrl Pts',(-21.,-5.30906763780461,7.78574460437678));
#49599=CARTESIAN_POINT('Ctrl Pts',(-21.,-5.3552506895127,7.80830658422592));
#49600=CARTESIAN_POINT('Ctrl Pts',(-21.,-5.38173489786212,7.82099713708327));
#49601=CARTESIAN_POINT('Ctrl Pts',(-21.,-5.38825861761966,7.82410819644306));
#49602=CARTESIAN_POINT('',(-21.,-6.43881576337966,6.98510211559242));
#49603=CARTESIAN_POINT('Origin',(-21.,0.,0.));
#49604=CARTESIAN_POINT('',(-21.,-5.14318775290069,5.02073460645076));
#49605=CARTESIAN_POINT('Ctrl Pts',(-21.,-6.43881576337966,6.98510211559242));
#49606=CARTESIAN_POINT('Ctrl Pts',(-21.,-6.43553427649956,6.96667706709454));
#49607=CARTESIAN_POINT('Ctrl Pts',(-21.,-6.42683709146975,6.92192478151019));
#49608=CARTESIAN_POINT('Ctrl Pts',(-21.,-6.4106515413257,6.85332508014768));
#49609=CARTESIAN_POINT('Ctrl Pts',(-21.,-6.38390364438073,6.76443559520424));
#49610=CARTESIAN_POINT('Ctrl Pts',(-21.,-6.34471916009928,6.65665410688205));
#49611=CARTESIAN_POINT('Ctrl Pts',(-21.,-6.30066002212815,6.5419987212145));
#49612=CARTESIAN_POINT('Ctrl Pts',(-21.,-6.25619247809081,6.42500173364409));
#49613=CARTESIAN_POINT('Ctrl Pts',(-21.,-6.2106280007764,6.30643444970003));
#49614=CARTESIAN_POINT('Ctrl Pts',(-21.,-6.16210362315516,6.18879908596403));
#49615=CARTESIAN_POINT('Ctrl Pts',(-21.,-6.108358567083,6.07525130357771));
#49616=CARTESIAN_POINT('Ctrl Pts',(-21.,-6.04784410793973,5.96805062448362));
#49617=CARTESIAN_POINT('Ctrl Pts',(-21.,-5.98031419419066,5.86773709824143));
#49618=CARTESIAN_POINT('Ctrl Pts',(-21.,-5.906356307844,5.77378059171821));
#49619=CARTESIAN_POINT('Ctrl Pts',(-21.,-5.82712980893039,5.68494139022769));
#49620=CARTESIAN_POINT('Ctrl Pts',(-21.,-5.74401277228714,5.59976212994534));
#49621=CARTESIAN_POINT('Ctrl Pts',(-21.,-5.65833178588016,5.51693367893109));
#49622=CARTESIAN_POINT('Ctrl Pts',(-21.,-5.57130730604024,5.43530536621495));
#49623=CARTESIAN_POINT('Ctrl Pts',(-21.,-5.48397628091718,5.35393582972231));
#49624=CARTESIAN_POINT('Ctrl Pts',(-21.,-5.39711839642203,5.27213248760413));
#49625=CARTESIAN_POINT('Ctrl Pts',(-21.,-5.31119154860082,5.18948821771405));
#49626=CARTESIAN_POINT('Ctrl Pts',(-21.,-5.24337588200476,5.12253927774717));
#49627=CARTESIAN_POINT('Ctrl Pts',(-21.,-5.19306705314332,5.071830148219));
#49628=CARTESIAN_POINT('Ctrl Pts',(-21.,-5.1597732798141,5.03780325407688));
#49629=CARTESIAN_POINT('Ctrl Pts',(-21.,-5.14318775290069,5.02073460645076));
#49630=CARTESIAN_POINT('',(-21.,-6.03932124977422,3.89701874412038));
#49631=CARTESIAN_POINT('Origin',(-21.,0.,0.));
#49632=CARTESIAN_POINT('',(-21.,-8.24940658621529,4.71140010775012));
#49633=CARTESIAN_POINT('Ctrl Pts',(-21.,-6.03932124977421,3.89701874412039));
#49634=CARTESIAN_POINT('Ctrl Pts',(-21.,-6.0565953297729,3.90728293824429));
#49635=CARTESIAN_POINT('Ctrl Pts',(-21.,-6.09105342163039,3.92794852152394));
#49636=CARTESIAN_POINT('Ctrl Pts',(-21.,-6.14247034880463,3.95935849016754));
#49637=CARTESIAN_POINT('Ctrl Pts',(-21.,-6.21048516503746,4.00206265639536));
#49638=CARTESIAN_POINT('Ctrl Pts',(-21.,-6.29463308326085,4.05676946424956));
#49639=CARTESIAN_POINT('Ctrl Pts',(-21.,-6.37801243240243,4.11264895980536));
#49640=CARTESIAN_POINT('Ctrl Pts',(-21.,-6.46083145580807,4.1693867325325));
#49641=CARTESIAN_POINT('Ctrl Pts',(-21.,-6.54344708143028,4.22644426515767));
#49642=CARTESIAN_POINT('Ctrl Pts',(-21.,-6.62638951409907,4.28302021638686));
#49643=CARTESIAN_POINT('Ctrl Pts',(-21.,-6.71027219290964,4.33817259947066));
#49644=CARTESIAN_POINT('Ctrl Pts',(-21.,-6.79571235355295,4.39092540044367));
#49645=CARTESIAN_POINT('Ctrl Pts',(-21.,-6.88325224876452,4.44037556328962));
#49646=CARTESIAN_POINT('Ctrl Pts',(-21.,-6.9732685530375,4.48581308997575));
#49647=CARTESIAN_POINT('Ctrl Pts',(-21.,-7.06592138953324,4.5267956450212));
#49648=CARTESIAN_POINT('Ctrl Pts',(-21.,-7.16121001331941,4.56309881747208));
#49649=CARTESIAN_POINT('Ctrl Pts',(-21.,-7.25900770064673,4.59469206087561));
#49650=CARTESIAN_POINT('Ctrl Pts',(-21.,-7.35910284385827,4.62170482170181));
#49651=CARTESIAN_POINT('Ctrl Pts',(-21.,-7.46123890856565,4.64440143603747));
#49652=CARTESIAN_POINT('Ctrl Pts',(-21.,-7.56514580946327,4.66314297047291));
#49653=CARTESIAN_POINT('Ctrl Pts',(-21.,-7.67055506601851,4.67833376211481));
#49654=CARTESIAN_POINT('Ctrl Pts',(-21.,-7.77721964274024,4.69037000103626));
#49655=CARTESIAN_POINT('Ctrl Pts',(-21.,-7.8849298684541,4.69959254734285));
#49656=CARTESIAN_POINT('Ctrl Pts',(-21.,-7.99353571494822,4.70622700687469));
#49657=CARTESIAN_POINT('Ctrl Pts',(-21.,-8.08820523826853,4.70981110890122));
#49658=CARTESIAN_POINT('Ctrl Pts',(-21.,-8.16141264001154,4.71119538406403));
#49659=CARTESIAN_POINT('Ctrl Pts',(-21.,-8.2128114080041,4.71148495034738));
#49660=CARTESIAN_POINT('Ctrl Pts',(-21.,-8.24217907974318,4.71142767604211));
#49661=CARTESIAN_POINT('Ctrl Pts',(-21.,-8.24940658621529,4.71140010775012));
#49662=CARTESIAN_POINT('',(-21.,-8.83189477299562,3.49966208636385));
#49663=CARTESIAN_POINT('Origin',(-21.,0.,0.));
#49664=CARTESIAN_POINT('',(-21.,-6.8122671513043,2.29198004120026));
#49665=CARTESIAN_POINT('Ctrl Pts',(-21.,-8.83189477299562,3.49966208636385));
#49666=CARTESIAN_POINT('Ctrl Pts',(-21.,-8.82094392654054,3.48448547507508));
#49667=CARTESIAN_POINT('Ctrl Pts',(-21.,-8.7936907445869,3.44793862615663));
#49668=CARTESIAN_POINT('Ctrl Pts',(-21.,-8.74934377286773,3.39315507789778));
#49669=CARTESIAN_POINT('Ctrl Pts',(-21.,-8.68667704834296,3.32467389681987));
#49670=CARTESIAN_POINT('Ctrl Pts',(-21.,-8.60460841273967,3.24456764186082));
#49671=CARTESIAN_POINT('Ctrl Pts',(-21.,-8.51516539363766,3.16038325236223));
#49672=CARTESIAN_POINT('Ctrl Pts',(-21.,-8.4243384303954,3.07426635319921));
#49673=CARTESIAN_POINT('Ctrl Pts',(-21.,-8.33184183835821,2.98721060740198));
#49674=CARTESIAN_POINT('Ctrl Pts',(-21.,-8.2370828133169,2.90227874531213));
#49675=CARTESIAN_POINT('Ctrl Pts',(-21.,-8.13939365460193,2.82329483425037));
#49676=CARTESIAN_POINT('Ctrl Pts',(-21.,-8.03835937937461,2.75296659957235));
#49677=CARTESIAN_POINT('Ctrl Pts',(-21.,-7.93399262158453,2.69188736687836));
#49678=CARTESIAN_POINT('Ctrl Pts',(-21.,-7.82659266808561,2.63932460382938));
#49679=CARTESIAN_POINT('Ctrl Pts',(-21.,-7.71666617412861,2.59365833862295));
#49680=CARTESIAN_POINT('Ctrl Pts',(-21.,-7.60482241577417,2.55297760756074));
#49681=CARTESIAN_POINT('Ctrl Pts',(-21.,-7.49168859641893,2.51552733857386));
#49682=CARTESIAN_POINT('Ctrl Pts',(-21.,-7.37786505179862,2.47974127678492));
#49683=CARTESIAN_POINT('Ctrl Pts',(-21.,-7.26387759821705,2.44432136933076));
#49684=CARTESIAN_POINT('Ctrl Pts',(-21.,-7.15012820840451,2.4083053284885));
#49685=CARTESIAN_POINT('Ctrl Pts',(-21.,-7.03685278876406,2.37112767623027));
#49686=CARTESIAN_POINT('Ctrl Pts',(-21.,-6.94670492800217,2.34023288057449));
#49687=CARTESIAN_POINT('Ctrl Pts',(-21.,-6.8793763726903,2.31637371632821));
#49688=CARTESIAN_POINT('Ctrl Pts',(-21.,-6.83461600336474,2.30016217089616));
#49689=CARTESIAN_POINT('Ctrl Pts',(-21.,-6.8122671513043,2.29198004120026));
#49690=CARTESIAN_POINT('',(-21.,-7.13209349341826,0.890729280500487));
#49691=CARTESIAN_POINT('Origin',(-21.,0.,0.));
#49692=CARTESIAN_POINT('',(-21.,-9.47665840807863,0.665541446186861));
#49693=CARTESIAN_POINT('Ctrl Pts',(-21.,-7.13209349341826,0.890729280500492));
#49694=CARTESIAN_POINT('Ctrl Pts',(-21.,-7.15211036864424,0.892482057440589));
#49695=CARTESIAN_POINT('Ctrl Pts',(-21.,-7.19212249719958,0.89615029887462));
#49696=CARTESIAN_POINT('Ctrl Pts',(-21.,-7.25207582250743,0.902140734147994));
#49697=CARTESIAN_POINT('Ctrl Pts',(-21.,-7.33188369780814,0.911105335666499));
#49698=CARTESIAN_POINT('Ctrl Pts',(-21.,-7.43143474677318,0.923884053007731));
#49699=CARTESIAN_POINT('Ctrl Pts',(-21.,-7.53080214904746,0.938052795086852));
#49700=CARTESIAN_POINT('Ctrl Pts',(-21.,-7.63003710778607,0.953237934402831));
#49701=CARTESIAN_POINT('Ctrl Pts',(-21.,-7.7292275500742,0.968799418422935));
#49702=CARTESIAN_POINT('Ctrl Pts',(-21.,-7.82850348500033,0.983785216334555));
#49703=CARTESIAN_POINT('Ctrl Pts',(-21.,-7.92800888935854,0.997080466154163));
#49704=CARTESIAN_POINT('Ctrl Pts',(-21.,-8.02787639670185,1.00753800115478));
#49705=CARTESIAN_POINT('Ctrl Pts',(-21.,-8.12820273854249,1.01410892133532));
#49706=CARTESIAN_POINT('Ctrl Pts',(-21.,-8.2290192302709,1.01599010763451));
#49707=CARTESIAN_POINT('Ctrl Pts',(-21.,-8.33027821569813,1.01271355471894));
#49708=CARTESIAN_POINT('Ctrl Pts',(-21.,-8.43188165539955,1.00407739851957));
#49709=CARTESIAN_POINT('Ctrl Pts',(-21.,-8.53370212161309,0.990109101007577));
#49710=CARTESIAN_POINT('Ctrl Pts',(-21.,-8.63560512714608,0.971017102543951));
#49711=CARTESIAN_POINT('Ctrl Pts',(-21.,-8.73747423363077,0.947150867813171));
#49712=CARTESIAN_POINT('Ctrl Pts',(-21.,-8.83922276353739,0.918952892194649));
#49713=CARTESIAN_POINT('Ctrl Pts',(-21.,-8.94078425956014,0.886903960171005));
#49714=CARTESIAN_POINT('Ctrl Pts',(-21.,-9.04210805084257,0.851468211346448));
#49715=CARTESIAN_POINT('Ctrl Pts',(-21.,-9.14315312384119,0.813043722977555));
#49716=CARTESIAN_POINT('Ctrl Pts',(-21.,-9.24388219451328,0.771898853704203));
#49717=CARTESIAN_POINT('Ctrl Pts',(-21.,-9.33073157135269,0.734052451290806));
#49718=CARTESIAN_POINT('Ctrl Pts',(-21.,-9.39728977570677,0.703536138917768));
#49719=CARTESIAN_POINT('Ctrl Pts',(-21.,-9.44372410361835,0.681495939481608));
#49720=CARTESIAN_POINT('Ctrl Pts',(-21.,-9.47015861118831,0.668702181892298));
#49721=CARTESIAN_POINT('Ctrl Pts',(-21.,-9.47665840807863,0.665541446186861));
#49722=CARTESIAN_POINT('',(-21.,-9.47570870673866,-0.6789289396079));
#49723=CARTESIAN_POINT('Origin',(-21.,0.,0.));
#49724=CARTESIAN_POINT('',(-21.,-7.13209349341826,-0.89072928050049));
#49725=CARTESIAN_POINT('Ctrl Pts',(-21.,-9.47570870673866,-0.6789289396079));
#49726=CARTESIAN_POINT('Ctrl Pts',(-21.,-9.45925745015235,-0.687851199692912));
#49727=CARTESIAN_POINT('Ctrl Pts',(-21.,-9.41884609819914,-0.708954060299465));
#49728=CARTESIAN_POINT('Ctrl Pts',(-21.,-9.35512116653373,-0.739070901845867));
#49729=CARTESIAN_POINT('Ctrl Pts',(-21.,-9.26894752777823,-0.77358024127919));
#49730=CARTESIAN_POINT('Ctrl Pts',(-21.,-9.1602494406401,-0.810145236641717));
#49731=CARTESIAN_POINT('Ctrl Pts',(-21.,-9.04313782728701,-0.847184879177381));
#49732=CARTESIAN_POINT('Ctrl Pts',(-21.,-8.92394083882956,-0.885365181899303));
#49733=CARTESIAN_POINT('Ctrl Pts',(-21.,-8.80283221651881,-0.923666931425906));
#49734=CARTESIAN_POINT('Ctrl Pts',(-21.,-8.68060673111004,-0.959073494961789));
#49735=CARTESIAN_POINT('Ctrl Pts',(-21.,-8.55832200571467,-0.98784980243911));
#49736=CARTESIAN_POINT('Ctrl Pts',(-21.,-8.43677899171613,-1.00737622330388));
#49737=CARTESIAN_POINT('Ctrl Pts',(-21.,-8.31624650623966,-1.017123671327));
#49738=CARTESIAN_POINT('Ctrl Pts',(-21.,-8.19667636355292,-1.01788199103989));
#49739=CARTESIAN_POINT('Ctrl Pts',(-21.,-8.0778221648407,-1.01133055607812));
#49740=CARTESIAN_POINT('Ctrl Pts',(-21.,-7.95940371279084,-0.999455440216892));
#49741=CARTESIAN_POINT('Ctrl Pts',(-21.,-7.84122460090589,-0.984110042106142));
#49742=CARTESIAN_POINT('Ctrl Pts',(-21.,-7.72314614047142,-0.966965984543332));
#49743=CARTESIAN_POINT('Ctrl Pts',(-21.,-7.60507887157754,-0.949420915891056));
#49744=CARTESIAN_POINT('Ctrl Pts',(-21.,-7.4869674381447,-0.932516236860826));
#49745=CARTESIAN_POINT('Ctrl Pts',(-21.,-7.36877903277666,-0.916863781503486));
#49746=CARTESIAN_POINT('Ctrl Pts',(-21.,-7.27415386726379,-0.90558533966873));
#49747=CARTESIAN_POINT('Ctrl Pts',(-21.,-7.20314083161155,-0.89786893854071));
#49748=CARTESIAN_POINT('Ctrl Pts',(-21.,-7.15577920638447,-0.893054239868308));
#49749=CARTESIAN_POINT('Ctrl Pts',(-21.,-7.13209349341826,-0.89072928050049));
#49750=CARTESIAN_POINT('',(-21.,-6.8122671513043,-2.29198004120026));
#49751=CARTESIAN_POINT('Origin',(-21.,0.,0.));
#49752=CARTESIAN_POINT('',(-21.,-8.82694180863381,-3.51213586112389));
#49753=CARTESIAN_POINT('Ctrl Pts',(-21.,-6.8122671513043,-2.29198004120026));
#49754=CARTESIAN_POINT('Ctrl Pts',(-21.,-6.8310622341282,-2.29908584041335));
#49755=CARTESIAN_POINT('Ctrl Pts',(-21.,-6.86870350660446,-2.31314148102898));
#49756=CARTESIAN_POINT('Ctrl Pts',(-21.,-6.92531873868941,-2.33375705829959));
#49757=CARTESIAN_POINT('Ctrl Pts',(-21.,-7.00111274457534,-2.36030757076476));
#49758=CARTESIAN_POINT('Ctrl Pts',(-21.,-7.09634961812101,-2.39198792562662));
#49759=CARTESIAN_POINT('Ctrl Pts',(-21.,-7.19202414084635,-2.42233623016115));
#49760=CARTESIAN_POINT('Ctrl Pts',(-21.,-7.28802033430286,-2.45171132733138));
#49761=CARTESIAN_POINT('Ctrl Pts',(-21.,-7.3841397096708,-2.4807280346756));
#49762=CARTESIAN_POINT('Ctrl Pts',(-21.,-7.4800863304027,-2.5103005111467));
#49763=CARTESIAN_POINT('Ctrl Pts',(-21.,-7.57550619462173,-2.54149568187359));
#49764=CARTESIAN_POINT('Ctrl Pts',(-21.,-7.67002106404108,-2.5754046559055));
#49765=CARTESIAN_POINT('Ctrl Pts',(-21.,-7.76326299008741,-2.61301442971916));
#49766=CARTESIAN_POINT('Ctrl Pts',(-21.,-7.85491172665132,-2.65506217582471));
#49767=CARTESIAN_POINT('Ctrl Pts',(-21.,-7.94472127708621,-2.70194887521209));
#49768=CARTESIAN_POINT('Ctrl Pts',(-21.,-8.03251572538561,-2.75381386341092));
#49769=CARTESIAN_POINT('Ctrl Pts',(-21.,-8.11819217840571,-2.81057710920625));
#49770=CARTESIAN_POINT('Ctrl Pts',(-21.,-8.201719906256,-2.87199246251599));
#49771=CARTESIAN_POINT('Ctrl Pts',(-21.,-8.28314562863609,-2.93769454582461));
#49772=CARTESIAN_POINT('Ctrl Pts',(-21.,-8.36258324333989,-3.00724707660037));
#49773=CARTESIAN_POINT('Ctrl Pts',(-21.,-8.44018147897284,-3.08018804824792));
#49774=CARTESIAN_POINT('Ctrl Pts',(-21.,-8.51609606529771,-3.15607730017284));
#49775=CARTESIAN_POINT('Ctrl Pts',(-21.,-8.59046276963722,-3.23453838205034));
#49776=CARTESIAN_POINT('Ctrl Pts',(-21.,-8.66336443667969,-3.31531333416059));
#49777=CARTESIAN_POINT('Ctrl Pts',(-21.,-8.72519208281745,-3.38709429686028));
#49778=CARTESIAN_POINT('Ctrl Pts',(-21.,-8.77191842112748,-3.44346706684567));
#49779=CARTESIAN_POINT('Ctrl Pts',(-21.,-8.80419142083552,-3.4834717001977));
#49780=CARTESIAN_POINT('Ctrl Pts',(-21.,-8.82245708581418,-3.50646798047535));
#49781=CARTESIAN_POINT('Ctrl Pts',(-21.,-8.82694180863381,-3.51213586112389));
#49782=CARTESIAN_POINT('',(-21.,-8.24274231917123,-4.72304976257329));
#49783=CARTESIAN_POINT('Origin',(-21.,0.,0.));
#49784=CARTESIAN_POINT('',(-21.,-6.03932124977421,-3.89701874412038));
#49785=CARTESIAN_POINT('Ctrl Pts',(-21.,-8.24274231917123,-4.72304976257329));
#49786=CARTESIAN_POINT('Ctrl Pts',(-21.,-8.22404902558203,-4.72395050842036));
#49787=CARTESIAN_POINT('Ctrl Pts',(-21.,-8.17848346749629,-4.7254297003623));
#49788=CARTESIAN_POINT('Ctrl Pts',(-21.,-8.10800208013598,-4.72491482536916));
#49789=CARTESIAN_POINT('Ctrl Pts',(-21.,-8.0153892731556,-4.71861732525386));
#49790=CARTESIAN_POINT('Ctrl Pts',(-21.,-7.9015907237349,-4.70439891524807));
#49791=CARTESIAN_POINT('Ctrl Pts',(-21.,-7.78000590743498,-4.68695765535521));
#49792=CARTESIAN_POINT('Ctrl Pts',(-21.,-7.65604731918147,-4.66963928443128));
#49793=CARTESIAN_POINT('Ctrl Pts',(-21.,-7.53031371454558,-4.65160090645338));
#49794=CARTESIAN_POINT('Ctrl Pts',(-21.,-7.40483002515176,-4.63046946729401));
#49795=CARTESIAN_POINT('Ctrl Pts',(-21.,-7.28216972266428,-4.60333867057275));
#49796=CARTESIAN_POINT('Ctrl Pts',(-21.,-7.16419105444418,-4.56819583049617));
#49797=CARTESIAN_POINT('Ctrl Pts',(-21.,-7.05136577826386,-4.52468089222283));
#49798=CARTESIAN_POINT('Ctrl Pts',(-21.,-6.94330777957998,-4.47348457408032));
#49799=CARTESIAN_POINT('Ctrl Pts',(-21.,-6.83906640781858,-4.4160130309926));
#49800=CARTESIAN_POINT('Ctrl Pts',(-21.,-6.73752748880879,-4.35393408054299));
#49801=CARTESIAN_POINT('Ctrl Pts',(-21.,-6.63770990687462,-4.2888323596294));
#49802=CARTESIAN_POINT('Ctrl Pts',(-21.,-6.53876341785232,-4.22215377357323));
#49803=CARTESIAN_POINT('Ctrl Pts',(-21.,-6.44000100425059,-4.15511874483724));
#49804=CARTESIAN_POINT('Ctrl Pts',(-21.,-6.34092094513049,-4.08864152493875));
#49805=CARTESIAN_POINT('Ctrl Pts',(-21.,-6.24122821720367,-4.02325912271413));
#49806=CARTESIAN_POINT('Ctrl Pts',(-21.,-6.16086742147115,-3.97204127711522));
#49807=CARTESIAN_POINT('Ctrl Pts',(-21.,-6.10023490810719,-3.93427763849175));
#49808=CARTESIAN_POINT('Ctrl Pts',(-21.,-6.05965257770704,-3.90939030583537));
#49809=CARTESIAN_POINT('Ctrl Pts',(-21.,-6.03932124977421,-3.89701874412038));
#49810=CARTESIAN_POINT('',(-21.,-5.14318775290069,-5.02073460645077));
#49811=CARTESIAN_POINT('Origin',(-21.,0.,0.));
#49812=CARTESIAN_POINT('',(-21.,-6.42894112865204,-6.99419158761942));
#49813=CARTESIAN_POINT('Ctrl Pts',(-21.,-5.14318775290069,-5.02073460645076));
#49814=CARTESIAN_POINT('Ctrl Pts',(-21.,-5.15703844666268,-5.03529159113598));
#49815=CARTESIAN_POINT('Ctrl Pts',(-21.,-5.18485354740602,-5.06428722179623));
#49816=CARTESIAN_POINT('Ctrl Pts',(-21.,-5.22691734521339,-5.10742564369891));
#49817=CARTESIAN_POINT('Ctrl Pts',(-21.,-5.28368554926634,-5.16423261553338));
#49818=CARTESIAN_POINT('Ctrl Pts',(-21.,-5.35574541658332,-5.23409735978387));
#49819=CARTESIAN_POINT('Ctrl Pts',(-21.,-5.42877754716296,-5.30295185702147));
#49820=CARTESIAN_POINT('Ctrl Pts',(-21.,-5.50252175190725,-5.37106909242141));
#49821=CARTESIAN_POINT('Ctrl Pts',(-21.,-5.57653243923659,-5.43891687637388));
#49822=CARTESIAN_POINT('Ctrl Pts',(-21.,-5.65014634083023,-5.50719043557996));
#49823=CARTESIAN_POINT('Ctrl Pts',(-21.,-5.72258159055366,-5.57669744070723));
#49824=CARTESIAN_POINT('Ctrl Pts',(-21.,-5.79302399301176,-5.64825683559838));
#49825=CARTESIAN_POINT('Ctrl Pts',(-21.,-5.86071379627312,-5.72259822644884));
#49826=CARTESIAN_POINT('Ctrl Pts',(-21.,-5.92504262139805,-5.80024683316115));
#49827=CARTESIAN_POINT('Ctrl Pts',(-21.,-5.98561485393513,-5.88145719317904));
#49828=CARTESIAN_POINT('Ctrl Pts',(-21.,-6.04221154361855,-5.96627851638222));
#49829=CARTESIAN_POINT('Ctrl Pts',(-21.,-6.09477471117184,-6.05459405347559));
#49830=CARTESIAN_POINT('Ctrl Pts',(-21.,-6.14338347043832,-6.14616869769857));
#49831=CARTESIAN_POINT('Ctrl Pts',(-21.,-6.18823844577549,-6.2406935262026));
#49832=CARTESIAN_POINT('Ctrl Pts',(-21.,-6.22963155144596,-6.33782488040964));
#49833=CARTESIAN_POINT('Ctrl Pts',(-21.,-6.2678972444421,-6.43721103768399));
#49834=CARTESIAN_POINT('Ctrl Pts',(-21.,-6.30336681095649,-6.53852299564495));
#49835=CARTESIAN_POINT('Ctrl Pts',(-21.,-6.33632590879467,-6.64148049150319));
#49836=CARTESIAN_POINT('Ctrl Pts',(-21.,-6.36696110296949,-6.74588705654512));
#49837=CARTESIAN_POINT('Ctrl Pts',(-21.,-6.3915212948217,-6.8373854795327));
#49838=CARTESIAN_POINT('Ctrl Pts',(-21.,-6.40916104272443,-6.90844938866819));
#49839=CARTESIAN_POINT('Ctrl Pts',(-21.,-6.42088065083439,-6.95849504767608));
#49840=CARTESIAN_POINT('Ctrl Pts',(-21.,-6.42735973425904,-6.9871391553022));
#49841=CARTESIAN_POINT('Ctrl Pts',(-21.,-6.42894112865204,-6.99419158761942));
#49842=CARTESIAN_POINT('',(-21.,-5.37719972469147,-7.83171265565699));
#49843=CARTESIAN_POINT('Origin',(-21.,0.,0.));
#49844=CARTESIAN_POINT('',(-21.,-3.75038736519793,-6.13145585166881));
#49845=CARTESIAN_POINT('Ctrl Pts',(-21.,-5.37719972469147,-7.83171265565699));
#49846=CARTESIAN_POINT('Ctrl Pts',(-21.,-5.35996683015292,-7.82441348350419));
#49847=CARTESIAN_POINT('Ctrl Pts',(-21.,-5.31827188353843,-7.80597603467631));
#49848=CARTESIAN_POINT('Ctrl Pts',(-21.,-5.25499374364742,-7.77493142045055));
#49849=CARTESIAN_POINT('Ctrl Pts',(-21.,-5.17428487068616,-7.72907437791823));
#49850=CARTESIAN_POINT('Ctrl Pts',(-21.,-5.07792505734327,-7.66688869302314));
#49851=CARTESIAN_POINT('Ctrl Pts',(-21.,-4.97594840210465,-7.59842098612654));
#49852=CARTESIAN_POINT('Ctrl Pts',(-21.,-4.87177973271099,-7.52903405731413));
#49853=CARTESIAN_POINT('Ctrl Pts',(-21.,-4.76632422816958,-7.45822827381644));
#49854=CARTESIAN_POINT('Ctrl Pts',(-21.,-4.66243591843162,-7.38474417264741));
#49855=CARTESIAN_POINT('Ctrl Pts',(-21.,-4.56369441608956,-7.30707985875561));
#49856=CARTESIAN_POINT('Ctrl Pts',(-21.,-4.4726472158023,-7.22422822821349));
#49857=CARTESIAN_POINT('Ctrl Pts',(-21.,-4.38987557857684,-7.13606957084443));
#49858=CARTESIAN_POINT('Ctrl Pts',(-21.,-4.31473193577955,-7.04305867353628));
#49859=CARTESIAN_POINT('Ctrl Pts',(-21.,-4.24574967308285,-6.94604996627335));
#49860=CARTESIAN_POINT('Ctrl Pts',(-21.,-4.18120131531612,-6.84606267872027));
#49861=CARTESIAN_POINT('Ctrl Pts',(-21.,-4.11951535961712,-6.74409882925098));
#49862=CARTESIAN_POINT('Ctrl Pts',(-21.,-4.0592984076569,-6.64109222642907));
#49863=CARTESIAN_POINT('Ctrl Pts',(-21.,-3.99940195660266,-6.53784434718121));
#49864=CARTESIAN_POINT('Ctrl Pts',(-21.,-3.93897729264122,-6.43496121510494));
#49865=CARTESIAN_POINT('Ctrl Pts',(-21.,-3.87752560957259,-6.33279865263617));
#49866=CARTESIAN_POINT('Ctrl Pts',(-21.,-3.82734562477572,-6.25178572573963));
#49867=CARTESIAN_POINT('Ctrl Pts',(-21.,-3.78910264658076,-6.19145440139071));
#49868=CARTESIAN_POINT('Ctrl Pts',(-21.,-3.7633374392529,-6.15142367620606));
#49869=CARTESIAN_POINT('Ctrl Pts',(-21.,-3.75038736519793,-6.13145585166881));
#49870=CARTESIAN_POINT('',(-21.,-2.45543694297674,-6.75507110762463));
#49871=CARTESIAN_POINT('Origin',(-21.,0.,0.));
#49872=CARTESIAN_POINT('',(-21.,-2.75760981235205,-9.09096189205629));
#49873=CARTESIAN_POINT('Ctrl Pts',(-21.,-2.45543694297675,-6.75507110762463));
#49874=CARTESIAN_POINT('Ctrl Pts',(-21.,-2.46159994790965,-6.77419608843536));
#49875=CARTESIAN_POINT('Ctrl Pts',(-21.,-2.47407975508802,-6.8123887688799));
#49876=CARTESIAN_POINT('Ctrl Pts',(-21.,-2.49326086758344,-6.8695059418988));
#49877=CARTESIAN_POINT('Ctrl Pts',(-21.,-2.5197596307744,-6.94531805563895));
#49878=CARTESIAN_POINT('Ctrl Pts',(-21.,-2.55437015138428,-7.03952961984441));
#49879=CARTESIAN_POINT('Ctrl Pts',(-21.,-2.59029498067661,-7.13325283216217));
#49880=CARTESIAN_POINT('Ctrl Pts',(-21.,-2.62718125254576,-7.22662075191781));
#49881=CARTESIAN_POINT('Ctrl Pts',(-21.,-2.66442452752942,-7.31986152676826));
#49882=CARTESIAN_POINT('Ctrl Pts',(-21.,-2.70112557395893,-7.41331375298832));
#49883=CARTESIAN_POINT('Ctrl Pts',(-21.,-2.73622951961898,-7.50736587770304));
#49884=CARTESIAN_POINT('Ctrl Pts',(-21.,-2.76864747338962,-7.60240247767684));
#49885=CARTESIAN_POINT('Ctrl Pts',(-21.,-2.79737835816915,-7.69875126136884));
#49886=CARTESIAN_POINT('Ctrl Pts',(-21.,-2.82164615909785,-7.79662146983088));
#49887=CARTESIAN_POINT('Ctrl Pts',(-21.,-2.84098400021346,-7.89607078269802));
#49888=CARTESIAN_POINT('Ctrl Pts',(-21.,-2.85517326277626,-7.9970485375799));
#49889=CARTESIAN_POINT('Ctrl Pts',(-21.,-2.86421236488387,-8.099424390731));
#49890=CARTESIAN_POINT('Ctrl Pts',(-21.,-2.8682745946465,-8.20302084448955));
#49891=CARTESIAN_POINT('Ctrl Pts',(-21.,-2.86767474496505,-8.30764661663281));
#49892=CARTESIAN_POINT('Ctrl Pts',(-21.,-2.86282492937103,-8.41311873833255));
#49893=CARTESIAN_POINT('Ctrl Pts',(-21.,-2.85417908993455,-8.51926543389428));
#49894=CARTESIAN_POINT('Ctrl Pts',(-21.,-2.84217845398458,-8.62593402210748));
#49895=CARTESIAN_POINT('Ctrl Pts',(-21.,-2.82720199177778,-8.73299593720093));
#49896=CARTESIAN_POINT('Ctrl Pts',(-21.,-2.80950303716262,-8.84035511450549));
#49897=CARTESIAN_POINT('Ctrl Pts',(-21.,-2.79193132752197,-8.93344861295375));
#49898=CARTESIAN_POINT('Ctrl Pts',(-21.,-2.77699071660796,-9.0051285824934));
#49899=CARTESIAN_POINT('Ctrl Pts',(-21.,-2.76583572100211,-9.05530311062091));
#49900=CARTESIAN_POINT('Ctrl Pts',(-21.,-2.75924496093975,-9.08392172878324));
#49901=CARTESIAN_POINT('Ctrl Pts',(-21.,-2.75760981235205,-9.09096189205629));
#49902=CARTESIAN_POINT('',(-21.,-1.44663677770972,-9.38920880763537));
#49903=CARTESIAN_POINT('Origin',(-21.,0.,0.));
#49904=CARTESIAN_POINT('',(-21.,-0.718643267461624,-7.15148293042304));
#49905=CARTESIAN_POINT('Ctrl Pts',(-21.,-1.44663677770972,-9.38920880763537));
#49906=CARTESIAN_POINT('Ctrl Pts',(-21.,-1.43427746833275,-9.37515540804603));
#49907=CARTESIAN_POINT('Ctrl Pts',(-21.,-1.40471132872148,-9.34045308130916));
#49908=CARTESIAN_POINT('Ctrl Pts',(-21.,-1.36116944796064,-9.28502749443539));
#49909=CARTESIAN_POINT('Ctrl Pts',(-21.,-1.30834989113785,-9.2086934591593));
#49910=CARTESIAN_POINT('Ctrl Pts',(-21.,-1.24851405668088,-9.11085713692575));
#49911=CARTESIAN_POINT('Ctrl Pts',(-21.,-1.18634328973517,-9.00492385207762));
#49912=CARTESIAN_POINT('Ctrl Pts',(-21.,-1.12259642171968,-8.89721129760285));
#49913=CARTESIAN_POINT('Ctrl Pts',(-21.,-1.05830577327405,-8.78766206238304));
#49914=CARTESIAN_POINT('Ctrl Pts',(-21.,-0.996589197042053,-8.67637972666424));
#49915=CARTESIAN_POINT('Ctrl Pts',(-21.,-0.941323460369318,-8.56356426545847));
#49916=CARTESIAN_POINT('Ctrl Pts',(-21.,-0.895240742652424,-8.44941362598824));
#49917=CARTESIAN_POINT('Ctrl Pts',(-21.,-0.858916682261846,-8.33407215281038));
#49918=CARTESIAN_POINT('Ctrl Pts',(-21.,-0.831570515383447,-8.21766862525226));
#49919=CARTESIAN_POINT('Ctrl Pts',(-21.,-0.811510144890449,-8.10033651802127));
#49920=CARTESIAN_POINT('Ctrl Pts',(-21.,-0.796736942256156,-7.98224460192821));
#49921=CARTESIAN_POINT('Ctrl Pts',(-21.,-0.785400272847099,-7.86361381479518));
#49922=CARTESIAN_POINT('Ctrl Pts',(-21.,-0.775839563797133,-7.74468091618948));
#49923=CARTESIAN_POINT('Ctrl Pts',(-21.,-0.766672302003446,-7.62566969516693));
#49924=CARTESIAN_POINT('Ctrl Pts',(-21.,-0.756870878958097,-7.5067579169994));
#49925=CARTESIAN_POINT('Ctrl Pts',(-21.,-0.745831500234844,-7.38804974272502));
#49926=CARTESIAN_POINT('Ctrl Pts',(-21.,-0.735771087779772,-7.29328733826105));
#49927=CARTESIAN_POINT('Ctrl Pts',(-21.,-0.72749213560466,-7.22233768688913));
#49928=CARTESIAN_POINT('Ctrl Pts',(-21.,-0.721647166649912,-7.17509214524366));
#49929=CARTESIAN_POINT('Ctrl Pts',(-21.,-0.718643267461624,-7.15148293042304));
#49930=CARTESIAN_POINT('',(-21.,0.718643267461627,-7.15148293042304));
#49931=CARTESIAN_POINT('Origin',(-21.,0.,0.));
#49932=CARTESIAN_POINT('',(-21.,1.45989994714919,-9.38715570044056));
#49933=CARTESIAN_POINT('Ctrl Pts',(-21.,0.718643267461621,-7.15148293042304));
#49934=CARTESIAN_POINT('Ctrl Pts',(-21.,0.721388610069064,-7.17138797035723));
#49935=CARTESIAN_POINT('Ctrl Pts',(-21.,0.72671587532212,-7.21121317182152));
#49936=CARTESIAN_POINT('Ctrl Pts',(-21.,0.734216502709278,-7.2709963393441));
#49937=CARTESIAN_POINT('Ctrl Pts',(-21.,0.743235585416283,-7.35079807608913));
#49938=CARTESIAN_POINT('Ctrl Pts',(-21.,0.752929449590465,-7.45069670452966));
#49939=CARTESIAN_POINT('Ctrl Pts',(-21.,0.761227274615911,-7.55072560028829));
#49940=CARTESIAN_POINT('Ctrl Pts',(-21.,0.768504714146026,-7.65085154280962));
#49941=CARTESIAN_POINT('Ctrl Pts',(-21.,0.775405338877349,-7.75101782957587));
#49942=CARTESIAN_POINT('Ctrl Pts',(-21.,0.782886239966143,-7.85113936329068));
#49943=CARTESIAN_POINT('Ctrl Pts',(-21.,0.792066365329068,-7.95110843081948));
#49944=CARTESIAN_POINT('Ctrl Pts',(-21.,0.804093633570272,-8.05079907170372));
#49945=CARTESIAN_POINT('Ctrl Pts',(-21.,0.820012171364339,-8.15007218998677));
#49946=CARTESIAN_POINT('Ctrl Pts',(-21.,0.840611930230857,-8.24877960511329));
#49947=CARTESIAN_POINT('Ctrl Pts',(-21.,0.866338577132719,-8.34677071475058));
#49948=CARTESIAN_POINT('Ctrl Pts',(-21.,0.897367099160984,-8.4439050185459));
#49949=CARTESIAN_POINT('Ctrl Pts',(-21.,0.933642367528787,-8.5400643944807));
#49950=CARTESIAN_POINT('Ctrl Pts',(-21.,0.974931241694465,-8.63516410958082));
#49951=CARTESIAN_POINT('Ctrl Pts',(-21.,1.02086710880845,-8.72916840803945));
#49952=CARTESIAN_POINT('Ctrl Pts',(-21.,1.07099928020948,-8.82209124999857));
#49953=CARTESIAN_POINT('Ctrl Pts',(-21.,1.12484423754393,-8.91397482898789));
#49954=CARTESIAN_POINT('Ctrl Pts',(-21.,1.18193820283021,-9.00487302535333));
#49955=CARTESIAN_POINT('Ctrl Pts',(-21.,1.24188395306769,-9.09483443436949));
#49956=CARTESIAN_POINT('Ctrl Pts',(-21.,1.30441156144786,-9.18388242219763));
#49957=CARTESIAN_POINT('Ctrl Pts',(-21.,1.36063487998417,-9.26013268702205));
#49958=CARTESIAN_POINT('Ctrl Pts',(-21.,1.40519667848883,-9.3182316199014));
#49959=CARTESIAN_POINT('Ctrl Pts',(-21.,1.43701689412372,-9.35859733650268));
#49960=CARTESIAN_POINT('Ctrl Pts',(-21.,1.45537211681237,-9.38152219688984));
#49961=CARTESIAN_POINT('Ctrl Pts',(-21.,1.45989994714919,-9.38715570044056));
#49962=CARTESIAN_POINT('',(-21.,2.77045032493322,-9.08705700417233));
#49963=CARTESIAN_POINT('Origin',(-21.,0.,0.));
#49964=CARTESIAN_POINT('',(-21.,2.45543694297674,-6.75507110762463));
#49965=CARTESIAN_POINT('Ctrl Pts',(-21.,2.77045032493322,-9.08705700417233));
#49966=CARTESIAN_POINT('Ctrl Pts',(-21.,2.7754881363495,-9.06903282528875));
#49967=CARTESIAN_POINT('Ctrl Pts',(-21.,2.78706953240264,-9.02493884204925));
#49968=CARTESIAN_POINT('Ctrl Pts',(-21.,2.8022511505425,-8.95610999975804));
#49969=CARTESIAN_POINT('Ctrl Pts',(-21.,2.81671983020871,-8.86441786360011));
#49970=CARTESIAN_POINT('Ctrl Pts',(-21.,2.8281804649272,-8.7503085875302));
#49971=CARTESIAN_POINT('Ctrl Pts',(-21.,2.838231660712,-8.62789111098118));
#49972=CARTESIAN_POINT('Ctrl Pts',(-21.,2.84893087833482,-8.50318672326558));
#49973=CARTESIAN_POINT('Ctrl Pts',(-21.,2.85932311928695,-8.37659160589212));
#49974=CARTESIAN_POINT('Ctrl Pts',(-21.,2.8666442371861,-8.24955186700095));
#49975=CARTESIAN_POINT('Ctrl Pts',(-21.,2.86748815125169,-8.12392974416385));
#49976=CARTESIAN_POINT('Ctrl Pts',(-21.,2.85947913898695,-8.00108902987832));
#49977=CARTESIAN_POINT('Ctrl Pts',(-21.,2.84216119689693,-7.88140953422486));
#49978=CARTESIAN_POINT('Ctrl Pts',(-21.,2.81629364412744,-7.76466852264525));
#49979=CARTESIAN_POINT('Ctrl Pts',(-21.,2.78345892001629,-7.65025207826714));
#49980=CARTESIAN_POINT('Ctrl Pts',(-21.,2.74553095355499,-7.53744508591865));
#49981=CARTESIAN_POINT('Ctrl Pts',(-21.,2.70427297026251,-7.42564364342468));
#49982=CARTESIAN_POINT('Ctrl Pts',(-21.,2.66128382072048,-7.31434056822034));
#49983=CARTESIAN_POINT('Ctrl Pts',(-21.,2.61790620462629,-7.20313763732345));
#49984=CARTESIAN_POINT('Ctrl Pts',(-21.,2.57514309471485,-7.09174914908801));
#49985=CARTESIAN_POINT('Ctrl Pts',(-21.,2.53358368474749,-6.98000697278327));
#49986=CARTESIAN_POINT('Ctrl Pts',(-21.,2.50153193679118,-6.89026394714059));
#49987=CARTESIAN_POINT('Ctrl Pts',(-21.,2.47820711493347,-6.82274841734025));
#49988=CARTESIAN_POINT('Ctrl Pts',(-21.,2.46297417772978,-6.77764561818537));
#49989=CARTESIAN_POINT('Ctrl Pts',(-21.,2.45543694297674,-6.75507110762463));
#49990=CARTESIAN_POINT('',(-21.,3.75038736519794,-6.13145585166881));
#49991=CARTESIAN_POINT('Origin',(-21.,0.,0.));
#49992=CARTESIAN_POINT('',(-21.,5.38825861761966,-7.82410819644306));
#49993=CARTESIAN_POINT('Ctrl Pts',(-21.,3.75038736519793,-6.13145585166881));
#49994=CARTESIAN_POINT('Ctrl Pts',(-21.,3.7614973065729,-6.1481985134482));
#49995=CARTESIAN_POINT('Ctrl Pts',(-21.,3.78357651403939,-6.1817683663582));
#49996=CARTESIAN_POINT('Ctrl Pts',(-21.,3.81627329006595,-6.23237673886416));
#49997=CARTESIAN_POINT('Ctrl Pts',(-21.,3.859023878729,-6.30036238594766));
#49998=CARTESIAN_POINT('Ctrl Pts',(-21.,3.91110213900011,-6.38616193008433));
#49999=CARTESIAN_POINT('Ctrl Pts',(-21.,3.96197913233089,-6.47268455970493));
#50000=CARTESIAN_POINT('Ctrl Pts',(-21.,4.01197889710939,-6.55973735411151));
#50001=CARTESIAN_POINT('Ctrl Pts',(-21.,4.06165666819706,-6.64698999124062));
#50002=CARTESIAN_POINT('Ctrl Pts',(-21.,4.11183783259628,-6.73395053478792));
#50003=CARTESIAN_POINT('Ctrl Pts',(-21.,4.16348379256721,-6.82003644526658));
#50004=CARTESIAN_POINT('Ctrl Pts',(-21.,4.21757413484032,-6.90463617300865));
#50005=CARTESIAN_POINT('Ctrl Pts',(-21.,4.27498923356982,-6.98717136730191));
#50006=CARTESIAN_POINT('Ctrl Pts',(-21.,4.33637651734857,-7.06716577496009));
#50007=CARTESIAN_POINT('Ctrl Pts',(-21.,4.40207217433237,-7.14429034032177));
#50008=CARTESIAN_POINT('Ctrl Pts',(-21.,4.47217290162416,-7.21834255288981));
#50009=CARTESIAN_POINT('Ctrl Pts',(-21.,4.54657777868016,-7.28923990788708));
#50010=CARTESIAN_POINT('Ctrl Pts',(-21.,4.62503998887083,-7.35700721943171));
#50011=CARTESIAN_POINT('Ctrl Pts',(-21.,4.70721371156899,-7.42177134000892));
#50012=CARTESIAN_POINT('Ctrl Pts',(-21.,4.79269894740031,-7.48374039375355));
#50013=CARTESIAN_POINT('Ctrl Pts',(-21.,4.88107836846757,-7.54316218647348));
#50014=CARTESIAN_POINT('Ctrl Pts',(-21.,4.9719575030537,-7.60028648840776));
#50015=CARTESIAN_POINT('Ctrl Pts',(-21.,5.06499955030093,-7.65532943098672));
#50016=CARTESIAN_POINT('Ctrl Pts',(-21.,5.15997145275563,-7.70842918324715));
#50017=CARTESIAN_POINT('Ctrl Pts',(-21.,5.24371066241773,-7.75273391435114));
#50018=CARTESIAN_POINT('Ctrl Pts',(-21.,5.3090676378046,-7.78574460437678));
#50019=CARTESIAN_POINT('Ctrl Pts',(-21.,5.3552506895127,-7.80830658422591));
#50020=CARTESIAN_POINT('Ctrl Pts',(-21.,5.38173489786212,-7.82099713708327));
#50021=CARTESIAN_POINT('Ctrl Pts',(-21.,5.38825861761966,-7.82410819644306));
#50022=CARTESIAN_POINT('',(-21.,6.43881576337966,-6.98510211559242));
#50023=CARTESIAN_POINT('Origin',(-21.,0.,0.));
#50024=CARTESIAN_POINT('',(-21.,5.14318775290069,-5.02073460645076));
#50025=CARTESIAN_POINT('Ctrl Pts',(-21.,6.43881576337966,-6.98510211559242));
#50026=CARTESIAN_POINT('Ctrl Pts',(-21.,6.43553427649956,-6.96667706709454));
#50027=CARTESIAN_POINT('Ctrl Pts',(-21.,6.42683709146975,-6.9219247815102));
#50028=CARTESIAN_POINT('Ctrl Pts',(-21.,6.4106515413257,-6.85332508014768));
#50029=CARTESIAN_POINT('Ctrl Pts',(-21.,6.38390364438073,-6.76443559520424));
#50030=CARTESIAN_POINT('Ctrl Pts',(-21.,6.34471916009928,-6.65665410688205));
#50031=CARTESIAN_POINT('Ctrl Pts',(-21.,6.30066002212815,-6.5419987212145));
#50032=CARTESIAN_POINT('Ctrl Pts',(-21.,6.25619247809081,-6.42500173364409));
#50033=CARTESIAN_POINT('Ctrl Pts',(-21.,6.2106280007764,-6.30643444970003));
#50034=CARTESIAN_POINT('Ctrl Pts',(-21.,6.16210362315516,-6.18879908596403));
#50035=CARTESIAN_POINT('Ctrl Pts',(-21.,6.108358567083,-6.07525130357771));
#50036=CARTESIAN_POINT('Ctrl Pts',(-21.,6.04784410793973,-5.96805062448362));
#50037=CARTESIAN_POINT('Ctrl Pts',(-21.,5.98031419419066,-5.86773709824143));
#50038=CARTESIAN_POINT('Ctrl Pts',(-21.,5.906356307844,-5.77378059171821));
#50039=CARTESIAN_POINT('Ctrl Pts',(-21.,5.82712980893039,-5.68494139022769));
#50040=CARTESIAN_POINT('Ctrl Pts',(-21.,5.74401277228714,-5.59976212994534));
#50041=CARTESIAN_POINT('Ctrl Pts',(-21.,5.65833178588016,-5.51693367893109));
#50042=CARTESIAN_POINT('Ctrl Pts',(-21.,5.57130730604024,-5.43530536621495));
#50043=CARTESIAN_POINT('Ctrl Pts',(-21.,5.48397628091718,-5.35393582972231));
#50044=CARTESIAN_POINT('Ctrl Pts',(-21.,5.39711839642203,-5.27213248760413));
#50045=CARTESIAN_POINT('Ctrl Pts',(-21.,5.31119154860082,-5.18948821771405));
#50046=CARTESIAN_POINT('Ctrl Pts',(-21.,5.24337588200475,-5.12253927774717));
#50047=CARTESIAN_POINT('Ctrl Pts',(-21.,5.19306705314332,-5.071830148219));
#50048=CARTESIAN_POINT('Ctrl Pts',(-21.,5.1597732798141,-5.03780325407688));
#50049=CARTESIAN_POINT('Ctrl Pts',(-21.,5.14318775290069,-5.02073460645076));
#50050=CARTESIAN_POINT('',(-21.,6.03932124977422,-3.89701874412038));
#50051=CARTESIAN_POINT('Origin',(-21.,0.,0.));
#50052=CARTESIAN_POINT('',(-21.,8.24940658621529,-4.71140010775012));
#50053=CARTESIAN_POINT('Ctrl Pts',(-21.,6.03932124977421,-3.89701874412039));
#50054=CARTESIAN_POINT('Ctrl Pts',(-21.,6.0565953297729,-3.90728293824429));
#50055=CARTESIAN_POINT('Ctrl Pts',(-21.,6.09105342163039,-3.92794852152395));
#50056=CARTESIAN_POINT('Ctrl Pts',(-21.,6.14247034880463,-3.95935849016754));
#50057=CARTESIAN_POINT('Ctrl Pts',(-21.,6.21048516503746,-4.00206265639536));
#50058=CARTESIAN_POINT('Ctrl Pts',(-21.,6.29463308326085,-4.05676946424956));
#50059=CARTESIAN_POINT('Ctrl Pts',(-21.,6.37801243240243,-4.11264895980536));
#50060=CARTESIAN_POINT('Ctrl Pts',(-21.,6.46083145580807,-4.1693867325325));
#50061=CARTESIAN_POINT('Ctrl Pts',(-21.,6.54344708143028,-4.22644426515767));
#50062=CARTESIAN_POINT('Ctrl Pts',(-21.,6.62638951409907,-4.28302021638686));
#50063=CARTESIAN_POINT('Ctrl Pts',(-21.,6.71027219290963,-4.33817259947066));
#50064=CARTESIAN_POINT('Ctrl Pts',(-21.,6.79571235355295,-4.39092540044368));
#50065=CARTESIAN_POINT('Ctrl Pts',(-21.,6.88325224876452,-4.44037556328962));
#50066=CARTESIAN_POINT('Ctrl Pts',(-21.,6.9732685530375,-4.48581308997575));
#50067=CARTESIAN_POINT('Ctrl Pts',(-21.,7.06592138953324,-4.5267956450212));
#50068=CARTESIAN_POINT('Ctrl Pts',(-21.,7.16121001331941,-4.56309881747208));
#50069=CARTESIAN_POINT('Ctrl Pts',(-21.,7.25900770064673,-4.59469206087561));
#50070=CARTESIAN_POINT('Ctrl Pts',(-21.,7.35910284385827,-4.62170482170181));
#50071=CARTESIAN_POINT('Ctrl Pts',(-21.,7.46123890856565,-4.64440143603747));
#50072=CARTESIAN_POINT('Ctrl Pts',(-21.,7.56514580946327,-4.66314297047291));
#50073=CARTESIAN_POINT('Ctrl Pts',(-21.,7.6705550660185,-4.67833376211481));
#50074=CARTESIAN_POINT('Ctrl Pts',(-21.,7.77721964274024,-4.69037000103626));
#50075=CARTESIAN_POINT('Ctrl Pts',(-21.,7.8849298684541,-4.69959254734285));
#50076=CARTESIAN_POINT('Ctrl Pts',(-21.,7.99353571494822,-4.70622700687469));
#50077=CARTESIAN_POINT('Ctrl Pts',(-21.,8.08820523826852,-4.70981110890123));
#50078=CARTESIAN_POINT('Ctrl Pts',(-21.,8.16141264001154,-4.71119538406403));
#50079=CARTESIAN_POINT('Ctrl Pts',(-21.,8.2128114080041,-4.71148495034738));
#50080=CARTESIAN_POINT('Ctrl Pts',(-21.,8.24217907974318,-4.71142767604211));
#50081=CARTESIAN_POINT('Ctrl Pts',(-21.,8.24940658621529,-4.71140010775012));
#50082=CARTESIAN_POINT('Origin',(-21.,0.,0.));
#50083=CARTESIAN_POINT('Origin',(-65.85,0.,0.));
#50084=CARTESIAN_POINT('',(-66.,3.33,-4.07807384116069E-16));
#50085=CARTESIAN_POINT('Origin',(-66.,0.,0.));
#50086=CARTESIAN_POINT('',(-65.85,3.18,-3.89437682128858E-16));
#50087=CARTESIAN_POINT('Origin',(-66.,16.375,0.));
#50088=CARTESIAN_POINT('',(-66.,16.3612159786808,-0.671741541784789));
#50089=CARTESIAN_POINT('',(-66.,14.0217614511585,-1.06963173887292));
#50090=CARTESIAN_POINT('Ctrl Pts',(-66.,16.3612159786808,-0.671741541784789));
#50091=CARTESIAN_POINT('Ctrl Pts',(-66.,16.3519363129391,-0.675875939350101));
#50092=CARTESIAN_POINT('Ctrl Pts',(-66.,16.322986318803,-0.688711885022031));
#50093=CARTESIAN_POINT('Ctrl Pts',(-66.,16.2743241898497,-0.709958710092983));
#50094=CARTESIAN_POINT('Ctrl Pts',(-66.,16.2058743852262,-0.739044856835963));
#50095=CARTESIAN_POINT('Ctrl Pts',(-66.,16.1175336986507,-0.775065535573949));
#50096=CARTESIAN_POINT('Ctrl Pts',(-66.,16.018547775909,-0.813401076758624));
#50097=CARTESIAN_POINT('Ctrl Pts',(-66.,15.9193580975472,-0.849783012021725));
#50098=CARTESIAN_POINT('Ctrl Pts',(-66.,15.8199726227578,-0.884304144422378));
#50099=CARTESIAN_POINT('Ctrl Pts',(-66.,15.7203984586304,-0.917113393337539));
#50100=CARTESIAN_POINT('Ctrl Pts',(-66.,15.6206443917204,-0.948332278883351));
#50101=CARTESIAN_POINT('Ctrl Pts',(-66.,15.5207233107191,-0.977976807855906));
#50102=CARTESIAN_POINT('Ctrl Pts',(-66.,15.42065441025,-1.00588830882699));
#50103=CARTESIAN_POINT('Ctrl Pts',(-66.,15.3204663197849,-1.03163045186508));
#50104=CARTESIAN_POINT('Ctrl Pts',(-66.,15.2201951366894,-1.05457808085916));
#50105=CARTESIAN_POINT('Ctrl Pts',(-66.,15.1198807137451,-1.07407094658941));
#50106=CARTESIAN_POINT('Ctrl Pts',(-66.,15.0195634762927,-1.08955145679141));
#50107=CARTESIAN_POINT('Ctrl Pts',(-66.,14.9192812134642,-1.100697501046));
#50108=CARTESIAN_POINT('Ctrl Pts',(-66.,14.8190654065121,-1.10759084369408));
#50109=CARTESIAN_POINT('Ctrl Pts',(-66.,14.7189411465911,-1.11063958426619));
#50110=CARTESIAN_POINT('Ctrl Pts',(-66.,14.6189280002071,-1.11043751754959));
#50111=CARTESIAN_POINT('Ctrl Pts',(-66.,14.5190405063557,-1.10764458318629));
#50112=CARTESIAN_POINT('Ctrl Pts',(-66.,14.4192887981899,-1.10286394535002));
#50113=CARTESIAN_POINT('Ctrl Pts',(-66.,14.3196790995356,-1.09650878711472));
#50114=CARTESIAN_POINT('Ctrl Pts',(-66.,14.2202146396052,-1.08882773106131));
#50115=CARTESIAN_POINT('Ctrl Pts',(-66.,14.1407601934611,-1.08172501415579));
#50116=CARTESIAN_POINT('Ctrl Pts',(-66.,14.0812352370361,-1.07587965991017));
#50117=CARTESIAN_POINT('Ctrl Pts',(-66.,14.0415811730659,-1.0717527195609));
#50118=CARTESIAN_POINT('Ctrl Pts',(-66.,14.0217614511585,-1.06963173887291));
#50119=CARTESIAN_POINT('',(-66.,13.847248627403,-2.45104298226008));
#50120=CARTESIAN_POINT('Origin',(-66.,0.,0.));
#50121=CARTESIAN_POINT('',(-66.,16.017075735697,-3.40498309495744));
#50122=CARTESIAN_POINT('Ctrl Pts',(-66.,13.847248627403,-2.45104298226008));
#50123=CARTESIAN_POINT('Ctrl Pts',(-66.,13.8704109184829,-2.45416751351779));
#50124=CARTESIAN_POINT('Ctrl Pts',(-66.,13.9167144589915,-2.46064068498796));
#50125=CARTESIAN_POINT('Ctrl Pts',(-66.,13.9861066530346,-2.47102275853729));
#50126=CARTESIAN_POINT('Ctrl Pts',(-66.,14.0785031060049,-2.48621203480011));
#50127=CARTESIAN_POINT('Ctrl Pts',(-66.,14.1937640331043,-2.50749463728168));
#50128=CARTESIAN_POINT('Ctrl Pts',(-66.,14.3087190397278,-2.53121250086624));
#50129=CARTESIAN_POINT('Ctrl Pts',(-66.,14.423228955274,-2.55762788131115));
#50130=CARTESIAN_POINT('Ctrl Pts',(-66.,14.537056384215,-2.58717382256056));
#50131=CARTESIAN_POINT('Ctrl Pts',(-66.,14.6499173448672,-2.62041096375855));
#50132=CARTESIAN_POINT('Ctrl Pts',(-66.,14.7615516365331,-2.65797355871958));
#50133=CARTESIAN_POINT('Ctrl Pts',(-66.,14.8717795409674,-2.70050907188802));
#50134=CARTESIAN_POINT('Ctrl Pts',(-66.,14.9805825983482,-2.74864579544975));
#50135=CARTESIAN_POINT('Ctrl Pts',(-66.,15.0880810351184,-2.80279667637514));
#50136=CARTESIAN_POINT('Ctrl Pts',(-66.,15.1944599098748,-2.86283428974206));
#50137=CARTESIAN_POINT('Ctrl Pts',(-66.,15.299916309402,-2.9278833773088));
#50138=CARTESIAN_POINT('Ctrl Pts',(-66.,15.4045879562307,-2.99587287520288));
#50139=CARTESIAN_POINT('Ctrl Pts',(-66.,15.5085273245779,-3.06389197726713));
#50140=CARTESIAN_POINT('Ctrl Pts',(-66.,15.6117260024113,-3.1296030647124));
#50141=CARTESIAN_POINT('Ctrl Pts',(-66.,15.7141266693079,-3.19226978910788));
#50142=CARTESIAN_POINT('Ctrl Pts',(-66.,15.8156387361042,-3.25420659877988));
#50143=CARTESIAN_POINT('Ctrl Pts',(-66.,15.8964112622344,-3.30811417274226));
#50144=CARTESIAN_POINT('Ctrl Pts',(-66.,15.9565872333324,-3.35376990021665));
#50145=CARTESIAN_POINT('Ctrl Pts',(-66.,15.9965977364772,-3.38711758925191));
#50146=CARTESIAN_POINT('Ctrl Pts',(-66.,16.0167227315819,-3.40467488782123));
#50147=CARTESIAN_POINT('Ctrl Pts',(-66.,16.017075735697,-3.40498309495744));
#50148=CARTESIAN_POINT('',(-66.,15.6801429643085,-4.71950650162129));
#50149=CARTESIAN_POINT('Origin',(-66.,0.,0.));
#50150=CARTESIAN_POINT('',(-66.,13.3152354345065,-4.52309756402218));
#50151=CARTESIAN_POINT('Ctrl Pts',(-66.,15.6801429643085,-4.71950650162129));
#50152=CARTESIAN_POINT('Ctrl Pts',(-66.,15.6701266534662,-4.72120325045824));
#50153=CARTESIAN_POINT('Ctrl Pts',(-66.,15.6388940067504,-4.72643636051809));
#50154=CARTESIAN_POINT('Ctrl Pts',(-66.,15.586476817532,-4.73491389815065));
#50155=CARTESIAN_POINT('Ctrl Pts',(-66.,15.5129440588396,-4.74606347591976));
#50156=CARTESIAN_POINT('Ctrl Pts',(-66.,15.418420778849,-4.75898306342126));
#50157=CARTESIAN_POINT('Ctrl Pts',(-66.,15.3130110194811,-4.77149742512795));
#50158=CARTESIAN_POINT('Ctrl Pts',(-66.,15.2078897478867,-4.78206888507335));
#50159=CARTESIAN_POINT('Ctrl Pts',(-66.,15.1030415940234,-4.79078931010852));
#50160=CARTESIAN_POINT('Ctrl Pts',(-66.,14.9984364069554,-4.79780470849564));
#50161=CARTESIAN_POINT('Ctrl Pts',(-66.,14.8940524763685,-4.80323496770043));
#50162=CARTESIAN_POINT('Ctrl Pts',(-66.,14.7898983053036,-4.80709879692323));
#50163=CARTESIAN_POINT('Ctrl Pts',(-66.,14.6860319453295,-4.80924728319928));
#50164=CARTESIAN_POINT('Ctrl Pts',(-66.,14.5825896373118,-4.80926492456431));
#50165=CARTESIAN_POINT('Ctrl Pts',(-66.,14.4797618145538,-4.80655518238588));
#50166=CARTESIAN_POINT('Ctrl Pts',(-66.,14.3777512750926,-4.80048846137132));
#50167=CARTESIAN_POINT('Ctrl Pts',(-66.,14.27673584179,-4.79053474041595));
#50168=CARTESIAN_POINT('Ctrl Pts',(-66.,14.1768322221664,-4.77639142656668));
#50169=CARTESIAN_POINT('Ctrl Pts',(-66.,14.0780505744683,-4.75814554445644));
#50170=CARTESIAN_POINT('Ctrl Pts',(-66.,13.9803137113395,-4.73619861233502));
#50171=CARTESIAN_POINT('Ctrl Pts',(-66.,13.8834929138094,-4.71113063582666));
#50172=CARTESIAN_POINT('Ctrl Pts',(-66.,13.7874381437893,-4.68358443705714));
#50173=CARTESIAN_POINT('Ctrl Pts',(-66.,13.6920092152502,-4.65414675070122));
#50174=CARTESIAN_POINT('Ctrl Pts',(-66.,13.5971094020329,-4.62321932672933));
#50175=CARTESIAN_POINT('Ctrl Pts',(-66.,13.5026800019769,-4.59104377985933));
#50176=CARTESIAN_POINT('Ctrl Pts',(-66.,13.4274881372306,-4.56440469062003));
#50177=CARTESIAN_POINT('Ctrl Pts',(-66.,13.3712869472582,-4.54393972423008));
#50178=CARTESIAN_POINT('Ctrl Pts',(-66.,13.3339050169562,-4.53008087460641));
#50179=CARTESIAN_POINT('Ctrl Pts',(-66.,13.3152354345065,-4.52309756402217));
#50180=CARTESIAN_POINT('',(-66.,12.8026622457696,-5.81770965851216));
#50181=CARTESIAN_POINT('Origin',(-66.,0.,0.));
#50182=CARTESIAN_POINT('',(-66.,14.6670849864349,-7.28129404712486));
#50183=CARTESIAN_POINT('Ctrl Pts',(-66.,12.8026622457696,-5.81770965851216));
#50184=CARTESIAN_POINT('Ctrl Pts',(-66.,12.8243198115569,-5.82649625442995));
#50185=CARTESIAN_POINT('Ctrl Pts',(-66.,12.8675588289116,-5.84428128157946));
#50186=CARTESIAN_POINT('Ctrl Pts',(-66.,12.932189022876,-5.87159432010365));
#50187=CARTESIAN_POINT('Ctrl Pts',(-66.,13.0179052519711,-5.90928446078516));
#50188=CARTESIAN_POINT('Ctrl Pts',(-66.,13.124252277086,-5.95856265812867));
#50189=CARTESIAN_POINT('Ctrl Pts',(-66.,13.2296973679703,-6.01012352904084));
#50190=CARTESIAN_POINT('Ctrl Pts',(-66.,13.3340405059683,-6.06418647971103));
#50191=CARTESIAN_POINT('Ctrl Pts',(-66.,13.4369440601197,-6.12111191134452));
#50192=CARTESIAN_POINT('Ctrl Pts',(-66.,13.537993545262,-6.18137222620287));
#50193=CARTESIAN_POINT('Ctrl Pts',(-66.,13.6367792028716,-6.24551704256852));
#50194=CARTESIAN_POINT('Ctrl Pts',(-66.,13.7329659430228,-6.31412878948963));
#50195=CARTESIAN_POINT('Ctrl Pts',(-66.,13.8263796359301,-6.38781142942664));
#50196=CARTESIAN_POINT('Ctrl Pts',(-66.,13.9170340351662,-6.46699483496205));
#50197=CARTESIAN_POINT('Ctrl Pts',(-66.,14.0051400746611,-6.55160160666348));
#50198=CARTESIAN_POINT('Ctrl Pts',(-66.,14.0911063172293,-6.64083299762664));
#50199=CARTESIAN_POINT('Ctrl Pts',(-66.,14.1755812112355,-6.73271726045961));
#50200=CARTESIAN_POINT('Ctrl Pts',(-66.,14.2593394703776,-6.8244480871404));
#50201=CARTESIAN_POINT('Ctrl Pts',(-66.,14.3429542890555,-6.9137592074853));
#50202=CARTESIAN_POINT('Ctrl Pts',(-66.,14.426553270081,-6.99992315179396));
#50203=CARTESIAN_POINT('Ctrl Pts',(-66.,14.5094730904225,-7.08515912713373));
#50204=CARTESIAN_POINT('Ctrl Pts',(-66.,14.5743017306281,-7.15746040594034));
#50205=CARTESIAN_POINT('Ctrl Pts',(-66.,14.6212330452241,-7.21664693024351));
#50206=CARTESIAN_POINT('Ctrl Pts',(-66.,14.6516933118151,-7.2588971478181));
#50207=CARTESIAN_POINT('Ctrl Pts',(-66.,14.6668197205911,-7.28090773432903));
#50208=CARTESIAN_POINT('Ctrl Pts',(-66.,14.6670849864349,-7.28129404712486));
#50209=CARTESIAN_POINT('',(-66.,14.0138288999568,-8.47072751083015));
#50210=CARTESIAN_POINT('Origin',(-66.,0.,0.));
#50211=CARTESIAN_POINT('',(-66.,11.7720642054939,-7.6923605344347));
#50212=CARTESIAN_POINT('Ctrl Pts',(-66.,14.0138288999568,-8.47072751083015));
#50213=CARTESIAN_POINT('Ctrl Pts',(-66.,14.0037053056615,-8.4698799979691));
#50214=CARTESIAN_POINT('Ctrl Pts',(-66.,13.9721524684248,-8.46718145686578));
#50215=CARTESIAN_POINT('Ctrl Pts',(-66.,13.9192737837169,-8.4623570321923));
#50216=CARTESIAN_POINT('Ctrl Pts',(-66.,13.8452784046188,-8.45486947201102));
#50217=CARTESIAN_POINT('Ctrl Pts',(-66.,13.7505117765273,-8.44387618307839));
#50218=CARTESIAN_POINT('Ctrl Pts',(-66.,13.6453014633841,-8.42978304193647));
#50219=CARTESIAN_POINT('Ctrl Pts',(-66.,13.5408537546603,-8.41387978285669));
#50220=CARTESIAN_POINT('Ctrl Pts',(-66.,13.4371309168349,-8.39625156414993));
#50221=CARTESIAN_POINT('Ctrl Pts',(-66.,13.3340674354409,-8.37703230872753));
#50222=CARTESIAN_POINT('Ctrl Pts',(-66.,13.231612467433,-8.35633273843435));
#50223=CARTESIAN_POINT('Ctrl Pts',(-66.,13.1297695959248,-8.33417308930716));
#50224=CARTESIAN_POINT('Ctrl Pts',(-66.,13.0286320818366,-8.31042356359388));
#50225=CARTESIAN_POINT('Ctrl Pts',(-66.,12.9284352169133,-8.284715594814));
#50226=CARTESIAN_POINT('Ctrl Pts',(-66.,12.829511804771,-8.25651874452987));
#50227=CARTESIAN_POINT('Ctrl Pts',(-66.,12.7322148461558,-8.22527363116368));
#50228=CARTESIAN_POINT('Ctrl Pts',(-66.,12.636848388186,-8.19051110794578));
#50229=CARTESIAN_POINT('Ctrl Pts',(-66.,12.5436007236081,-8.15196711241727));
#50230=CARTESIAN_POINT('Ctrl Pts',(-66.,12.4524600493824,-8.10972846142537));
#50231=CARTESIAN_POINT('Ctrl Pts',(-66.,12.3632517496072,-8.06416486307078));
#50232=CARTESIAN_POINT('Ctrl Pts',(-66.,12.2757069077219,-8.01580608992824));
#50233=CARTESIAN_POINT('Ctrl Pts',(-66.,12.1895203359981,-7.96523745572904));
#50234=CARTESIAN_POINT('Ctrl Pts',(-66.,12.1044103376288,-7.91299239895144));
#50235=CARTESIAN_POINT('Ctrl Pts',(-66.,12.0201833141302,-7.85943599303422));
#50236=CARTESIAN_POINT('Ctrl Pts',(-66.,11.936722320441,-7.80478766329085));
#50237=CARTESIAN_POINT('Ctrl Pts',(-66.,11.870517618491,-7.7602860336664));
#50238=CARTESIAN_POINT('Ctrl Pts',(-66.,11.8211715224307,-7.72648734423527));
#50239=CARTESIAN_POINT('Ctrl Pts',(-66.,11.7884105699588,-7.70376738782835));
#50240=CARTESIAN_POINT('Ctrl Pts',(-66.,11.7720642054939,-7.69236053443469));
#50241=CARTESIAN_POINT('',(-66.,10.9536375103364,-8.81882824088046));
#50242=CARTESIAN_POINT('Origin',(-66.,0.,0.));
#50243=CARTESIAN_POINT('',(-66.,12.3955073457098,-10.7000945155851));
#50244=CARTESIAN_POINT('Ctrl Pts',(-66.,10.9536375103364,-8.81882824088046));
#50245=CARTESIAN_POINT('Ctrl Pts',(-66.,10.9724295263217,-8.83272480732197));
#50246=CARTESIAN_POINT('Ctrl Pts',(-66.,11.0098871540402,-8.86070419148627));
#50247=CARTESIAN_POINT('Ctrl Pts',(-66.,11.0656943951459,-8.90323201632451));
#50248=CARTESIAN_POINT('Ctrl Pts',(-66.,11.1393445344495,-8.96105481127105));
#50249=CARTESIAN_POINT('Ctrl Pts',(-66.,11.2300954828748,-9.03523227310488));
#50250=CARTESIAN_POINT('Ctrl Pts',(-66.,11.3194051551598,-9.11139639219764));
#50251=CARTESIAN_POINT('Ctrl Pts',(-66.,11.407025252502,-9.18970993907287));
#50252=CARTESIAN_POINT('Ctrl Pts',(-66.,11.4925391231036,-9.27043802686381));
#50253=CARTESIAN_POINT('Ctrl Pts',(-66.,11.5754278219505,-9.35393513817802));
#50254=CARTESIAN_POINT('Ctrl Pts',(-66.,11.655157779328,-9.44063172122792));
#50255=CARTESIAN_POINT('Ctrl Pts',(-66.,11.7312595885623,-9.53100857350628));
#50256=CARTESIAN_POINT('Ctrl Pts',(-66.,11.8034143911192,-9.62560737856555));
#50257=CARTESIAN_POINT('Ctrl Pts',(-66.,11.8715286035136,-9.724847924125));
#50258=CARTESIAN_POINT('Ctrl Pts',(-66.,11.9358257812543,-9.82870769953299));
#50259=CARTESIAN_POINT('Ctrl Pts',(-66.,11.9969002916812,-9.93651465742827));
#50260=CARTESIAN_POINT('Ctrl Pts',(-66.,12.0558705645975,-10.0465202590396));
#50261=CARTESIAN_POINT('Ctrl Pts',(-66.,12.1141848750712,-10.1561990251342));
#50262=CARTESIAN_POINT('Ctrl Pts',(-66.,12.1729620080223,-10.2634984322242));
#50263=CARTESIAN_POINT('Ctrl Pts',(-66.,12.2325064717433,-10.3677455989363));
#50264=CARTESIAN_POINT('Ctrl Pts',(-66.,12.2916238883603,-10.4709250501372));
#50265=CARTESIAN_POINT('Ctrl Pts',(-66.,12.336435220754,-10.5570770785351));
#50266=CARTESIAN_POINT('Ctrl Pts',(-66.,12.3671730117507,-10.6260754926723));
#50267=CARTESIAN_POINT('Ctrl Pts',(-66.,12.3861691112129,-10.6745735022306));
#50268=CARTESIAN_POINT('Ctrl Pts',(-66.,12.3953464857659,-10.6996543705834));
#50269=CARTESIAN_POINT('Ctrl Pts',(-66.,12.3955073457098,-10.7000945155851));
#50270=CARTESIAN_POINT('',(-66.,11.4669744265634,-11.689701557377));
#50271=CARTESIAN_POINT('Origin',(-66.,0.,0.));
#50272=CARTESIAN_POINT('',(-66.,9.48921088782657,-10.3782842019456));
#50273=CARTESIAN_POINT('Ctrl Pts',(-66.,11.4669744265634,-11.689701557377));
#50274=CARTESIAN_POINT('Ctrl Pts',(-66.,11.4573796514766,-11.6863630351679));
#50275=CARTESIAN_POINT('Ctrl Pts',(-66.,11.4274892045258,-11.6759024021635));
#50276=CARTESIAN_POINT('Ctrl Pts',(-66.,11.3774715865628,-11.6580791515292));
#50277=CARTESIAN_POINT('Ctrl Pts',(-66.,11.3076629888636,-11.632424924341));
#50278=CARTESIAN_POINT('Ctrl Pts',(-66.,11.2186075484415,-11.5982095077484));
#50279=CARTESIAN_POINT('Ctrl Pts',(-66.,11.1202074324343,-11.5583943876468));
#50280=CARTESIAN_POINT('Ctrl Pts',(-66.,11.0229961202521,-11.5170156697979));
#50281=CARTESIAN_POINT('Ctrl Pts',(-66.,10.926915885831,-11.4741464531626));
#50282=CARTESIAN_POINT('Ctrl Pts',(-66.,10.8318699676878,-11.4299001604323));
#50283=CARTESIAN_POINT('Ctrl Pts',(-66.,10.737781584702,-11.3843713907704));
#50284=CARTESIAN_POINT('Ctrl Pts',(-66.,10.6446491749193,-11.3375806355454));
#50285=CARTESIAN_POINT('Ctrl Pts',(-66.,10.5525953486849,-11.289425367888));
#50286=CARTESIAN_POINT('Ctrl Pts',(-66.,10.4619396643774,-11.2396071151889));
#50287=CARTESIAN_POINT('Ctrl Pts',(-66.,10.3731363846505,-11.1876948686032));
#50288=CARTESIAN_POINT('Ctrl Pts',(-66.,10.2866665326243,-11.1332346082697));
#50289=CARTESIAN_POINT('Ctrl Pts',(-66.,10.2029412752749,-11.0758475399707));
#50290=CARTESIAN_POINT('Ctrl Pts',(-66.,10.1222086594491,-11.0153247237569));
#50291=CARTESIAN_POINT('Ctrl Pts',(-66.,10.0444356624493,-10.951747313668));
#50292=CARTESIAN_POINT('Ctrl Pts',(-66.,9.9693612115878,-10.885429977536));
#50293=CARTESIAN_POINT('Ctrl Pts',(-66.,9.89659308973021,-10.816818967327));
#50294=CARTESIAN_POINT('Ctrl Pts',(-66.,9.82569013557624,-10.7464053109633));
#50295=CARTESIAN_POINT('Ctrl Pts',(-66.,9.75624684158698,-10.6746356328252));
#50296=CARTESIAN_POINT('Ctrl Pts',(-66.,9.68798490145875,-10.6018153909131));
#50297=CARTESIAN_POINT('Ctrl Pts',(-66.,9.62073647531797,-10.5281280338367));
#50298=CARTESIAN_POINT('Ctrl Pts',(-66.,9.56767882107163,-10.4685600648819));
#50299=CARTESIAN_POINT('Ctrl Pts',(-66.,9.52828841562115,-10.4235513483695));
#50300=CARTESIAN_POINT('Ctrl Pts',(-66.,9.50220693210954,-10.3933978635985));
#50301=CARTESIAN_POINT('Ctrl Pts',(-66.,9.48921088782658,-10.3782842019456));
#50302=CARTESIAN_POINT('',(-66.,8.41635544546801,-11.2658274114927));
#50303=CARTESIAN_POINT('Origin',(-66.,0.,0.));
#50304=CARTESIAN_POINT('',(-66.,9.34507439096662,-13.4465686934362));
#50305=CARTESIAN_POINT('Ctrl Pts',(-66.,8.41635544546801,-11.2658274114927));
#50306=CARTESIAN_POINT('Ctrl Pts',(-66.,8.43110114017464,-11.2839607760805));
#50307=CARTESIAN_POINT('Ctrl Pts',(-66.,8.46042377774785,-11.3203764696515));
#50308=CARTESIAN_POINT('Ctrl Pts',(-66.,8.50390149179148,-11.3754469011628));
#50309=CARTESIAN_POINT('Ctrl Pts',(-66.,8.56085783218497,-11.4497691315105));
#50310=CARTESIAN_POINT('Ctrl Pts',(-66.,8.63031048807256,-11.544185015102));
#50311=CARTESIAN_POINT('Ctrl Pts',(-66.,8.69787308659046,-11.6401667106607));
#50312=CARTESIAN_POINT('Ctrl Pts',(-66.,8.76326465031677,-11.7378101255738));
#50313=CARTESIAN_POINT('Ctrl Pts',(-66.,8.8260156863806,-11.8372684268691));
#50314=CARTESIAN_POINT('Ctrl Pts',(-66.,8.88553539714026,-11.9387559040544));
#50315=CARTESIAN_POINT('Ctrl Pts',(-66.,8.94119992783734,-12.0425567886278));
#50316=CARTESIAN_POINT('Ctrl Pts',(-66.,8.99243504959771,-12.149020036252));
#50317=CARTESIAN_POINT('Ctrl Pts',(-66.,9.03879721019277,-12.2585910156016));
#50318=CARTESIAN_POINT('Ctrl Pts',(-66.,9.08009136927418,-12.3716530527263));
#50319=CARTESIAN_POINT('Ctrl Pts',(-66.,9.11653965711474,-12.4882399401825));
#50320=CARTESIAN_POINT('Ctrl Pts',(-66.,9.14888489929381,-12.6078485573591));
#50321=CARTESIAN_POINT('Ctrl Pts',(-66.,9.17864523199547,-12.7290634412273));
#50322=CARTESIAN_POINT('Ctrl Pts',(-66.,9.20785149120868,-12.8497986264917));
#50323=CARTESIAN_POINT('Ctrl Pts',(-66.,9.23809775500251,-12.9683443039596));
#50324=CARTESIAN_POINT('Ctrl Pts',(-66.,9.26984630377419,-13.0841244601964));
#50325=CARTESIAN_POINT('Ctrl Pts',(-66.,9.30144675196197,-13.1987642428721));
#50326=CARTESIAN_POINT('Ctrl Pts',(-66.,9.32342511572492,-13.293353772072));
#50327=CARTESIAN_POINT('Ctrl Pts',(-66.,9.33603801466832,-13.3678286519246));
#50328=CARTESIAN_POINT('Ctrl Pts',(-66.,9.3423763522097,-13.4195271451628));
#50329=CARTESIAN_POINT('Ctrl Pts',(-66.,9.34502804434446,-13.4461023721578));
#50330=CARTESIAN_POINT('Ctrl Pts',(-66.,9.34507439096662,-13.4465686934362));
#50331=CARTESIAN_POINT('',(-66.,8.199607777367,-14.1741686633588));
#50332=CARTESIAN_POINT('Origin',(-66.,0.,0.));
#50333=CARTESIAN_POINT('',(-66.,6.61011555120063,-12.4121021043889));
#50334=CARTESIAN_POINT('Ctrl Pts',(-66.,8.199607777367,-14.1741686633588));
#50335=CARTESIAN_POINT('Ctrl Pts',(-66.,8.19114469649464,-14.1685489034304));
#50336=CARTESIAN_POINT('Ctrl Pts',(-66.,8.16479476654098,-14.150983458568));
#50337=CARTESIAN_POINT('Ctrl Pts',(-66.,8.1207810062114,-14.1212812823596));
#50338=CARTESIAN_POINT('Ctrl Pts',(-66.,8.05954552084273,-14.0790723376084));
#50339=CARTESIAN_POINT('Ctrl Pts',(-66.,7.98179694893469,-14.0237846738158));
#50340=CARTESIAN_POINT('Ctrl Pts',(-66.,7.89638987124254,-13.9607493051802));
#50341=CARTESIAN_POINT('Ctrl Pts',(-66.,7.81252309986449,-13.8964951055849));
#50342=CARTESIAN_POINT('Ctrl Pts',(-66.,7.7301225433348,-13.8310785215643));
#50343=CARTESIAN_POINT('Ctrl Pts',(-66.,7.6490662730339,-13.7645853488249));
#50344=CARTESIAN_POINT('Ctrl Pts',(-66.,7.56925639420599,-13.6970881198352));
#50345=CARTESIAN_POINT('Ctrl Pts',(-66.,7.49068629797234,-13.6286062937474));
#50346=CARTESIAN_POINT('Ctrl Pts',(-66.,7.41350024004436,-13.5590710567155));
#50347=CARTESIAN_POINT('Ctrl Pts',(-66.,7.33808196640605,-13.4882727841331));
#50348=CARTESIAN_POINT('Ctrl Pts',(-66.,7.26497865575545,-13.4159069786186));
#50349=CARTESIAN_POINT('Ctrl Pts',(-66.,7.19476912913493,-13.3416535097654));
#50350=CARTESIAN_POINT('Ctrl Pts',(-66.,7.12794583824513,-13.2652477369413));
#50351=CARTESIAN_POINT('Ctrl Pts',(-66.,7.06480099833745,-13.1865489711723));
#50352=CARTESIAN_POINT('Ctrl Pts',(-66.,7.00528244199424,-13.1056276044837));
#50353=CARTESIAN_POINT('Ctrl Pts',(-66.,6.94905904389849,-13.0227234927017));
#50354=CARTESIAN_POINT('Ctrl Pts',(-66.,6.89563993078743,-12.9381713275312));
#50355=CARTESIAN_POINT('Ctrl Pts',(-66.,6.84447568757558,-12.8523369979956));
#50356=CARTESIAN_POINT('Ctrl Pts',(-66.,6.79506247552229,-12.7655522513249));
#50357=CARTESIAN_POINT('Ctrl Pts',(-66.,6.74705476751256,-12.6780437370314));
#50358=CARTESIAN_POINT('Ctrl Pts',(-66.,6.70024437485702,-12.5899474002701));
#50359=CARTESIAN_POINT('Ctrl Pts',(-66.,6.66366757586302,-12.5190559665502));
#50360=CARTESIAN_POINT('Ctrl Pts',(-66.,6.63670790506457,-12.4656652861453));
#50361=CARTESIAN_POINT('Ctrl Pts',(-66.,6.6189446860433,-12.4299729273552));
#50362=CARTESIAN_POINT('Ctrl Pts',(-66.,6.61011555120064,-12.4121021043889));
#50363=CARTESIAN_POINT('',(-66.,5.35024281477071,-13.004953213026));
#50364=CARTESIAN_POINT('Origin',(-66.,0.,0.));
#50365=CARTESIAN_POINT('',(-66.,5.70745604345953,-15.3481455072584));
#50366=CARTESIAN_POINT('Ctrl Pts',(-66.,5.35024281477071,-13.004953213026));
#50367=CARTESIAN_POINT('Ctrl Pts',(-66.,5.36001566196946,-13.026183989773));
#50368=CARTESIAN_POINT('Ctrl Pts',(-66.,5.37936086023753,-13.0687478607962));
#50369=CARTESIAN_POINT('Ctrl Pts',(-66.,5.40777718254589,-13.1329006212338));
#50370=CARTESIAN_POINT('Ctrl Pts',(-66.,5.44446094769152,-13.2190523479119));
#50371=CARTESIAN_POINT('Ctrl Pts',(-66.,5.48825134524296,-13.3277741560577));
#50372=CARTESIAN_POINT('Ctrl Pts',(-66.,5.52982166345111,-13.4375425451545));
#50373=CARTESIAN_POINT('Ctrl Pts',(-66.,5.56887590111916,-13.548380533239));
#50374=CARTESIAN_POINT('Ctrl Pts',(-66.,5.60492122426722,-13.6603197171863));
#50375=CARTESIAN_POINT('Ctrl Pts',(-66.,5.63733210461441,-13.7734207288063));
#50376=CARTESIAN_POINT('Ctrl Pts',(-66.,5.66543360144756,-13.8878037235725));
#50377=CARTESIAN_POINT('Ctrl Pts',(-66.,5.68858274460417,-14.0036638891498));
#50378=CARTESIAN_POINT('Ctrl Pts',(-66.,5.7062391581791,-14.1213222951832));
#50379=CARTESIAN_POINT('Ctrl Pts',(-66.,5.71811860006313,-14.2411017202677));
#50380=CARTESIAN_POINT('Ctrl Pts',(-66.,5.7244278180311,-14.3630901368566));
#50381=CARTESIAN_POINT('Ctrl Pts',(-66.,5.72601142143879,-14.4869849640075));
#50382=CARTESIAN_POINT('Ctrl Pts',(-66.,5.72469186277131,-14.611792753182));
#50383=CARTESIAN_POINT('Ctrl Pts',(-66.,5.72295493404455,-14.7359981218931));
#50384=CARTESIAN_POINT('Ctrl Pts',(-66.,5.72276984468895,-14.8583414088431));
#50385=CARTESIAN_POINT('Ctrl Pts',(-66.,5.72472760042901,-14.9783796615786));
#50386=CARTESIAN_POINT('Ctrl Pts',(-66.,5.72682550780959,-15.0972765365679));
#50387=CARTESIAN_POINT('Ctrl Pts',(-66.,5.72458992151581,-15.1943601585744));
#50388=CARTESIAN_POINT('Ctrl Pts',(-66.,5.71828541357827,-15.2696319735416));
#50389=CARTESIAN_POINT('Ctrl Pts',(-66.,5.7115677281404,-15.3212825439959));
#50390=CARTESIAN_POINT('Ctrl Pts',(-66.,5.70752712228784,-15.3476823103842));
#50391=CARTESIAN_POINT('Ctrl Pts',(-66.,5.70745604345953,-15.3481455072584));
#50392=CARTESIAN_POINT('',(-66.,4.41702961547073,-15.7680206232759));
#50393=CARTESIAN_POINT('Origin',(-66.,0.,0.));
#50394=CARTESIAN_POINT('',(-66.,3.31568234418831,-13.6660219830951));
#50395=CARTESIAN_POINT('Ctrl Pts',(-66.,4.41702961547073,-15.7680206232759));
#50396=CARTESIAN_POINT('Ctrl Pts',(-66.,4.41022999530899,-15.7604727358124));
#50397=CARTESIAN_POINT('Ctrl Pts',(-66.,4.38907624535977,-15.7369061805941));
#50398=CARTESIAN_POINT('Ctrl Pts',(-66.,4.35383188909641,-15.6971913757796));
#50399=CARTESIAN_POINT('Ctrl Pts',(-66.,4.30501716681229,-15.6410798566978));
#50400=CARTESIAN_POINT('Ctrl Pts',(-66.,4.24346069213056,-15.5681938729551));
#50401=CARTESIAN_POINT('Ctrl Pts',(-66.,4.17641309355012,-15.4858989998248));
#50402=CARTESIAN_POINT('Ctrl Pts',(-66.,4.11116052066234,-15.4028066461541));
#50403=CARTESIAN_POINT('Ctrl Pts',(-66.,4.04761717203886,-15.3189530593075));
#50404=CARTESIAN_POINT('Ctrl Pts',(-66.,3.98564361314731,-15.2343910171469));
#50405=CARTESIAN_POINT('Ctrl Pts',(-66.,3.92512698668427,-15.1491664279643));
#50406=CARTESIAN_POINT('Ctrl Pts',(-66.,3.8660560521067,-15.0632964960055));
#50407=CARTESIAN_POINT('Ctrl Pts',(-66.,3.80858764637521,-14.9767504442745));
#50408=CARTESIAN_POINT('Ctrl Pts',(-66.,3.75314559090774,-14.8894206676529));
#50409=CARTESIAN_POINT('Ctrl Pts',(-66.,3.7003355991968,-14.801148312913));
#50410=CARTESIAN_POINT('Ctrl Pts',(-66.,3.65079792075207,-14.7117672540732));
#50411=CARTESIAN_POINT('Ctrl Pts',(-66.,3.60507534944737,-14.6211436324314));
#50412=CARTESIAN_POINT('Ctrl Pts',(-66.,3.56348590797974,-14.5292138499942));
#50413=CARTESIAN_POINT('Ctrl Pts',(-66.,3.52596156208203,-14.436033113783));
#50414=CARTESIAN_POINT('Ctrl Pts',(-66.,3.49212193962963,-14.3417513965941));
#50415=CARTESIAN_POINT('Ctrl Pts',(-66.,3.46140835460361,-14.246570799961));
#50416=CARTESIAN_POINT('Ctrl Pts',(-66.,3.43319765990381,-14.1507090838548));
#50417=CARTESIAN_POINT('Ctrl Pts',(-66.,3.40691934362888,-14.0543622734568));
#50418=CARTESIAN_POINT('Ctrl Pts',(-66.,3.38218236859189,-13.9576639685687));
#50419=CARTESIAN_POINT('Ctrl Pts',(-66.,3.35875127854871,-13.860694068957));
#50420=CARTESIAN_POINT('Ctrl Pts',(-66.,3.34095358960791,-13.7829335399729));
#50421=CARTESIAN_POINT('Ctrl Pts',(-66.,3.3281186287285,-13.7245156284827));
#50422=CARTESIAN_POINT('Ctrl Pts',(-66.,3.31978980257722,-13.6855270778435));
#50423=CARTESIAN_POINT('Ctrl Pts',(-66.,3.31568234418832,-13.6660219830951));
#50424=CARTESIAN_POINT('',(-66.,1.94795475120472,-13.9269299753125));
#50425=CARTESIAN_POINT('Origin',(-66.,0.,0.));
#50426=CARTESIAN_POINT('',(-66.,1.71121724218688,-16.2853418923289));
#50427=CARTESIAN_POINT('Ctrl Pts',(-66.,1.94795475120472,-13.9269299753125));
#50428=CARTESIAN_POINT('Ctrl Pts',(-66.,1.95214068696407,-13.9499241564345));
#50429=CARTESIAN_POINT('Ctrl Pts',(-66.,1.96029291597316,-13.9959617603545));
#50430=CARTESIAN_POINT('Ctrl Pts',(-66.,1.9718623445077,-14.0651658958429));
#50431=CARTESIAN_POINT('Ctrl Pts',(-66.,1.98596855852791,-14.1577338890203));
#50432=CARTESIAN_POINT('Ctrl Pts',(-66.,2.00134518601523,-14.2739302306637));
#50433=CARTESIAN_POINT('Ctrl Pts',(-66.,2.01431120793567,-14.3905881617116));
#50434=CARTESIAN_POINT('Ctrl Pts',(-66.,2.02457419816135,-14.5076563645426));
#50435=CARTESIAN_POINT('Ctrl Pts',(-66.,2.03164894817481,-14.625042880531));
#50436=CARTESIAN_POINT('Ctrl Pts',(-66.,2.03491450329845,-14.7426508740692));
#50437=CARTESIAN_POINT('Ctrl Pts',(-66.,2.03368724587156,-14.8604288747958));
#50438=CARTESIAN_POINT('Ctrl Pts',(-66.,2.02729586462329,-14.9784060380191));
#50439=CARTESIAN_POINT('Ctrl Pts',(-66.,2.01513711377743,-15.096758960368));
#50440=CARTESIAN_POINT('Ctrl Pts',(-66.,1.99685540944097,-15.2157295916163));
#50441=CARTESIAN_POINT('Ctrl Pts',(-66.,1.97262912616775,-15.3354545564815));
#50442=CARTESIAN_POINT('Ctrl Pts',(-66.,1.94335158717786,-15.4558508259636));
#50443=CARTESIAN_POINT('Ctrl Pts',(-66.,1.91103504986532,-15.5764093880396));
#50444=CARTESIAN_POINT('Ctrl Pts',(-66.,1.87846407081847,-15.6962806600859));
#50445=CARTESIAN_POINT('Ctrl Pts',(-66.,1.84785925815835,-15.8147342778518));
#50446=CARTESIAN_POINT('Ctrl Pts',(-66.,1.81990320787353,-15.9314881821968));
#50447=CARTESIAN_POINT('Ctrl Pts',(-66.,1.79236675521062,-16.047171421572));
#50448=CARTESIAN_POINT('Ctrl Pts',(-66.,1.76605768896888,-16.1406490153657));
#50449=CARTESIAN_POINT('Ctrl Pts',(-66.,1.74123190957046,-16.211988160483));
#50450=CARTESIAN_POINT('Ctrl Pts',(-66.,1.72188029803531,-16.2603454128541));
#50451=CARTESIAN_POINT('Ctrl Pts',(-66.,1.71140128032148,-16.284910924222));
#50452=CARTESIAN_POINT('Ctrl Pts',(-66.,1.71121724218688,-16.2853418923289));
#50453=CARTESIAN_POINT('',(-66.,0.356913238135829,-16.3711098567093));
#50454=CARTESIAN_POINT('Origin',(-66.,0.,0.));
#50455=CARTESIAN_POINT('',(-66.,-0.187087378736044,-14.0612554404903));
#50456=CARTESIAN_POINT('Ctrl Pts',(-66.,0.356913238135829,-16.3711098567093));
#50457=CARTESIAN_POINT('Ctrl Pts',(-66.,0.352204323826719,-16.3621081032393));
#50458=CARTESIAN_POINT('Ctrl Pts',(-66.,0.337575921789304,-16.3340212110009));
#50459=CARTESIAN_POINT('Ctrl Pts',(-66.,0.313315502115871,-16.2867892048278));
#50460=CARTESIAN_POINT('Ctrl Pts',(-66.,0.279988751445404,-16.220300804523));
#50461=CARTESIAN_POINT('Ctrl Pts',(-66.,0.238492193683111,-16.1343961952447));
#50462=CARTESIAN_POINT('Ctrl Pts',(-66.,0.194016921417006,-16.0380127071578));
#50463=CARTESIAN_POINT('Ctrl Pts',(-66.,0.151478606156202,-15.9413031975852));
#50464=CARTESIAN_POINT('Ctrl Pts',(-66.,0.110785127729046,-15.844281437166));
#50465=CARTESIAN_POINT('Ctrl Pts',(-66.,0.0717883068748032,-15.7469638696907));
#50466=CARTESIAN_POINT('Ctrl Pts',(-66.,0.0343674149818962,-15.6493668946876));
#50467=CARTESIAN_POINT('Ctrl Pts',(-66.,-0.00149271387238248,-15.5515043804903));
#50468=CARTESIAN_POINT('Ctrl Pts',(-66.,-0.0356325161212601,-15.4533855207845));
#50469=CARTESIAN_POINT('Ctrl Pts',(-66.,-0.0676147251712506,-15.3550114911653));
#50470=CARTESIAN_POINT('Ctrl Pts',(-66.,-0.0968131519417803,-15.2563790638913));
#50471=CARTESIAN_POINT('Ctrl Pts',(-66.,-0.122566347687195,-15.1574865557124));
#50472=CARTESIAN_POINT('Ctrl Pts',(-66.,-0.144315282095873,-15.058339300691));
#50473=CARTESIAN_POINT('Ctrl Pts',(-66.,-0.161736107560775,-14.9589547879103));
#50474=CARTESIAN_POINT('Ctrl Pts',(-66.,-0.174908450355344,-14.8593695705273));
#50475=CARTESIAN_POINT('Ctrl Pts',(-66.,-0.184238029232279,-14.7596343149665));
#50476=CARTESIAN_POINT('Ctrl Pts',(-66.,-0.190316238669402,-14.6598058338069));
#50477=CARTESIAN_POINT('Ctrl Pts',(-66.,-0.19380080315749,-14.5599400753078));
#50478=CARTESIAN_POINT('Ctrl Pts',(-66.,-0.195293060397626,-14.4600850256186));
#50479=CARTESIAN_POINT('Ctrl Pts',(-66.,-0.195204987344071,-14.3602728402636));
#50480=CARTESIAN_POINT('Ctrl Pts',(-66.,-0.193784513213942,-14.2605223532243));
#50481=CARTESIAN_POINT('Ctrl Pts',(-66.,-0.191684797850075,-14.1807787089954));
#50482=CARTESIAN_POINT('Ctrl Pts',(-66.,-0.189588581014708,-14.1210041786448));
#50483=CARTESIAN_POINT('Ctrl Pts',(-66.,-0.187959683517641,-14.0811692301831));
#50484=CARTESIAN_POINT('Ctrl Pts',(-66.,-0.187087378736032,-14.0612554404903));
#50485=CARTESIAN_POINT('',(-66.,-1.57673047345591,-13.9738265075847));
#50486=CARTESIAN_POINT('Origin',(-66.,0.,0.));
#50487=CARTESIAN_POINT('',(-66.,-2.39254363182917,-16.1992703530064));
#50488=CARTESIAN_POINT('Ctrl Pts',(-66.,-1.57673047345591,-13.9738265075847));
#50489=CARTESIAN_POINT('Ctrl Pts',(-66.,-1.57839446687451,-13.997139284115));
#50490=CARTESIAN_POINT('Ctrl Pts',(-66.,-1.58194744165485,-14.0437579089631));
#50491=CARTESIAN_POINT('Ctrl Pts',(-66.,-1.58795185663835,-14.1136650691543));
#50492=CARTESIAN_POINT('Ctrl Pts',(-66.,-1.59730953904946,-14.2068329413785));
#50493=CARTESIAN_POINT('Ctrl Pts',(-66.,-1.61131285168258,-14.3232027730338));
#50494=CARTESIAN_POINT('Ctrl Pts',(-66.,-1.6277658288928,-14.4394201991873));
#50495=CARTESIAN_POINT('Ctrl Pts',(-66.,-1.64693894753001,-14.5553627910342));
#50496=CARTESIAN_POINT('Ctrl Pts',(-66.,-1.6692793032136,-14.6708208125467));
#50497=CARTESIAN_POINT('Ctrl Pts',(-66.,-1.69536426015181,-14.7855460452371));
#50498=CARTESIAN_POINT('Ctrl Pts',(-66.,-1.72584315874106,-14.8993186269813));
#50499=CARTESIAN_POINT('Ctrl Pts',(-66.,-1.76137347040452,-15.0119998487957));
#50500=CARTESIAN_POINT('Ctrl Pts',(-66.,-1.80258340663877,-15.1236107380773));
#50501=CARTESIAN_POINT('Ctrl Pts',(-66.,-1.84987755047685,-15.2342972131845));
#50502=CARTESIAN_POINT('Ctrl Pts',(-66.,-1.90311710851519,-15.3442359664661));
#50503=CARTESIAN_POINT('Ctrl Pts',(-66.,-1.96141617445265,-15.4535687378813));
#50504=CARTESIAN_POINT('Ctrl Pts',(-66.,-2.02269912351901,-15.5623029350202));
#50505=CARTESIAN_POINT('Ctrl Pts',(-66.,-2.08405759848474,-15.6703081575233));
#50506=CARTESIAN_POINT('Ctrl Pts',(-66.,-2.14315912151332,-15.777429229659));
#50507=CARTESIAN_POINT('Ctrl Pts',(-66.,-2.19927239636847,-15.8835627084126));
#50508=CARTESIAN_POINT('Ctrl Pts',(-66.,-2.25471299248206,-15.9887635087906));
#50509=CARTESIAN_POINT('Ctrl Pts',(-66.,-2.30344244328183,-16.0727615333669));
#50510=CARTESIAN_POINT('Ctrl Pts',(-66.,-2.34522959911868,-16.1356855077795));
#50511=CARTESIAN_POINT('Ctrl Pts',(-66.,-2.3759992038281,-16.1777109780555));
#50512=CARTESIAN_POINT('Ctrl Pts',(-66.,-2.39225819818114,-16.1988986929781));
#50513=CARTESIAN_POINT('Ctrl Pts',(-66.,-2.39254363182917,-16.1992703530064));
#50514=CARTESIAN_POINT('',(-66.,-3.7256293105862,-15.9455420491152));
#50515=CARTESIAN_POINT('Origin',(-66.,0.,0.));
#50516=CARTESIAN_POINT('',(-66.,-3.67810171359515,-13.5729685048794));
#50517=CARTESIAN_POINT('Ctrl Pts',(-66.,-3.7256293105862,-15.9455420491152));
#50518=CARTESIAN_POINT('Ctrl Pts',(-66.,-3.72795164063846,-15.9356520429153));
#50519=CARTESIAN_POINT('Ctrl Pts',(-66.,-3.73513553846456,-15.9048096163928));
#50520=CARTESIAN_POINT('Ctrl Pts',(-66.,-3.74688765015641,-15.853028169516));
#50521=CARTESIAN_POINT('Ctrl Pts',(-66.,-3.76263238690138,-15.7803405987066));
#50522=CARTESIAN_POINT('Ctrl Pts',(-66.,-3.78146164640637,-15.6868150664286));
#50523=CARTESIAN_POINT('Ctrl Pts',(-66.,-3.80057004743305,-15.5823990924153));
#50524=CARTESIAN_POINT('Ctrl Pts',(-66.,-3.81772126627406,-15.4781490410999));
#50525=CARTESIAN_POINT('Ctrl Pts',(-66.,-3.83300795359517,-15.3740553411364));
#50526=CARTESIAN_POINT('Ctrl Pts',(-66.,-3.84657772273756,-15.2700970690198));
#50527=CARTESIAN_POINT('Ctrl Pts',(-66.,-3.85855158779829,-15.1662600850723));
#50528=CARTESIAN_POINT('Ctrl Pts',(-66.,-3.86894768714904,-15.0625540503165));
#50529=CARTESIAN_POINT('Ctrl Pts',(-66.,-3.87761375658259,-14.9590275514473));
#50530=CARTESIAN_POINT('Ctrl Pts',(-66.,-3.88412655939816,-14.8557904709058));
#50531=CARTESIAN_POINT('Ctrl Pts',(-66.,-3.88787877668998,-14.7529954092481));
#50532=CARTESIAN_POINT('Ctrl Pts',(-66.,-3.88822932173376,-14.6508052317201));
#50533=CARTESIAN_POINT('Ctrl Pts',(-66.,-3.88463805371054,-14.5493641299902));
#50534=CARTESIAN_POINT('Ctrl Pts',(-66.,-3.87679564863944,-14.4487695813147));
#50535=CARTESIAN_POINT('Ctrl Pts',(-66.,-3.86478832158859,-14.3490371882169));
#50536=CARTESIAN_POINT('Ctrl Pts',(-66.,-3.84902164513744,-14.2501151271916));
#50537=CARTESIAN_POINT('Ctrl Pts',(-66.,-3.83008256273264,-14.1519113521203));
#50538=CARTESIAN_POINT('Ctrl Pts',(-66.,-3.8086220490069,-14.0543164841154));
#50539=CARTESIAN_POINT('Ctrl Pts',(-66.,-3.7852344832017,-13.9572274551481));
#50540=CARTESIAN_POINT('Ctrl Pts',(-66.,-3.76032689601146,-13.8605729560155));
#50541=CARTESIAN_POINT('Ctrl Pts',(-66.,-3.73414411132176,-13.764309571506));
#50542=CARTESIAN_POINT('Ctrl Pts',(-66.,-3.71227892449176,-13.6875933984758));
#50543=CARTESIAN_POINT('Ctrl Pts',(-66.,-3.69538324295473,-13.6302181028421));
#50544=CARTESIAN_POINT('Ctrl Pts',(-66.,-3.68389897142971,-13.5920397328724));
#50545=CARTESIAN_POINT('Ctrl Pts',(-66.,-3.67810171359514,-13.5729685048794));
#50546=CARTESIAN_POINT('',(-66.,-5.00234392366024,-13.1426961282463));
#50547=CARTESIAN_POINT('Origin',(-66.,0.,0.));
#50548=CARTESIAN_POINT('',(-66.,-6.34597219029742,-15.0953390806557));
#50549=CARTESIAN_POINT('Ctrl Pts',(-66.,-5.00234392366024,-13.1426961282463));
#50550=CARTESIAN_POINT('Ctrl Pts',(-66.,-5.00975329143057,-13.1648626726972));
#50551=CARTESIAN_POINT('Ctrl Pts',(-66.,-5.02478822352796,-13.2091330988228));
#50552=CARTESIAN_POINT('Ctrl Pts',(-66.,-5.04798920255339,-13.2753507597416));
#50553=CARTESIAN_POINT('Ctrl Pts',(-66.,-5.08022280379478,-13.3632644309532));
#50554=CARTESIAN_POINT('Ctrl Pts',(-66.,-5.12272617691501,-13.4724958081193));
#50555=CARTESIAN_POINT('Ctrl Pts',(-66.,-5.16756435218796,-13.5809703610753));
#50556=CARTESIAN_POINT('Ctrl Pts',(-66.,-5.21496886213029,-13.6885022424853));
#50557=CARTESIAN_POINT('Ctrl Pts',(-66.,-5.26532059680125,-13.7947771174053));
#50558=CARTESIAN_POINT('Ctrl Pts',(-66.,-5.31911705202313,-13.8994109809482));
#50559=CARTESIAN_POINT('Ctrl Pts',(-66.,-5.37693249048282,-14.0020293939727));
#50560=CARTESIAN_POINT('Ctrl Pts',(-66.,-5.43936923240832,-14.102334498799));
#50561=CARTESIAN_POINT('Ctrl Pts',(-66.,-5.50704098217782,-14.2001904323636));
#50562=CARTESIAN_POINT('Ctrl Pts',(-66.,-5.58037590052447,-14.2956379130225));
#50563=CARTESIAN_POINT('Ctrl Pts',(-66.,-5.65928349609497,-14.3888825985252));
#50564=CARTESIAN_POINT('Ctrl Pts',(-66.,-5.7429409442582,-14.4802820917477));
#50565=CARTESIAN_POINT('Ctrl Pts',(-66.,-5.8293396720056,-14.5703597544468));
#50566=CARTESIAN_POINT('Ctrl Pts',(-66.,-5.91563026424745,-14.6597125620614));
#50567=CARTESIAN_POINT('Ctrl Pts',(-66.,-5.99951493159239,-14.7487702776409));
#50568=CARTESIAN_POINT('Ctrl Pts',(-66.,-6.08025962758854,-14.8376145740015));
#50569=CARTESIAN_POINT('Ctrl Pts',(-66.,-6.16012083060275,-14.925722782193));
#50570=CARTESIAN_POINT('Ctrl Pts',(-66.,-6.22820881535241,-14.9949633327447));
#50571=CARTESIAN_POINT('Ctrl Pts',(-66.,-6.28433170694406,-15.045518391722));
#50572=CARTESIAN_POINT('Ctrl Pts',(-66.,-6.32458593740117,-15.0785714650465));
#50573=CARTESIAN_POINT('Ctrl Pts',(-66.,-6.3456032959818,-15.0950500814723));
#50574=CARTESIAN_POINT('Ctrl Pts',(-66.,-6.34597219029742,-15.0953390806557));
#50575=CARTESIAN_POINT('',(-66.,-7.57407686781798,-14.5180571909737));
#50576=CARTESIAN_POINT('Origin',(-66.,0.,0.));
#50577=CARTESIAN_POINT('',(-66.,-6.93800739067722,-12.2318420402206));
#50578=CARTESIAN_POINT('Ctrl Pts',(-66.,-7.57407686781798,-14.5180571909737));
#50579=CARTESIAN_POINT('Ctrl Pts',(-66.,-7.57386669307527,-14.5079003575064));
#50580=CARTESIAN_POINT('Ctrl Pts',(-66.,-7.57315469596912,-14.4762403397886));
#50581=CARTESIAN_POINT('Ctrl Pts',(-66.,-7.57166007128053,-14.4231630709543));
#50582=CARTESIAN_POINT('Ctrl Pts',(-66.,-7.56883349438523,-14.3488435570404));
#50583=CARTESIAN_POINT('Ctrl Pts',(-66.,-7.56381234400904,-14.2535736549186));
#50584=CARTESIAN_POINT('Ctrl Pts',(-66.,-7.556353222684,-14.1476860346413));
#50585=CARTESIAN_POINT('Ctrl Pts',(-66.,-7.54703967094767,-14.0424458557121));
#50586=CARTESIAN_POINT('Ctrl Pts',(-66.,-7.53595904837785,-13.9378208062029));
#50587=CARTESIAN_POINT('Ctrl Pts',(-66.,-7.52324912730704,-13.8337539100138));
#50588=CARTESIAN_POINT('Ctrl Pts',(-66.,-7.50902360355704,-13.730201376709));
#50589=CARTESIAN_POINT('Ctrl Pts',(-66.,-7.49330244824787,-13.6271680529626));
#50590=CARTESIAN_POINT('Ctrl Pts',(-66.,-7.47595026385202,-13.5247388655977));
#50591=CARTESIAN_POINT('Ctrl Pts',(-66.,-7.45658443707985,-13.4231254995838));
#50592=CARTESIAN_POINT('Ctrl Pts',(-66.,-7.43465467928082,-13.32262679532));
#50593=CARTESIAN_POINT('Ctrl Pts',(-66.,-7.40958054758866,-13.2235599331263));
#50594=CARTESIAN_POINT('Ctrl Pts',(-66.,-7.38087472971119,-13.1261989021839));
#50595=CARTESIAN_POINT('Ctrl Pts',(-66.,-7.34826186125705,-13.0307150430677));
#50596=CARTESIAN_POINT('Ctrl Pts',(-66.,-7.31182932887926,-12.9371020273035));
#50597=CARTESIAN_POINT('Ctrl Pts',(-66.,-7.27195707536722,-12.8452087977179));
#50598=CARTESIAN_POINT('Ctrl Pts',(-66.,-7.22919071332107,-12.7548002330908));
#50599=CARTESIAN_POINT('Ctrl Pts',(-66.,-7.18413356438513,-12.6656085000656));
#50600=CARTESIAN_POINT('Ctrl Pts',(-66.,-7.13733570230759,-12.5773859525787));
#50601=CARTESIAN_POINT('Ctrl Pts',(-66.,-7.08917363628753,-12.4899622973194));
#50602=CARTESIAN_POINT('Ctrl Pts',(-66.,-7.03987370169386,-12.4032345978205));
#50603=CARTESIAN_POINT('Ctrl Pts',(-66.,-6.99961691350077,-12.3343662552827));
#50604=CARTESIAN_POINT('Ctrl Pts',(-66.,-6.96898338507103,-12.2829952952022));
#50605=CARTESIAN_POINT('Ctrl Pts',(-66.,-6.94836533853418,-12.24887239112));
#50606=CARTESIAN_POINT('Ctrl Pts',(-66.,-6.93800739067721,-12.2318420402206));
#50607=CARTESIAN_POINT('',(-66.,-8.11364170780698,-11.4857618157149));
#50608=CARTESIAN_POINT('Origin',(-66.,0.,0.));
#50609=CARTESIAN_POINT('',(-66.,-9.90065997719615,-13.0429121370937));
#50610=CARTESIAN_POINT('Ctrl Pts',(-66.,-8.11364170780698,-11.4857618157149));
#50611=CARTESIAN_POINT('Ctrl Pts',(-66.,-8.12633089210227,-11.5053893225758));
#50612=CARTESIAN_POINT('Ctrl Pts',(-66.,-8.15190308143842,-11.5445298762901));
#50613=CARTESIAN_POINT('Ctrl Pts',(-66.,-8.19084282166638,-11.6028973387695));
#50614=CARTESIAN_POINT('Ctrl Pts',(-66.,-8.24392698602517,-11.6800328696824));
#50615=CARTESIAN_POINT('Ctrl Pts',(-66.,-8.3122597763829,-11.775262383207));
#50616=CARTESIAN_POINT('Ctrl Pts',(-66.,-8.3826658022629,-11.8691782078618));
#50617=CARTESIAN_POINT('Ctrl Pts',(-66.,-8.45532310380908,-11.9615427552514));
#50618=CARTESIAN_POINT('Ctrl Pts',(-66.,-8.53052243279731,-12.0519568423361));
#50619=CARTESIAN_POINT('Ctrl Pts',(-66.,-8.60865015717173,-12.1399248062686));
#50620=CARTESIAN_POINT('Ctrl Pts',(-66.,-8.69016937887314,-12.2249411582788));
#50621=CARTESIAN_POINT('Ctrl Pts',(-66.,-8.77558942093922,-12.3065676074844));
#50622=CARTESIAN_POINT('Ctrl Pts',(-66.,-8.86547091932666,-12.3845199371372));
#50623=CARTESIAN_POINT('Ctrl Pts',(-66.,-8.96023870955522,-12.4587311071067));
#50624=CARTESIAN_POINT('Ctrl Pts',(-66.,-9.05985628822634,-12.5294228183105));
#50625=CARTESIAN_POINT('Ctrl Pts',(-66.,-9.16361561347667,-12.5971460670373));
#50626=CARTESIAN_POINT('Ctrl Pts',(-66.,-9.26970137008846,-12.6629072844668));
#50627=CARTESIAN_POINT('Ctrl Pts',(-66.,-9.37550212434126,-12.7279933116739));
#50628=CARTESIAN_POINT('Ctrl Pts',(-66.,-9.47889915384706,-12.7933918468958));
#50629=CARTESIAN_POINT('Ctrl Pts',(-66.,-9.57920178477654,-12.8593645469766));
#50630=CARTESIAN_POINT('Ctrl Pts',(-66.,-9.67846562159703,-12.9248440002217));
#50631=CARTESIAN_POINT('Ctrl Pts',(-66.,-9.76163392180467,-12.9749764383087));
#50632=CARTESIAN_POINT('Ctrl Pts',(-66.,-9.82856614146686,-13.0099860215666));
#50633=CARTESIAN_POINT('Ctrl Pts',(-66.,-9.87577567632734,-13.031989851782));
#50634=CARTESIAN_POINT('Ctrl Pts',(-66.,-9.9002308011995,-13.0427239576368));
#50635=CARTESIAN_POINT('Ctrl Pts',(-66.,-9.90065997719615,-13.0429121370937));
#50636=CARTESIAN_POINT('',(-66.,-10.9466173199386,-12.178349405844));
#50637=CARTESIAN_POINT('Origin',(-66.,0.,0.));
#50638=CARTESIAN_POINT('',(-66.,-9.76197254719673,-10.1221439546065));
#50639=CARTESIAN_POINT('Ctrl Pts',(-66.,-10.9466173199386,-12.178349405844));
#50640=CARTESIAN_POINT('Ctrl Pts',(-66.,-10.9438878464529,-12.1685639363102));
#50641=CARTESIAN_POINT('Ctrl Pts',(-66.,-10.9353246918112,-12.1380756427477));
#50642=CARTESIAN_POINT('Ctrl Pts',(-66.,-10.9206772435082,-12.0870375919612));
#50643=CARTESIAN_POINT('Ctrl Pts',(-66.,-10.8994569571944,-12.0157559033301));
#50644=CARTESIAN_POINT('Ctrl Pts',(-66.,-10.8709008942817,-11.9247277896931));
#50645=CARTESIAN_POINT('Ctrl Pts',(-66.,-10.8373429346305,-11.8240218317612));
#50646=CARTESIAN_POINT('Ctrl Pts',(-66.,-10.8021498170253,-11.7244041527066));
#50647=CARTESIAN_POINT('Ctrl Pts',(-66.,-10.7653981208323,-11.6258217302963));
#50648=CARTESIAN_POINT('Ctrl Pts',(-66.,-10.727207120633,-11.5281851158537));
#50649=CARTESIAN_POINT('Ctrl Pts',(-66.,-10.6876760500473,-11.4314236196986));
#50650=CARTESIAN_POINT('Ctrl Pts',(-66.,-10.6468254580846,-11.3355369696227));
#50651=CARTESIAN_POINT('Ctrl Pts',(-66.,-10.6045453214218,-11.2406410963124));
#50652=CARTESIAN_POINT('Ctrl Pts',(-66.,-10.5605176911805,-11.1470361863206));
#50653=CARTESIAN_POINT('Ctrl Pts',(-66.,-10.5142838856252,-11.055148542648));
#50654=CARTESIAN_POINT('Ctrl Pts',(-66.,-10.4653605771075,-10.9654297310826));
#50655=CARTESIAN_POINT('Ctrl Pts',(-66.,-10.4133439014856,-10.8782663225706));
#50656=CARTESIAN_POINT('Ctrl Pts',(-66.,-10.3580097561152,-10.7938927550471));
#50657=CARTESIAN_POINT('Ctrl Pts',(-66.,-10.2994412084092,-10.7122811666816));
#50658=CARTESIAN_POINT('Ctrl Pts',(-66.,-10.2379686981643,-10.6331907581101));
#50659=CARTESIAN_POINT('Ctrl Pts',(-66.,-10.1740622242879,-10.5562581065423));
#50660=CARTESIAN_POINT('Ctrl Pts',(-66.,-10.108239546518,-10.4810737531071));
#50661=CARTESIAN_POINT('Ctrl Pts',(-66.,-10.0409718699529,-10.4072610342189));
#50662=CARTESIAN_POINT('Ctrl Pts',(-66.,-9.97258152483879,-10.3345613726147));
#50663=CARTESIAN_POINT('Ctrl Pts',(-66.,-9.90326213654415,-10.2628187784479));
#50664=CARTESIAN_POINT('Ctrl Pts',(-66.,-9.84714322904426,-10.2061255176443));
#50665=CARTESIAN_POINT('Ctrl Pts',(-66.,-9.80469667097528,-10.163986719468));
#50666=CARTESIAN_POINT('Ctrl Pts',(-66.,-9.77624035711837,-10.1360633488319));
#50667=CARTESIAN_POINT('Ctrl Pts',(-66.,-9.76197254719672,-10.1221439546065));
#50668=CARTESIAN_POINT('',(-66.,-10.7151295435653,-9.10713484662511));
#50669=CARTESIAN_POINT('Origin',(-66.,0.,0.));
#50670=CARTESIAN_POINT('',(-66.,-12.8332528856473,-10.1709510554827));
#50671=CARTESIAN_POINT('Ctrl Pts',(-66.,-10.7151295435653,-9.10713484662511));
#50672=CARTESIAN_POINT('Ctrl Pts',(-66.,-10.7323012362688,-9.12299004745485));
#50673=CARTESIAN_POINT('Ctrl Pts',(-66.,-10.7668038881397,-9.15454138381928));
#50674=CARTESIAN_POINT('Ctrl Pts',(-66.,-10.8190356624814,-9.20139120553108));
#50675=CARTESIAN_POINT('Ctrl Pts',(-66.,-10.889634916681,-9.26290188705335));
#50676=CARTESIAN_POINT('Ctrl Pts',(-66.,-10.9795035237476,-9.33814591637203));
#50677=CARTESIAN_POINT('Ctrl Pts',(-66.,-11.0710535306934,-9.4116019360644));
#50678=CARTESIAN_POINT('Ctrl Pts',(-66.,-11.1643982983724,-9.48299554522798));
#50679=CARTESIAN_POINT('Ctrl Pts',(-66.,-11.2597201712738,-9.55186779486609));
#50680=CARTESIAN_POINT('Ctrl Pts',(-66.,-11.3572701125446,-9.61764250849074));
#50681=CARTESIAN_POINT('Ctrl Pts',(-66.,-11.4573709649815,-9.6797149094218));
#50682=CARTESIAN_POINT('Ctrl Pts',(-66.,-11.5604070517922,-9.73753381300202));
#50683=CARTESIAN_POINT('Ctrl Pts',(-66.,-11.6668507136929,-9.79068450718227));
#50684=CARTESIAN_POINT('Ctrl Pts',(-66.,-11.7770967670118,-9.83899640572359));
#50685=CARTESIAN_POINT('Ctrl Pts',(-66.,-11.8911649899478,-9.88269332242761));
#50686=CARTESIAN_POINT('Ctrl Pts',(-66.,-12.0085066122796,-9.9224850258725));
#50687=CARTESIAN_POINT('Ctrl Pts',(-66.,-12.1276136395118,-9.95979777888845));
#50688=CARTESIAN_POINT('Ctrl Pts',(-66.,-12.2462767052779,-9.99652743122885));
#50689=CARTESIAN_POINT('Ctrl Pts',(-66.,-12.362689281313,-10.0341575556064));
#50690=CARTESIAN_POINT('Ctrl Pts',(-66.,-12.4762474639872,-10.0731133520306));
#50691=CARTESIAN_POINT('Ctrl Pts',(-66.,-12.5886768226797,-10.1118497354652));
#50692=CARTESIAN_POINT('Ctrl Pts',(-66.,-12.6816996681717,-10.1397240556283));
#50693=CARTESIAN_POINT('Ctrl Pts',(-66.,-12.7552356183835,-10.1569883822946));
#50694=CARTESIAN_POINT('Ctrl Pts',(-66.,-12.8064341089476,-10.166560387824));
#50695=CARTESIAN_POINT('Ctrl Pts',(-66.,-12.8327903946759,-10.1708755197597));
#50696=CARTESIAN_POINT('Ctrl Pts',(-66.,-12.8332528856473,-10.1709510554827));
#50697=CARTESIAN_POINT('',(-66.,-13.631341547005,-9.07343113870903));
#50698=CARTESIAN_POINT('Origin',(-66.,0.,0.));
#50699=CARTESIAN_POINT('',(-66.,-11.9725570665522,-7.37643433768308));
#50700=CARTESIAN_POINT('Ctrl Pts',(-66.,-13.631341547005,-9.07343113870903));
#50701=CARTESIAN_POINT('Ctrl Pts',(-66.,-13.6262642776339,-9.06463189014802));
#50702=CARTESIAN_POINT('Ctrl Pts',(-66.,-13.6103880199559,-9.03723101235338));
#50703=CARTESIAN_POINT('Ctrl Pts',(-66.,-13.5835081010849,-8.99143908805054));
#50704=CARTESIAN_POINT('Ctrl Pts',(-66.,-13.5452274539844,-8.92767411535463));
#50705=CARTESIAN_POINT('Ctrl Pts',(-66.,-13.4949307609898,-8.84660742136017));
#50706=CARTESIAN_POINT('Ctrl Pts',(-66.,-13.4373825330349,-8.7574108514811));
#50707=CARTESIAN_POINT('Ctrl Pts',(-66.,-13.3785211625712,-8.66967501744431));
#50708=CARTESIAN_POINT('Ctrl Pts',(-66.,-13.3184076369901,-8.58332951829382));
#50709=CARTESIAN_POINT('Ctrl Pts',(-66.,-13.2571352386615,-8.49825805316535));
#50710=CARTESIAN_POINT('Ctrl Pts',(-66.,-13.1947825037901,-8.41436747482742));
#50711=CARTESIAN_POINT('Ctrl Pts',(-66.,-13.1313692681049,-8.3316524092927));
#50712=CARTESIAN_POINT('Ctrl Pts',(-66.,-13.0668177956572,-8.25025250675973));
#50713=CARTESIAN_POINT('Ctrl Pts',(-66.,-13.0008947798771,-8.17053759353955));
#50714=CARTESIAN_POINT('Ctrl Pts',(-66.,-12.9332619666045,-8.09303464904925));
#50715=CARTESIAN_POINT('Ctrl Pts',(-66.,-12.8635635126628,-8.01830125100551));
#50716=CARTESIAN_POINT('Ctrl Pts',(-66.,-12.7915043783298,-7.9468122624453));
#50717=CARTESIAN_POINT('Ctrl Pts',(-66.,-12.7169258039014,-7.87885048806616));
#50718=CARTESIAN_POINT('Ctrl Pts',(-66.,-12.6399013181197,-7.81436828334278));
#50719=CARTESIAN_POINT('Ctrl Pts',(-66.,-12.5606910950408,-7.75305023703025));
#50720=CARTESIAN_POINT('Ctrl Pts',(-66.,-12.4796599881192,-7.69442745995809));
#50721=CARTESIAN_POINT('Ctrl Pts',(-66.,-12.3972076624386,-7.63797459554787));
#50722=CARTESIAN_POINT('Ctrl Pts',(-66.,-12.3136968468978,-7.58320962985052));
#50723=CARTESIAN_POINT('Ctrl Pts',(-66.,-12.2293754395952,-7.5298019490105));
#50724=CARTESIAN_POINT('Ctrl Pts',(-66.,-12.144392189705,-7.47755231121817));
#50725=CARTESIAN_POINT('Ctrl Pts',(-66.,-12.0759373202474,-7.43659637822836));
#50726=CARTESIAN_POINT('Ctrl Pts',(-66.,-12.0243448058902,-7.40633747762124));
#50727=CARTESIAN_POINT('Ctrl Pts',(-66.,-11.9898382395678,-7.38636816850343));
#50728=CARTESIAN_POINT('Ctrl Pts',(-66.,-11.9725570665522,-7.37643433768309));
#50729=CARTESIAN_POINT('',(-66.,-12.6433463826116,-6.1562731014228));
#50730=CARTESIAN_POINT('Origin',(-66.,0.,0.));
#50731=CARTESIAN_POINT('',(-66.,-14.9594853178907,-6.65991171291435));
#50732=CARTESIAN_POINT('Ctrl Pts',(-66.,-12.6433463826116,-6.1562731014228));
#50733=CARTESIAN_POINT('Ctrl Pts',(-66.,-12.6639216231176,-6.16735975564195));
#50734=CARTESIAN_POINT('Ctrl Pts',(-66.,-12.7051868090144,-6.18933938815496));
#50735=CARTESIAN_POINT('Ctrl Pts',(-66.,-12.7674287029928,-6.22172782249946));
#50736=CARTESIAN_POINT('Ctrl Pts',(-66.,-12.851107036246,-6.26374871229064));
#50737=CARTESIAN_POINT('Ctrl Pts',(-66.,-12.9568646849259,-6.31427939831312));
#50738=CARTESIAN_POINT('Ctrl Pts',(-66.,-13.0638062493037,-6.3626601011734));
#50739=CARTESIAN_POINT('Ctrl Pts',(-66.,-13.1719732880642,-6.40859684907992));
#50740=CARTESIAN_POINT('Ctrl Pts',(-66.,-13.281428281035,-6.45159976453225));
#50741=CARTESIAN_POINT('Ctrl Pts',(-66.,-13.3922710176287,-6.49104836068956));
#50742=CARTESIAN_POINT('Ctrl Pts',(-66.,-13.5046637960973,-6.52627657330457));
#50743=CARTESIAN_POINT('Ctrl Pts',(-66.,-13.6188417913781,-6.55665495690443));
#50744=CARTESIAN_POINT('Ctrl Pts',(-66.,-13.7351593700424,-6.58166436202222));
#50745=CARTESIAN_POINT('Ctrl Pts',(-66.,-13.8539565214648,-6.60104137487127));
#50746=CARTESIAN_POINT('Ctrl Pts',(-66.,-13.9753080627051,-6.61499785909296));
#50747=CARTESIAN_POINT('Ctrl Pts',(-66.,-14.0988589764351,-6.62435775818486));
#50748=CARTESIAN_POINT('Ctrl Pts',(-66.,-14.2235033417215,-6.63087754928856));
#50749=CARTESIAN_POINT('Ctrl Pts',(-66.,-14.3475726821666,-6.63694296762358));
#50750=CARTESIAN_POINT('Ctrl Pts',(-66.,-14.4696861744433,-6.64444024204806));
#50751=CARTESIAN_POINT('Ctrl Pts',(-66.,-14.5893646306071,-6.65393139885702));
#50752=CARTESIAN_POINT('Ctrl Pts',(-66.,-14.7078951610787,-6.6634907630476));
#50753=CARTESIAN_POINT('Ctrl Pts',(-66.,-14.8049275843586,-6.66735551923628));
#50754=CARTESIAN_POINT('Ctrl Pts',(-66.,-14.880446730922,-6.66578980817273));
#50755=CARTESIAN_POINT('Ctrl Pts',(-66.,-14.9324171877326,-6.66232854470537));
#50756=CARTESIAN_POINT('Ctrl Pts',(-66.,-14.9590185719531,-6.65995356711245));
#50757=CARTESIAN_POINT('Ctrl Pts',(-66.,-14.9594853178907,-6.65991171291435));
#50758=CARTESIAN_POINT('',(-66.,-15.4595584521058,-5.39839582338346));
#50759=CARTESIAN_POINT('Origin',(-66.,0.,0.));
#50760=CARTESIAN_POINT('',(-66.,-13.4308617934315,-4.16723622269519));
#50761=CARTESIAN_POINT('Ctrl Pts',(-66.,-15.4595584521058,-5.39839582338346));
#50762=CARTESIAN_POINT('Ctrl Pts',(-66.,-15.4524524103566,-5.3911356849437));
#50763=CARTESIAN_POINT('Ctrl Pts',(-66.,-15.430260613301,-5.36854392084221));
#50764=CARTESIAN_POINT('Ctrl Pts',(-66.,-15.3928371880222,-5.33087539803783));
#50765=CARTESIAN_POINT('Ctrl Pts',(-66.,-15.3399014939787,-5.27863372902275));
#50766=CARTESIAN_POINT('Ctrl Pts',(-66.,-15.2710244971014,-5.21262217319695));
#50767=CARTESIAN_POINT('Ctrl Pts',(-66.,-15.1931019676527,-5.14053953989829));
#50768=CARTESIAN_POINT('Ctrl Pts',(-66.,-15.1142708207137,-5.07019831600168));
#50769=CARTESIAN_POINT('Ctrl Pts',(-66.,-15.0345726196388,-5.00151514537911));
#50770=CARTESIAN_POINT('Ctrl Pts',(-66.,-14.954068793312,-4.9343541825898));
#50771=CARTESIAN_POINT('Ctrl Pts',(-66.,-14.8728122458042,-4.86860567563393));
#50772=CARTESIAN_POINT('Ctrl Pts',(-66.,-14.7908208532122,-4.80425948641264));
#50773=CARTESIAN_POINT('Ctrl Pts',(-66.,-14.7080540513971,-4.74147020990105));
#50774=CARTESIAN_POINT('Ctrl Pts',(-66.,-14.6243778356077,-4.68065407462106));
#50775=CARTESIAN_POINT('Ctrl Pts',(-66.,-14.5395956330118,-4.62240562435127));
#50776=CARTESIAN_POINT('Ctrl Pts',(-66.,-14.4535014438403,-4.56735341407851));
#50777=CARTESIAN_POINT('Ctrl Pts',(-66.,-14.3659275912213,-4.51603076153944));
#50778=CARTESIAN_POINT('Ctrl Pts',(-66.,-14.2767906338471,-4.4687510685349));
#50779=CARTESIAN_POINT('Ctrl Pts',(-66.,-14.1861499417075,-4.42544990152536));
#50780=CARTESIAN_POINT('Ctrl Pts',(-66.,-14.0941790754254,-4.38575705583354));
#50781=CARTESIAN_POINT('Ctrl Pts',(-66.,-14.0011148179182,-4.34912763794002));
#50782=CARTESIAN_POINT('Ctrl Pts',(-66.,-13.9072136271877,-4.31495340364481));
#50783=CARTESIAN_POINT('Ctrl Pts',(-66.,-13.8127069643429,-4.28267727534445));
#50784=CARTESIAN_POINT('Ctrl Pts',(-66.,-13.717752718985,-4.25191737627554));
#50785=CARTESIAN_POINT('Ctrl Pts',(-66.,-13.6224454176364,-4.22244373176092));
#50786=CARTESIAN_POINT('Ctrl Pts',(-66.,-13.5459558574286,-4.19979853847996));
#50787=CARTESIAN_POINT('Ctrl Pts',(-66.,-13.4884591342042,-4.1833208134517));
#50788=CARTESIAN_POINT('Ctrl Pts',(-66.,-13.4500704898848,-4.17256031098595));
#50789=CARTESIAN_POINT('Ctrl Pts',(-66.,-13.4308617934315,-4.1672362226952));
#50790=CARTESIAN_POINT('',(-66.,-13.7771352694631,-2.8185900760694));
#50791=CARTESIAN_POINT('Origin',(-66.,0.,0.));
#50792=CARTESIAN_POINT('',(-66.,-16.1457582704724,-2.73040562398164));
#50793=CARTESIAN_POINT('Ctrl Pts',(-66.,-13.7771352694631,-2.8185900760694));
#50794=CARTESIAN_POINT('Ctrl Pts',(-66.,-13.7998212397401,-2.82421156841951));
#50795=CARTESIAN_POINT('Ctrl Pts',(-66.,-13.8452561162702,-2.83523843593487));
#50796=CARTESIAN_POINT('Ctrl Pts',(-66.,-13.913597242777,-2.85113039846586));
#50797=CARTESIAN_POINT('Ctrl Pts',(-66.,-14.0050968376581,-2.87102116947837));
#50798=CARTESIAN_POINT('Ctrl Pts',(-66.,-14.1200983859353,-2.89366348336299));
#50799=CARTESIAN_POINT('Ctrl Pts',(-66.,-14.2357119759516,-2.91392893189869));
#50800=CARTESIAN_POINT('Ctrl Pts',(-66.,-14.3519047529378,-2.93152244373364));
#50801=CARTESIAN_POINT('Ctrl Pts',(-66.,-14.4686154062224,-2.94595399366867));
#50802=CARTESIAN_POINT('Ctrl Pts',(-66.,-14.5857862813476,-2.95659777198027));
#50803=CARTESIAN_POINT('Ctrl Pts',(-66.,-14.703408934225,-2.96276827812033));
#50804=CARTESIAN_POINT('Ctrl Pts',(-66.,-14.8215546146151,-2.96379735617437));
#50805=CARTESIAN_POINT('Ctrl Pts',(-66.,-14.9404374487894,-2.959094039328));
#50806=CARTESIAN_POINT('Ctrl Pts',(-66.,-15.0603212363863,-2.9483186375038));
#50807=CARTESIAN_POINT('Ctrl Pts',(-66.,-15.181331132295,-2.93165775201116));
#50808=CARTESIAN_POINT('Ctrl Pts',(-66.,-15.3033281791249,-2.90999772986683));
#50809=CARTESIAN_POINT('Ctrl Pts',(-66.,-15.4256780185848,-2.88531489660512));
#50810=CARTESIAN_POINT('Ctrl Pts',(-66.,-15.5473579007536,-2.86033496839371));
#50811=CARTESIAN_POINT('Ctrl Pts',(-66.,-15.6674994694501,-2.83722831154002));
#50812=CARTESIAN_POINT('Ctrl Pts',(-66.,-15.7857783615561,-2.81665846444538));
#50813=CARTESIAN_POINT('Ctrl Pts',(-66.,-15.9029623546524,-2.7964401593829));
#50814=CARTESIAN_POINT('Ctrl Pts',(-66.,-15.9979074517054,-2.77605251475231));
#50815=CARTESIAN_POINT('Ctrl Pts',(-66.,-16.0706646489018,-2.75575514534332));
#50816=CARTESIAN_POINT('Ctrl Pts',(-66.,-16.1201415770235,-2.73947809679247));
#50817=CARTESIAN_POINT('Ctrl Pts',(-66.,-16.1453165969326,-2.73056223824769));
#50818=CARTESIAN_POINT('Ctrl Pts',(-66.,-16.1457582704724,-2.73040562398164));
#50819=CARTESIAN_POINT('',(-66.,-16.3163944433819,-1.38415944456368));
#50820=CARTESIAN_POINT('Origin',(-66.,0.,0.));
#50821=CARTESIAN_POINT('',(-66.,-14.045256078575,-0.696195329812616));
#50822=CARTESIAN_POINT('Ctrl Pts',(-66.,-16.3163944433819,-1.38415944456368));
#50823=CARTESIAN_POINT('Ctrl Pts',(-66.,-16.307706127992,-1.37889459744425));
#50824=CARTESIAN_POINT('Ctrl Pts',(-66.,-16.2805931837835,-1.36253147066111));
#50825=CARTESIAN_POINT('Ctrl Pts',(-66.,-16.2349777035408,-1.33535320117812));
#50826=CARTESIAN_POINT('Ctrl Pts',(-66.,-16.170713106895,-1.29791737203952));
#50827=CARTESIAN_POINT('Ctrl Pts',(-66.,-16.0875836011606,-1.25110870320843));
#50828=CARTESIAN_POINT('Ctrl Pts',(-66.,-15.9941829293225,-1.20066922344171));
#50829=CARTESIAN_POINT('Ctrl Pts',(-66.,-15.900335256791,-1.15214240747963));
#50830=CARTESIAN_POINT('Ctrl Pts',(-66.,-15.8060601113054,-1.10543718159424));
#50831=CARTESIAN_POINT('Ctrl Pts',(-66.,-15.7113832084608,-1.06040669143688));
#50832=CARTESIAN_POINT('Ctrl Pts',(-66.,-15.6163284960372,-1.01693147636119));
#50833=CARTESIAN_POINT('Ctrl Pts',(-66.,-15.5209107672782,-0.974997271170846));
#50834=CARTESIAN_POINT('Ctrl Pts',(-66.,-15.4251291786488,-0.934763901846662));
#50835=CARTESIAN_POINT('Ctrl Pts',(-66.,-15.3289574472276,-0.89666784595261));
#50836=CARTESIAN_POINT('Ctrl Pts',(-66.,-15.2323530329047,-0.861333854256595));
#50837=CARTESIAN_POINT('Ctrl Pts',(-66.,-15.1352727230412,-0.829421964594113));
#50838=CARTESIAN_POINT('Ctrl Pts',(-66.,-15.0376867393704,-0.801490439086723));
#50839=CARTESIAN_POINT('Ctrl Pts',(-66.,-14.939592201905,-0.777863584450799));
#50840=CARTESIAN_POINT('Ctrl Pts',(-66.,-14.8410305914479,-0.758464226728878));
#50841=CARTESIAN_POINT('Ctrl Pts',(-66.,-14.7420779497362,-0.742890629132665));
#50842=CARTESIAN_POINT('Ctrl Pts',(-66.,-14.6428281112089,-0.730556131457601));
#50843=CARTESIAN_POINT('Ctrl Pts',(-66.,-14.5433782125866,-0.72080782010221));
#50844=CARTESIAN_POINT('Ctrl Pts',(-66.,-14.4438139036356,-0.71304855704325));
#50845=CARTESIAN_POINT('Ctrl Pts',(-66.,-14.3441931446757,-0.706869197330954));
#50846=CARTESIAN_POINT('Ctrl Pts',(-66.,-14.2445503001281,-0.702023483575367));
#50847=CARTESIAN_POINT('Ctrl Pts',(-66.,-14.1648321695468,-0.699111910780302));
#50848=CARTESIAN_POINT('Ctrl Pts',(-66.,-14.1050439680336,-0.697450717395246));
#50849=CARTESIAN_POINT('Ctrl Pts',(-66.,-14.0651853454231,-0.696575143525857));
#50850=CARTESIAN_POINT('Ctrl Pts',(-66.,-14.045256078575,-0.696195329812629));
#50851=CARTESIAN_POINT('',(-66.,-14.045256078575,0.696195329812624));
#50852=CARTESIAN_POINT('Origin',(-66.,0.,0.));
#50853=CARTESIAN_POINT('',(-66.,-16.3175338509752,1.37066189203528));
#50854=CARTESIAN_POINT('Ctrl Pts',(-66.,-14.045256078575,0.696195329812624));
#50855=CARTESIAN_POINT('Ctrl Pts',(-66.,-14.0686273356774,0.696392218370307));
#50856=CARTESIAN_POINT('Ctrl Pts',(-66.,-14.1153770624506,0.697010974492569));
#50857=CARTESIAN_POINT('Ctrl Pts',(-66.,-14.1855232971663,0.698614034227448));
#50858=CARTESIAN_POINT('Ctrl Pts',(-66.,-14.279094897617,0.702103192289484));
#50859=CARTESIAN_POINT('Ctrl Pts',(-66.,-14.3961143752671,0.708771950396692));
#50860=CARTESIAN_POINT('Ctrl Pts',(-66.,-14.5131355638642,0.717895108848178));
#50861=CARTESIAN_POINT('Ctrl Pts',(-66.,-14.6300532595709,0.7297502981378));
#50862=CARTESIAN_POINT('Ctrl Pts',(-66.,-14.7466862135917,0.744796901078022));
#50863=CARTESIAN_POINT('Ctrl Pts',(-66.,-14.8628229502399,0.763626728348506));
#50864=CARTESIAN_POINT('Ctrl Pts',(-66.,-14.97828481366,0.786901644277719));
#50865=CARTESIAN_POINT('Ctrl Pts',(-66.,-15.0929746515511,0.81528653252832));
#50866=CARTESIAN_POINT('Ctrl Pts',(-66.,-15.2069528955437,0.849407044643804));
#50867=CARTESIAN_POINT('Ctrl Pts',(-66.,-15.3203905800386,0.889657803015486));
#50868=CARTESIAN_POINT('Ctrl Pts',(-66.,-15.4334553338124,0.935889193512498));
#50869=CARTESIAN_POINT('Ctrl Pts',(-66.,-15.5462329906162,0.987208158041752));
#50870=CARTESIAN_POINT('Ctrl Pts',(-66.,-15.6586006138651,1.04154270247793));
#50871=CARTESIAN_POINT('Ctrl Pts',(-66.,-15.7702454432537,1.09599839647648));
#50872=CARTESIAN_POINT('Ctrl Pts',(-66.,-15.8808661517589,1.14825710837788));
#50873=CARTESIAN_POINT('Ctrl Pts',(-66.,-15.9903135820168,1.19759548023257));
#50874=CARTESIAN_POINT('Ctrl Pts',(-66.,-16.0987879364791,1.2463210640833));
#50875=CARTESIAN_POINT('Ctrl Pts',(-66.,-16.1856799576735,1.28968007884051));
#50876=CARTESIAN_POINT('Ctrl Pts',(-66.,-16.2511036032208,1.32743374822648));
#50877=CARTESIAN_POINT('Ctrl Pts',(-66.,-16.2949781852964,1.35550383503756));
#50878=CARTESIAN_POINT('Ctrl Pts',(-66.,-16.317145001806,1.37040035835162));
#50879=CARTESIAN_POINT('Ctrl Pts',(-66.,-16.3175338509752,1.37066189203528));
#50880=CARTESIAN_POINT('',(-66.,-16.1480113642792,2.71704876274038));
#50881=CARTESIAN_POINT('Origin',(-66.,0.,0.));
#50882=CARTESIAN_POINT('',(-66.,-13.7771352694631,2.8185900760694));
#50883=CARTESIAN_POINT('Ctrl Pts',(-66.,-16.1480113642792,2.71704876274038));
#50884=CARTESIAN_POINT('Ctrl Pts',(-66.,-16.1382866940579,2.7199875088322));
#50885=CARTESIAN_POINT('Ctrl Pts',(-66.,-16.1079562086956,2.72909384286184));
#50886=CARTESIAN_POINT('Ctrl Pts',(-66.,-16.0570148618746,2.74407414839715));
#50887=CARTESIAN_POINT('Ctrl Pts',(-66.,-15.9854593435823,2.76435190683515));
#50888=CARTESIAN_POINT('Ctrl Pts',(-66.,-15.8933006615651,2.78901652785862));
#50889=CARTESIAN_POINT('Ctrl Pts',(-66.,-15.7902905550528,2.81464355607623));
#50890=CARTESIAN_POINT('Ctrl Pts',(-66.,-15.6873231513416,2.83830684578773));
#50891=CARTESIAN_POINT('Ctrl Pts',(-66.,-15.5843947155558,2.86009946582377));
#50892=CARTESIAN_POINT('Ctrl Pts',(-66.,-15.4814936341966,2.88017005204204));
#50893=CARTESIAN_POINT('Ctrl Pts',(-66.,-15.3786133940255,2.89864026758367));
#50894=CARTESIAN_POINT('Ctrl Pts',(-66.,-15.2757647759192,2.91552760840775));
#50895=CARTESIAN_POINT('Ctrl Pts',(-66.,-15.1729867099492,2.9306770599819));
#50896=CARTESIAN_POINT('Ctrl Pts',(-66.,-15.0703622864763,2.94365932119071));
#50897=CARTESIAN_POINT('Ctrl Pts',(-66.,-14.9680056710645,2.95385868966535));
#50898=CARTESIAN_POINT('Ctrl Pts',(-66.,-14.8660391534142,2.96062511732634));
#50899=CARTESIAN_POINT('Ctrl Pts',(-66.,-14.7645727249416,2.96341047532946));
#50900=CARTESIAN_POINT('Ctrl Pts',(-66.,-14.6636842479405,2.96189992942649));
#50901=CARTESIAN_POINT('Ctrl Pts',(-66.,-14.5633947076351,2.95617854486928));
#50902=CARTESIAN_POINT('Ctrl Pts',(-66.,-14.463677848895,2.94665434795724));
#50903=CARTESIAN_POINT('Ctrl Pts',(-66.,-14.3644786617177,2.93391890356181));
#50904=CARTESIAN_POINT('Ctrl Pts',(-66.,-14.2657288580852,2.91862876972314));
#50905=CARTESIAN_POINT('Ctrl Pts',(-66.,-14.1673628947312,2.90138362450613));
#50906=CARTESIAN_POINT('Ctrl Pts',(-66.,-14.0693351608341,2.882594172965));
#50907=CARTESIAN_POINT('Ctrl Pts',(-66.,-13.9716176994713,2.862507481945));
#50908=CARTESIAN_POINT('Ctrl Pts',(-66.,-13.8936799818437,2.84550248942744));
#50909=CARTESIAN_POINT('Ctrl Pts',(-66.,-13.8353570146283,2.83224277227946));
#50910=CARTESIAN_POINT('Ctrl Pts',(-66.,-13.7965328775753,2.82317840202614));
#50911=CARTESIAN_POINT('Ctrl Pts',(-66.,-13.7771352694631,2.81859007606939));
#50912=CARTESIAN_POINT('',(-66.,-13.4308617934315,4.1672362226952));
#50913=CARTESIAN_POINT('Origin',(-66.,0.,0.));
#50914=CARTESIAN_POINT('',(-66.,-15.4640187679296,5.38560568043381));
#50915=CARTESIAN_POINT('Ctrl Pts',(-66.,-13.4308617934315,4.1672362226952));
#50916=CARTESIAN_POINT('Ctrl Pts',(-66.,-13.4534498353221,4.1732391209285));
#50917=CARTESIAN_POINT('Ctrl Pts',(-66.,-13.4985769550718,4.18546462196559));
#50918=CARTESIAN_POINT('Ctrl Pts',(-66.,-13.5661207520894,4.20446197782756));
#50919=CARTESIAN_POINT('Ctrl Pts',(-66.,-13.655884910321,4.23111182833087));
#50920=CARTESIAN_POINT('Ctrl Pts',(-66.,-13.7675695531958,4.26667263583206));
#50921=CARTESIAN_POINT('Ctrl Pts',(-66.,-13.8786454687203,4.30461115967259));
#50922=CARTESIAN_POINT('Ctrl Pts',(-66.,-13.988941714333,4.34517014494338));
#50923=CARTESIAN_POINT('Ctrl Pts',(-66.,-14.0981684916428,4.38874946735859));
#50924=CARTESIAN_POINT('Ctrl Pts',(-66.,-14.2059737915295,4.4358697529125));
#50925=CARTESIAN_POINT('Ctrl Pts',(-66.,-14.3120199719745,4.48712764234399));
#50926=CARTESIAN_POINT('Ctrl Pts',(-66.,-14.4160475830522,4.54314296997813));
#50927=CARTESIAN_POINT('Ctrl Pts',(-66.,-14.5179595646104,4.60453676010005));
#50928=CARTESIAN_POINT('Ctrl Pts',(-66.,-14.6178234390918,4.67173377183878));
#50929=CARTESIAN_POINT('Ctrl Pts',(-66.,-14.7158387764281,4.74463077904808));
#50930=CARTESIAN_POINT('Ctrl Pts',(-66.,-14.8123108082616,4.82238412668293));
#50931=CARTESIAN_POINT('Ctrl Pts',(-66.,-14.9076357442716,4.90295634303817));
#50932=CARTESIAN_POINT('Ctrl Pts',(-66.,-15.0022304656484,4.98346615129592));
#50933=CARTESIAN_POINT('Ctrl Pts',(-66.,-15.0963796080126,5.06159331118216));
#50934=CARTESIAN_POINT('Ctrl Pts',(-66.,-15.1901185918597,5.13660009643943));
#50935=CARTESIAN_POINT('Ctrl Pts',(-66.,-15.2830674650563,5.2107713514449));
#50936=CARTESIAN_POINT('Ctrl Pts',(-66.,-15.3564466651341,5.27437732996824));
#50937=CARTESIAN_POINT('Ctrl Pts',(-66.,-15.4104259507712,5.32721509743538));
#50938=CARTESIAN_POINT('Ctrl Pts',(-66.,-15.4459413854495,5.3653144757178));
#50939=CARTESIAN_POINT('Ctrl Pts',(-66.,-15.4637071759544,5.38525566045572));
#50940=CARTESIAN_POINT('Ctrl Pts',(-66.,-15.4640187679296,5.38560568043381));
#50941=CARTESIAN_POINT('',(-66.,-14.9649893429273,6.64753480367511));
#50942=CARTESIAN_POINT('Origin',(-66.,0.,0.));
#50943=CARTESIAN_POINT('',(-66.,-12.6433463826116,6.15627310142281));
#50944=CARTESIAN_POINT('Ctrl Pts',(-66.,-14.9649893429273,6.64753480367511));
#50945=CARTESIAN_POINT('Ctrl Pts',(-66.,-14.9548393546694,6.64796279651443));
#50946=CARTESIAN_POINT('Ctrl Pts',(-66.,-14.9231971040963,6.64924015333274));
#50947=CARTESIAN_POINT('Ctrl Pts',(-66.,-14.870130722867,6.65108122722986));
#50948=CARTESIAN_POINT('Ctrl Pts',(-66.,-14.7957803793054,6.65292678882822));
#50949=CARTESIAN_POINT('Ctrl Pts',(-66.,-14.7003831899324,6.65389759319505));
#50950=CARTESIAN_POINT('Ctrl Pts',(-66.,-14.5942361525827,6.65310192943101));
#50951=CARTESIAN_POINT('Ctrl Pts',(-66.,-14.4886188383546,6.65041484137187));
#50952=CARTESIAN_POINT('Ctrl Pts',(-66.,-14.3835044844334,6.64592554509403));
#50953=CARTESIAN_POINT('Ctrl Pts',(-66.,-14.278844877945,6.63977511862666));
#50954=CARTESIAN_POINT('Ctrl Pts',(-66.,-14.1746034538834,6.63207978306306));
#50955=CARTESIAN_POINT('Ctrl Pts',(-66.,-14.0707863033563,6.6228591657896));
#50956=CARTESIAN_POINT('Ctrl Pts',(-66.,-13.9674696839217,6.61197280385553));
#50957=CARTESIAN_POINT('Ctrl Pts',(-66.,-13.8648408383502,6.59902554716193));
#50958=CARTESIAN_POINT('Ctrl Pts',(-66.,-13.7631634644371,6.58344942858329));
#50959=CARTESIAN_POINT('Ctrl Pts',(-66.,-13.6627176703106,6.56464523470766));
#50960=CARTESIAN_POINT('Ctrl Pts',(-66.,-13.5637463059047,6.54210941091933));
#50961=CARTESIAN_POINT('Ctrl Pts',(-66.,-13.4664030834197,6.51555637763196));
#50962=CARTESIAN_POINT('Ctrl Pts',(-66.,-13.3706871739224,6.48507374642914));
#50963=CARTESIAN_POINT('Ctrl Pts',(-66.,-13.2764716751216,6.45105019532836));
#50964=CARTESIAN_POINT('Ctrl Pts',(-66.,-13.1835561890537,6.41404502367149));
#50965=CARTESIAN_POINT('Ctrl Pts',(-66.,-13.0917112937495,6.37467717998103));
#50966=CARTESIAN_POINT('Ctrl Pts',(-66.,-13.0007243712348,6.33351120238525));
#50967=CARTESIAN_POINT('Ctrl Pts',(-66.,-12.9104491054422,6.29093354993378));
#50968=CARTESIAN_POINT('Ctrl Pts',(-66.,-12.8207969747412,6.24717657480866));
#50969=CARTESIAN_POINT('Ctrl Pts',(-66.,-12.7495367835008,6.21132350319834));
#50970=CARTESIAN_POINT('Ctrl Pts',(-66.,-12.6963436971102,6.18397603231157));
#50971=CARTESIAN_POINT('Ctrl Pts',(-66.,-12.6609935089309,6.16554126565498));
#50972=CARTESIAN_POINT('Ctrl Pts',(-66.,-12.6433463826116,6.1562731014228));
#50973=CARTESIAN_POINT('',(-66.,-11.9725570665522,7.37643433768309));
#50974=CARTESIAN_POINT('Origin',(-66.,0.,0.));
#50975=CARTESIAN_POINT('',(-66.,-13.6388425130122,9.0621520570585));
#50976=CARTESIAN_POINT('Ctrl Pts',(-66.,-11.9725570665522,7.37643433768309));
#50977=CARTESIAN_POINT('Ctrl Pts',(-66.,-11.9929426034861,7.38786606141889));
#50978=CARTESIAN_POINT('Ctrl Pts',(-66.,-12.0336116133124,7.4109301341784));
#50979=CARTESIAN_POINT('Ctrl Pts',(-66.,-12.0943089474566,7.44612811243127));
#50980=CARTESIAN_POINT('Ctrl Pts',(-66.,-12.174625451278,7.49426414725743));
#50981=CARTESIAN_POINT('Ctrl Pts',(-66.,-12.2739577025182,7.5564825878338));
#50982=CARTESIAN_POINT('Ctrl Pts',(-66.,-12.3721090366891,7.62085266008235));
#50983=CARTESIAN_POINT('Ctrl Pts',(-66.,-12.4688535134548,7.68756697112423));
#50984=CARTESIAN_POINT('Ctrl Pts',(-66.,-12.5638109939272,7.75694076391353));
#50985=CARTESIAN_POINT('Ctrl Pts',(-66.,-12.6565110535803,7.82939076691323));
#50986=CARTESIAN_POINT('Ctrl Pts',(-66.,-12.7464782795223,7.9054109081407));
#50987=CARTESIAN_POINT('Ctrl Pts',(-66.,-12.8333072263957,7.98553702611316));
#50988=CARTESIAN_POINT('Ctrl Pts',(-66.,-12.9167494409123,8.07034649661759));
#50989=CARTESIAN_POINT('Ctrl Pts',(-66.,-12.9967646908729,8.16026752634251));
#50990=CARTESIAN_POINT('Ctrl Pts',(-66.,-13.0735719476516,8.2552497632047));
#50991=CARTESIAN_POINT('Ctrl Pts',(-66.,-13.1476766619554,8.35455196515643));
#50992=CARTESIAN_POINT('Ctrl Pts',(-66.,-13.2199692944164,8.45629920475326));
#50993=CARTESIAN_POINT('Ctrl Pts',(-66.,-13.2915701735423,8.557804399923));
#50994=CARTESIAN_POINT('Ctrl Pts',(-66.,-13.3633320128944,8.65689099100683));
#50995=CARTESIAN_POINT('Ctrl Pts',(-66.,-13.4354725852278,8.7528532374933));
#50996=CARTESIAN_POINT('Ctrl Pts',(-66.,-13.5070556576137,8.84780971091874));
#50997=CARTESIAN_POINT('Ctrl Pts',(-66.,-13.5623113515642,8.92766605565115));
#50998=CARTESIAN_POINT('Ctrl Pts',(-66.,-13.6014545602526,8.99226792994578));
#50999=CARTESIAN_POINT('Ctrl Pts',(-66.,-13.626379282156,9.03800267564234));
#51000=CARTESIAN_POINT('Ctrl Pts',(-66.,-13.6386277567007,9.0617355438285));
#51001=CARTESIAN_POINT('Ctrl Pts',(-66.,-13.6388425130122,9.0621520570585));
#51002=CARTESIAN_POINT('',(-66.,-12.8416620037784,10.1603317849721));
#51003=CARTESIAN_POINT('Origin',(-66.,0.,0.));
#51004=CARTESIAN_POINT('',(-66.,-10.7151295435653,9.10713484662512));
#51005=CARTESIAN_POINT('Ctrl Pts',(-66.,-12.8416620037784,10.1603317849721));
#51006=CARTESIAN_POINT('Ctrl Pts',(-66.,-12.8317244585753,10.1582221321948));
#51007=CARTESIAN_POINT('Ctrl Pts',(-66.,-12.8007586417669,10.151590250775));
#51008=CARTESIAN_POINT('Ctrl Pts',(-66.,-12.7489015820264,10.14017641159));
#51009=CARTESIAN_POINT('Ctrl Pts',(-66.,-12.6764281187229,10.123473812926));
#51010=CARTESIAN_POINT('Ctrl Pts',(-66.,-12.5837865782488,10.1006898014275));
#51011=CARTESIAN_POINT('Ctrl Pts',(-66.,-12.4811722187999,10.0735214401623));
#51012=CARTESIAN_POINT('Ctrl Pts',(-66.,-12.3795413183411,10.0446528139577));
#51013=CARTESIAN_POINT('Ctrl Pts',(-66.,-12.2788457677249,10.0141636803616));
#51014=CARTESIAN_POINT('Ctrl Pts',(-66.,-12.179003784094,9.98217869512325));
#51015=CARTESIAN_POINT('Ctrl Pts',(-66.,-12.079951048189,9.94880133468933));
#51016=CARTESIAN_POINT('Ctrl Pts',(-66.,-11.9816885786214,9.91405212461268));
#51017=CARTESIAN_POINT('Ctrl Pts',(-66.,-11.8843251688933,9.87781397932795));
#51018=CARTESIAN_POINT('Ctrl Pts',(-66.,-11.7881404490329,9.83975072848667));
#51019=CARTESIAN_POINT('Ctrl Pts',(-66.,-11.6935310799647,9.79937782767));
#51020=CARTESIAN_POINT('Ctrl Pts',(-66.,-11.6009173880207,9.75618454891596));
#51021=CARTESIAN_POINT('Ctrl Pts',(-66.,-11.5106598224983,9.70974355202577));
#51022=CARTESIAN_POINT('Ctrl Pts',(-66.,-11.4229782872014,9.65981645609066));
#51023=CARTESIAN_POINT('Ctrl Pts',(-66.,-11.3378501911246,9.60648791406797));
#51024=CARTESIAN_POINT('Ctrl Pts',(-66.,-11.255055958553,9.55010283362399));
#51025=CARTESIAN_POINT('Ctrl Pts',(-66.,-11.1742623953034,9.49115310573639));
#51026=CARTESIAN_POINT('Ctrl Pts',(-66.,-11.0950933608815,9.43018117859799));
#51027=CARTESIAN_POINT('Ctrl Pts',(-66.,-11.0172025221741,9.36768097839366));
#51028=CARTESIAN_POINT('Ctrl Pts',(-66.,-10.9403520514449,9.30399043552504));
#51029=CARTESIAN_POINT('Ctrl Pts',(-66.,-10.8643984244951,9.23931258796881));
#51030=CARTESIAN_POINT('Ctrl Pts',(-66.,-10.8042932995341,9.18686421761339));
#51031=CARTESIAN_POINT('Ctrl Pts',(-66.,-10.7595724112169,9.14714733516059));
#51032=CARTESIAN_POINT('Ctrl Pts',(-66.,-10.7299173542433,9.1205004962881));
#51033=CARTESIAN_POINT('Ctrl Pts',(-66.,-10.7151295435653,9.10713484662511));
#51034=CARTESIAN_POINT('',(-66.,-9.76197254719673,10.1221439546065));
#51035=CARTESIAN_POINT('Origin',(-66.,0.,0.));
#51036=CARTESIAN_POINT('',(-66.,-10.9566876228483,12.1692900916743));
#51037=CARTESIAN_POINT('Ctrl Pts',(-66.,-9.76197254719673,10.1221439546065));
#51038=CARTESIAN_POINT('Ctrl Pts',(-66.,-9.77887468091545,10.1382862065996));
#51039=CARTESIAN_POINT('Ctrl Pts',(-66.,-9.8125301973609,10.1707396505663));
#51040=CARTESIAN_POINT('Ctrl Pts',(-66.,-9.86256723189823,10.2199266327873));
#51041=CARTESIAN_POINT('Ctrl Pts',(-66.,-9.92838949999087,10.2865242878363));
#51042=CARTESIAN_POINT('Ctrl Pts',(-66.,-10.0091279489326,10.371490948043));
#51043=CARTESIAN_POINT('Ctrl Pts',(-66.,-10.0881874924486,10.4582479603236));
#51044=CARTESIAN_POINT('Ctrl Pts',(-66.,-10.1653013890907,10.5469256916157));
#51045=CARTESIAN_POINT('Ctrl Pts',(-66.,-10.2400230449985,10.6377349442392));
#51046=CARTESIAN_POINT('Ctrl Pts',(-66.,-10.3117931787431,10.7309623645438));
#51047=CARTESIAN_POINT('Ctrl Pts',(-66.,-10.3800284784999,10.8269681325114));
#51048=CARTESIAN_POINT('Ctrl Pts',(-66.,-10.4442029791024,10.9261704221467));
#51049=CARTESIAN_POINT('Ctrl Pts',(-66.,-10.5039324453602,11.0290666820944));
#51050=CARTESIAN_POINT('Ctrl Pts',(-66.,-10.5590714183695,11.1360616608015));
#51051=CARTESIAN_POINT('Ctrl Pts',(-66.,-10.6098445121699,11.2471610440543));
#51052=CARTESIAN_POINT('Ctrl Pts',(-66.,-10.6569256372063,11.3617725777663));
#51053=CARTESIAN_POINT('Ctrl Pts',(-66.,-10.7016435541469,11.4783016873407));
#51054=CARTESIAN_POINT('Ctrl Pts',(-66.,-10.7457516444569,11.5944243246999));
#51055=CARTESIAN_POINT('Ctrl Pts',(-66.,-10.7906171205087,11.7082443720486));
#51056=CARTESIAN_POINT('Ctrl Pts',(-66.,-10.8366264238543,11.819132418893));
#51057=CARTESIAN_POINT('Ctrl Pts',(-66.,-10.8823458677273,11.9289076462876));
#51058=CARTESIAN_POINT('Ctrl Pts',(-66.,-10.9160061370834,12.0199966893985));
#51059=CARTESIAN_POINT('Ctrl Pts',(-66.,-10.9378537570625,12.0923034971696));
#51060=CARTESIAN_POINT('Ctrl Pts',(-66.,-10.9506216542472,12.1427999280076));
#51061=CARTESIAN_POINT('Ctrl Pts',(-66.,-10.9565831961294,12.1688332562504));
#51062=CARTESIAN_POINT('Ctrl Pts',(-66.,-10.9566876228483,12.1692900916743));
#51063=CARTESIAN_POINT('',(-66.,-9.91144581260293,13.0347177531328));
#51064=CARTESIAN_POINT('Origin',(-66.,0.,0.));
#51065=CARTESIAN_POINT('',(-66.,-8.11364170780697,11.4857618157149));
#51066=CARTESIAN_POINT('Ctrl Pts',(-66.,-9.91144581260293,13.0347177531328));
#51067=CARTESIAN_POINT('Ctrl Pts',(-66.,-9.90234512296736,13.0302030119816));
#51068=CARTESIAN_POINT('Ctrl Pts',(-66.,-9.87400143607814,13.0160785978238));
#51069=CARTESIAN_POINT('Ctrl Pts',(-66.,-9.82661206760692,12.9921270190498));
#51070=CARTESIAN_POINT('Ctrl Pts',(-66.,-9.76056925879954,12.9579257458254));
#51071=CARTESIAN_POINT('Ctrl Pts',(-66.,-9.67650437592402,12.9128185216976));
#51072=CARTESIAN_POINT('Ctrl Pts',(-66.,-9.58387033196931,12.8609845509879));
#51073=CARTESIAN_POINT('Ctrl Pts',(-66.,-9.49261168852801,12.8077483085937));
#51074=CARTESIAN_POINT('Ctrl Pts',(-66.,-9.40266201299437,12.7531750820743));
#51075=CARTESIAN_POINT('Ctrl Pts',(-66.,-9.31391109124575,12.69736527232));
#51076=CARTESIAN_POINT('Ctrl Pts',(-66.,-9.22627089118454,12.6404031093252));
#51077=CARTESIAN_POINT('Ctrl Pts',(-66.,-9.13973729492348,12.5823087271131));
#51078=CARTESIAN_POINT('Ctrl Pts',(-66.,-9.05444479601274,12.5229957744206));
#51079=CARTESIAN_POINT('Ctrl Pts',(-66.,-8.9707478415549,12.4622081834688));
#51080=CARTESIAN_POINT('Ctrl Pts',(-66.,-8.88915113193907,12.3995752782536));
#51081=CARTESIAN_POINT('Ctrl Pts',(-66.,-8.81018880105177,12.334706907179));
#51082=CARTESIAN_POINT('Ctrl Pts',(-66.,-8.73431624919877,12.2672787958196));
#51083=CARTESIAN_POINT('Ctrl Pts',(-66.,-8.66180575442286,12.1971147402934));
#51084=CARTESIAN_POINT('Ctrl Pts',(-66.,-8.59261438312223,12.1242911158748));
#51085=CARTESIAN_POINT('Ctrl Pts',(-66.,-8.52644368290816,12.0490873880617));
#51086=CARTESIAN_POINT('Ctrl Pts',(-66.,-8.46284859919381,11.9718971321485));
#51087=CARTESIAN_POINT('Ctrl Pts',(-66.,-8.40132990725019,11.8931522119833));
#51088=CARTESIAN_POINT('Ctrl Pts',(-66.,-8.34142932020866,11.8132449066089));
#51089=CARTESIAN_POINT('Ctrl Pts',(-66.,-8.28283244225497,11.732443384369));
#51090=CARTESIAN_POINT('Ctrl Pts',(-66.,-8.22534976477564,11.6509086114121));
#51091=CARTESIAN_POINT('Ctrl Pts',(-66.,-8.18017633214654,11.5851604663126));
#51092=CARTESIAN_POINT('Ctrl Pts',(-66.,-8.14673761978747,11.5355697300868));
#51093=CARTESIAN_POINT('Ctrl Pts',(-66.,-8.12464103031309,11.502385137885));
#51094=CARTESIAN_POINT('Ctrl Pts',(-66.,-8.11364170780698,11.4857618157149));
#51095=CARTESIAN_POINT('',(-66.,-6.93800739067721,12.2318420402206));
#51096=CARTESIAN_POINT('Origin',(-66.,0.,0.));
#51097=CARTESIAN_POINT('',(-66.,-7.58608375346252,14.5117868743119));
#51098=CARTESIAN_POINT('Ctrl Pts',(-66.,-6.93800739067721,12.2318420402206));
#51099=CARTESIAN_POINT('Ctrl Pts',(-66.,-6.95036409795758,12.2516805434111));
#51100=CARTESIAN_POINT('Ctrl Pts',(-66.,-6.97489142114752,12.2914841893452));
#51101=CARTESIAN_POINT('Ctrl Pts',(-66.,-7.01112414517467,12.3515695765444));
#51102=CARTESIAN_POINT('Ctrl Pts',(-66.,-7.05831632235693,12.4324442762203));
#51103=CARTESIAN_POINT('Ctrl Pts',(-66.,-7.11538787531798,12.5348203883111));
#51104=CARTESIAN_POINT('Ctrl Pts',(-66.,-7.17038802629925,12.6385130784722));
#51105=CARTESIAN_POINT('Ctrl Pts',(-66.,-7.22302599308674,12.7435822820237));
#51106=CARTESIAN_POINT('Ctrl Pts',(-66.,-7.27281678798223,12.8501211151659));
#51107=CARTESIAN_POINT('Ctrl Pts',(-66.,-7.31914741436296,12.9582681310911));
#51108=CARTESIAN_POINT('Ctrl Pts',(-66.,-7.36136331309888,13.0682271303129));
#51109=CARTESIAN_POINT('Ctrl Pts',(-66.,-7.39885104754049,13.1802723469128));
#51110=CARTESIAN_POINT('Ctrl Pts',(-66.,-7.43111474350486,13.2947900458654));
#51111=CARTESIAN_POINT('Ctrl Pts',(-66.,-7.45791285510172,13.4121360855424));
#51112=CARTESIAN_POINT('Ctrl Pts',(-66.,-7.47946152571002,13.5323718323411));
#51113=CARTESIAN_POINT('Ctrl Pts',(-66.,-7.49656078124055,13.6550912336386));
#51114=CARTESIAN_POINT('Ctrl Pts',(-66.,-7.51089419147856,13.7790802606718));
#51115=CARTESIAN_POINT('Ctrl Pts',(-66.,-7.52473801944021,13.9025239278461));
#51116=CARTESIAN_POINT('Ctrl Pts',(-66.,-7.53988806932779,14.0239256992838));
#51117=CARTESIAN_POINT('Ctrl Pts',(-66.,-7.55687516994583,14.1427720426853));
#51118=CARTESIAN_POINT('Ctrl Pts',(-66.,-7.5738582645032,14.2604684427868));
#51119=CARTESIAN_POINT('Ctrl Pts',(-66.,-7.5838081107473,14.3570667246954));
#51120=CARTESIAN_POINT('Ctrl Pts',(-66.,-7.58698737570401,14.4325351632849));
#51121=CARTESIAN_POINT('Ctrl Pts',(-66.,-7.58679619423276,14.4846204028018));
#51122=CARTESIAN_POINT('Ctrl Pts',(-66.,-7.58609621785102,14.511318421344));
#51123=CARTESIAN_POINT('Ctrl Pts',(-66.,-7.58608375346252,14.5117868743119));
#51124=CARTESIAN_POINT('',(-66.,-6.35845702927376,15.0900844665257));
#51125=CARTESIAN_POINT('Origin',(-66.,0.,0.));
#51126=CARTESIAN_POINT('',(-66.,-5.00234392366024,13.1426961282463));
#51127=CARTESIAN_POINT('Ctrl Pts',(-66.,-6.35845702927376,15.0900844665257));
#51128=CARTESIAN_POINT('Ctrl Pts',(-66.,-6.35076502500556,15.0834483147912));
#51129=CARTESIAN_POINT('Ctrl Pts',(-66.,-6.32682440612351,15.0627188567828));
#51130=CARTESIAN_POINT('Ctrl Pts',(-66.,-6.2868803772285,15.027734504202));
#51131=CARTESIAN_POINT('Ctrl Pts',(-66.,-6.23141793548312,14.9781835481972));
#51132=CARTESIAN_POINT('Ctrl Pts',(-66.,-6.16121181596629,14.913587364225));
#51133=CARTESIAN_POINT('Ctrl Pts',(-66.,-6.08437862517161,14.8403447030824));
#51134=CARTESIAN_POINT('Ctrl Pts',(-66.,-6.00922635494104,14.7660858733973));
#51135=CARTESIAN_POINT('Ctrl Pts',(-66.,-5.93567442341548,14.6908575904833));
#51136=CARTESIAN_POINT('Ctrl Pts',(-66.,-5.86359111036561,14.614729691814));
#51137=CARTESIAN_POINT('Ctrl Pts',(-66.,-5.79287020223623,14.5377618684515));
#51138=CARTESIAN_POINT('Ctrl Pts',(-66.,-5.72350270338309,14.4599725977946));
#51139=CARTESIAN_POINT('Ctrl Pts',(-66.,-5.6556403566801,14.3813116886496));
#51140=CARTESIAN_POINT('Ctrl Pts',(-66.,-5.5896901550893,14.301619265488));
#51141=CARTESIAN_POINT('Ctrl Pts',(-66.,-5.52623312628269,14.2206618116565));
#51142=CARTESIAN_POINT('Ctrl Pts',(-66.,-5.46588365010489,14.1381942665852));
#51143=CARTESIAN_POINT('Ctrl Pts',(-66.,-5.40916346339393,14.0540157969766));
#51144=CARTESIAN_POINT('Ctrl Pts',(-66.,-5.35638011020072,13.9680234475133));
#51145=CARTESIAN_POINT('Ctrl Pts',(-66.,-5.30747301200313,13.8802805168475));
#51146=CARTESIAN_POINT('Ctrl Pts',(-66.,-5.2620835925999,13.7909834684638));
#51147=CARTESIAN_POINT('Ctrl Pts',(-66.,-5.21968290141691,13.7004028321899));
#51148=CARTESIAN_POINT('Ctrl Pts',(-66.,-5.17967999761633,13.6088327519355));
#51149=CARTESIAN_POINT('Ctrl Pts',(-66.,-5.14153343642338,13.5165392112663));
#51150=CARTESIAN_POINT('Ctrl Pts',(-66.,-5.10487200859133,13.4237037664646));
#51151=CARTESIAN_POINT('Ctrl Pts',(-66.,-5.06947212861492,13.3304351977558));
#51152=CARTESIAN_POINT('Ctrl Pts',(-66.,-5.04206880122609,13.2555184756737));
#51153=CARTESIAN_POINT('Ctrl Pts',(-66.,-5.02201334210169,13.1991698540138));
#51154=CARTESIAN_POINT('Ctrl Pts',(-66.,-5.00886363010872,13.1615326184551));
#51155=CARTESIAN_POINT('Ctrl Pts',(-66.,-5.00234392366025,13.1426961282463));
#51156=CARTESIAN_POINT('',(-66.,-3.67810171359515,13.5729685048794));
#51157=CARTESIAN_POINT('Origin',(-66.,0.,0.));
#51158=CARTESIAN_POINT('',(-66.,-3.73881834218222,15.9424547170178));
#51159=CARTESIAN_POINT('Ctrl Pts',(-66.,-3.67810171359515,13.5729685048794));
#51160=CARTESIAN_POINT('Ctrl Pts',(-66.,-3.68513657707394,13.595256733151));
#51161=CARTESIAN_POINT('Ctrl Pts',(-66.,-3.69899456508718,13.6399095715909));
#51162=CARTESIAN_POINT('Ctrl Pts',(-66.,-3.71914634329887,13.7071179779119));
#51163=CARTESIAN_POINT('Ctrl Pts',(-66.,-3.7447431715177,13.7971880673979));
#51164=CARTESIAN_POINT('Ctrl Pts',(-66.,-3.77456181293102,13.910540963737));
#51165=CARTESIAN_POINT('Ctrl Pts',(-66.,-3.80204670961501,14.0246539387008));
#51166=CARTESIAN_POINT('Ctrl Pts',(-66.,-3.82690130950572,14.1395127300348));
#51167=CARTESIAN_POINT('Ctrl Pts',(-66.,-3.84863270462788,14.2550869169872));
#51168=CARTESIAN_POINT('Ctrl Pts',(-66.,-3.86661269999714,14.3713582537855));
#51169=CARTESIAN_POINT('Ctrl Pts',(-66.,-3.88015661753544,14.4883613559395));
#51170=CARTESIAN_POINT('Ctrl Pts',(-66.,-3.88860209359085,14.6062092864715));
#51171=CARTESIAN_POINT('Ctrl Pts',(-66.,-3.89137277258683,14.725152856237));
#51172=CARTESIAN_POINT('Ctrl Pts',(-66.,-3.88814619886307,14.8454766736426));
#51173=CARTESIAN_POINT('Ctrl Pts',(-66.,-3.87911646405442,14.9672939298197));
#51174=CARTESIAN_POINT('Ctrl Pts',(-66.,-3.86515944096752,15.0904102873887));
#51175=CARTESIAN_POINT('Ctrl Pts',(-66.,-3.84820772362302,15.2140685453126));
#51176=CARTESIAN_POINT('Ctrl Pts',(-66.,-3.83091743061146,15.3370768226993));
#51177=CARTESIAN_POINT('Ctrl Pts',(-66.,-3.81540012098238,15.4584321984421));
#51178=CARTESIAN_POINT('Ctrl Pts',(-66.,-3.80229765686693,15.5777692855585));
#51179=CARTESIAN_POINT('Ctrl Pts',(-66.,-3.7894772918181,15.6959915606914));
#51180=CARTESIAN_POINT('Ctrl Pts',(-66.,-3.77509152951778,15.7920294560818));
#51181=CARTESIAN_POINT('Ctrl Pts',(-66.,-3.75940267454228,15.8659175659396));
#51182=CARTESIAN_POINT('Ctrl Pts',(-66.,-3.74626442705009,15.9163189069806));
#51183=CARTESIAN_POINT('Ctrl Pts',(-66.,-3.73894691449476,15.9420040811287));
#51184=CARTESIAN_POINT('Ctrl Pts',(-66.,-3.73881834218222,15.9424547170178));
#51185=CARTESIAN_POINT('',(-66.,-2.40594300602614,16.1972856754382));
#51186=CARTESIAN_POINT('Origin',(-66.,0.,0.));
#51187=CARTESIAN_POINT('',(-66.,-1.57673047345589,13.9738265075847));
#51188=CARTESIAN_POINT('Ctrl Pts',(-66.,-2.40594300602614,16.1972856754382));
#51189=CARTESIAN_POINT('Ctrl Pts',(-66.,-2.40014300404269,16.1889450869399));
#51190=CARTESIAN_POINT('Ctrl Pts',(-66.,-2.38210973029964,16.1629130931652));
#51191=CARTESIAN_POINT('Ctrl Pts',(-66.,-2.35212087122016,16.1190941623136));
#51192=CARTESIAN_POINT('Ctrl Pts',(-66.,-2.31072370572823,16.0573069923301));
#51193=CARTESIAN_POINT('Ctrl Pts',(-66.,-2.25878765825938,15.9772806643205));
#51194=CARTESIAN_POINT('Ctrl Pts',(-66.,-2.20258303257508,15.8872314185123));
#51195=CARTESIAN_POINT('Ctrl Pts',(-66.,-2.14825922908453,15.7966159569104));
#51196=CARTESIAN_POINT('Ctrl Pts',(-66.,-2.09572657992989,15.7054594872874));
#51197=CARTESIAN_POINT('Ctrl Pts',(-66.,-2.04484013524158,15.6137968955554));
#51198=CARTESIAN_POINT('Ctrl Pts',(-66.,-1.99548217379509,15.5216595832348));
#51199=CARTESIAN_POINT('Ctrl Pts',(-66.,-1.94763938741864,15.4290632100973));
#51200=CARTESIAN_POINT('Ctrl Pts',(-66.,-1.901471233747,15.3359968987161));
#51201=CARTESIAN_POINT('Ctrl Pts',(-66.,-1.85741167873706,15.2424070113801));
#51202=CARTESIAN_POINT('Ctrl Pts',(-66.,-1.81608156923822,15.1482118634974));
#51203=CARTESIAN_POINT('Ctrl Pts',(-66.,-1.77813692730802,15.0533268835806));
#51204=CARTESIAN_POINT('Ctrl Pts',(-66.,-1.74413304367239,14.957687298555));
#51205=CARTESIAN_POINT('Ctrl Pts',(-66.,-1.71439340426661,14.8612698707291));
#51206=CARTESIAN_POINT('Ctrl Pts',(-66.,-1.68884359201954,14.7641208448459));
#51207=CARTESIAN_POINT('Ctrl Pts',(-66.,-1.66708743757887,14.6663413378531));
#51208=CARTESIAN_POINT('Ctrl Pts',(-66.,-1.64854533029309,14.5680618357278));
#51209=CARTESIAN_POINT('Ctrl Pts',(-66.,-1.63257174420173,14.4694202802978));
#51210=CARTESIAN_POINT('Ctrl Pts',(-66.,-1.61857609759037,14.3705396469258));
#51211=CARTESIAN_POINT('Ctrl Pts',(-66.,-1.60615369222193,14.2715034719842));
#51212=CARTESIAN_POINT('Ctrl Pts',(-66.,-1.59506091439902,14.1723615147133));
#51213=CARTESIAN_POINT('Ctrl Pts',(-66.,-1.58714954409268,14.0929835088213));
#51214=CARTESIAN_POINT('Ctrl Pts',(-66.,-1.58173749645856,14.0334175928621));
#51215=CARTESIAN_POINT('Ctrl Pts',(-66.,-1.57836090671277,13.9936925998767));
#51216=CARTESIAN_POINT('Ctrl Pts',(-66.,-1.57673047345591,13.9738265075847));
#51217=CARTESIAN_POINT('',(-66.,-0.187087378736033,14.0612554404903));
#51218=CARTESIAN_POINT('Origin',(-66.,0.,0.));
#51219=CARTESIAN_POINT('',(-66.,0.343370775949386,16.3713994976063));
#51220=CARTESIAN_POINT('Ctrl Pts',(-66.,-0.187087378736033,14.0612554404903));
#51221=CARTESIAN_POINT('Ctrl Pts',(-66.,-0.188358372068459,14.0845929424903));
#51222=CARTESIAN_POINT('Ctrl Pts',(-66.,-0.190676276552008,14.1312892713751));
#51223=CARTESIAN_POINT('Ctrl Pts',(-66.,-0.193480898610155,14.2013977454735));
#51224=CARTESIAN_POINT('Ctrl Pts',(-66.,-0.195874035010017,14.2950037897925));
#51225=CARTESIAN_POINT('Ctrl Pts',(-66.,-0.196566149970303,14.4122110910203));
#51226=CARTESIAN_POINT('Ctrl Pts',(-66.,-0.194808815215985,14.5295742128916));
#51227=CARTESIAN_POINT('Ctrl Pts',(-66.,-0.190318342289957,14.6470055917277));
#51228=CARTESIAN_POINT('Ctrl Pts',(-66.,-0.182624874160768,14.7643531812717));
#51229=CARTESIAN_POINT('Ctrl Pts',(-66.,-0.171124489283723,14.8814430832361));
#51230=CARTESIAN_POINT('Ctrl Pts',(-66.,-0.155145411474415,14.9981385531066));
#51231=CARTESIAN_POINT('Ctrl Pts',(-66.,-0.13401796882278,15.1143843786811));
#51232=CARTESIAN_POINT('Ctrl Pts',(-66.,-0.107121538899203,15.2302801573274));
#51233=CARTESIAN_POINT('Ctrl Pts',(-66.,-0.0740730173483893,15.3460213644938));
#51234=CARTESIAN_POINT('Ctrl Pts',(-66.,-0.035032248569878,15.4617659038311));
#51235=CARTESIAN_POINT('Ctrl Pts',(-66.,0.00910408204356977,15.5775433641354));
#51236=CARTESIAN_POINT('Ctrl Pts',(-66.,0.0562757882257695,15.6931009498213));
#51237=CARTESIAN_POINT('Ctrl Pts',(-66.,0.103613789511375,15.8079447749594));
#51238=CARTESIAN_POINT('Ctrl Pts',(-66.,0.148823449024451,15.9216285504355));
#51239=CARTESIAN_POINT('Ctrl Pts',(-66.,0.191192201865526,16.0339579931922));
#51240=CARTESIAN_POINT('Ctrl Pts',(-66.,0.233010475834533,16.1452778030188));
#51241=CARTESIAN_POINT('Ctrl Pts',(-66.,0.270827936326797,16.2347208977209));
#51242=CARTESIAN_POINT('Ctrl Pts',(-66.,0.304399122776818,16.3023860171632));
#51243=CARTESIAN_POINT('Ctrl Pts',(-66.,0.329658911880923,16.3479365581074));
#51244=CARTESIAN_POINT('Ctrl Pts',(-66.,0.343134174384058,16.3709949939062));
#51245=CARTESIAN_POINT('Ctrl Pts',(-66.,0.343370775949386,16.3713994976063));
#51246=CARTESIAN_POINT('',(-66.,1.69774526472951,16.2867518559131));
#51247=CARTESIAN_POINT('Origin',(-66.,0.,0.));
#51248=CARTESIAN_POINT('',(-66.,1.94795475120473,13.9269299753125));
#51249=CARTESIAN_POINT('Ctrl Pts',(-66.,1.69774526472951,16.2867518559131));
#51250=CARTESIAN_POINT('Ctrl Pts',(-66.,1.70128882897267,16.277230900501));
#51251=CARTESIAN_POINT('Ctrl Pts',(-66.,1.71228166066573,16.2475320568679));
#51252=CARTESIAN_POINT('Ctrl Pts',(-66.,1.73043103962239,16.1976318523256));
#51253=CARTESIAN_POINT('Ctrl Pts',(-66.,1.75516179270489,16.1274907834907));
#51254=CARTESIAN_POINT('Ctrl Pts',(-66.,1.78556443525587,16.0370626599488));
#51255=CARTESIAN_POINT('Ctrl Pts',(-66.,1.8176089524919,15.9358649547671));
#51256=CARTESIAN_POINT('Ctrl Pts',(-66.,1.84769092488014,15.8345865639611));
#51257=CARTESIAN_POINT('Ctrl Pts',(-66.,1.87590347211591,15.7332296038656));
#51258=CARTESIAN_POINT('Ctrl Pts',(-66.,1.90239566597564,15.6317918168208));
#51259=CARTESIAN_POINT('Ctrl Pts',(-66.,1.92728933849566,15.5302743417326));
#51260=CARTESIAN_POINT('Ctrl Pts',(-66.,1.95060127417394,15.4286890367845));
#51261=CARTESIAN_POINT('Ctrl Pts',(-66.,1.97217431992445,15.3270650217851));
#51262=CARTESIAN_POINT('Ctrl Pts',(-66.,1.99157480447254,15.2254582670956));
#51263=CARTESIAN_POINT('Ctrl Pts',(-66.,2.00818107188229,15.1239440527286));
#51264=CARTESIAN_POINT('Ctrl Pts',(-66.,2.02133667816179,15.022603610217));
#51265=CARTESIAN_POINT('Ctrl Pts',(-66.,2.03048766965571,14.9215122966393));
#51266=CARTESIAN_POINT('Ctrl Pts',(-66.,2.03531494435546,14.8207280520398));
#51267=CARTESIAN_POINT('Ctrl Pts',(-66.,2.03590208198289,14.7202771615244));
#51268=CARTESIAN_POINT('Ctrl Pts',(-66.,2.03265795226397,14.6201590419547));
#51269=CARTESIAN_POINT('Ctrl Pts',(-66.,2.02617640685866,14.5203559365434));
#51270=CARTESIAN_POINT('Ctrl Pts',(-66.,2.01711699607993,14.4208409176437));
#51271=CARTESIAN_POINT('Ctrl Pts',(-66.,2.00608233016073,14.3215862254212));
#51272=CARTESIAN_POINT('Ctrl Pts',(-66.,1.99348516764985,14.2225721274408));
#51273=CARTESIAN_POINT('Ctrl Pts',(-66.,1.97957384329226,14.1237862354018));
#51274=CARTESIAN_POINT('Ctrl Pts',(-66.,1.96749615602378,14.044934557742));
#51275=CARTESIAN_POINT('Ctrl Pts',(-66.,1.95792473331065,13.9858940930512));
#51276=CARTESIAN_POINT('Ctrl Pts',(-66.,1.9513160372573,13.9465774100468));
#51277=CARTESIAN_POINT('Ctrl Pts',(-66.,1.94795475120472,13.9269299753125));
#51278=CARTESIAN_POINT('',(-66.,3.31568234418832,13.6660219830951));
#51279=CARTESIAN_POINT('Origin',(-66.,0.,0.));
#51280=CARTESIAN_POINT('',(-66.,4.40398464539872,15.7716690379646));
#51281=CARTESIAN_POINT('Ctrl Pts',(-66.,3.31568234418832,13.6660219830951));
#51282=CARTESIAN_POINT('Ctrl Pts',(-66.,3.32025508218772,13.6889423777435));
#51283=CARTESIAN_POINT('Ctrl Pts',(-66.,3.32962290369722,13.7347480949923));
#51284=CARTESIAN_POINT('Ctrl Pts',(-66.,3.34434166251121,13.8033514635997));
#51285=CARTESIAN_POINT('Ctrl Pts',(-66.,3.36530258749166,13.8946118507282));
#51286=CARTESIAN_POINT('Ctrl Pts',(-66.,3.39378048711278,14.0083089910501));
#51287=CARTESIAN_POINT('Ctrl Pts',(-66.,3.42466963349977,14.1215479032503));
#51288=CARTESIAN_POINT('Ctrl Pts',(-66.,3.45822302631379,14.2341732241738));
#51289=CARTESIAN_POINT('Ctrl Pts',(-66.,3.49485794879717,14.3459208356842));
#51290=CARTESIAN_POINT('Ctrl Pts',(-66.,3.53511610244324,14.4564721136477));
#51291=CARTESIAN_POINT('Ctrl Pts',(-66.,3.57961415137445,14.5655275456869));
#51292=CARTESIAN_POINT('Ctrl Pts',(-66.,3.62898699781003,14.6728671135607));
#51293=CARTESIAN_POINT('Ctrl Pts',(-66.,3.68386053504292,14.7784329430806));
#51294=CARTESIAN_POINT('Ctrl Pts',(-66.,3.74465444426779,14.8823190942953));
#51295=CARTESIAN_POINT('Ctrl Pts',(-66.,3.81125317193191,14.9847182617076));
#51296=CARTESIAN_POINT('Ctrl Pts',(-66.,3.88279556209739,15.0858821011164));
#51297=CARTESIAN_POINT('Ctrl Pts',(-66.,3.95722328533246,15.1860781064647));
#51298=CARTESIAN_POINT('Ctrl Pts',(-66.,4.03163457417435,15.2855414194547));
#51299=CARTESIAN_POINT('Ctrl Pts',(-66.,4.10369589439471,15.3844104249513));
#51300=CARTESIAN_POINT('Ctrl Pts',(-66.,4.17266875139903,15.482674151341));
#51301=CARTESIAN_POINT('Ctrl Pts',(-66.,4.24085733833789,15.5800968628044));
#51302=CARTESIAN_POINT('Ctrl Pts',(-66.,4.29973028689649,15.6573251182294));
#51303=CARTESIAN_POINT('Ctrl Pts',(-66.,4.34907440371019,15.7145155989467));
#51304=CARTESIAN_POINT('Ctrl Pts',(-66.,4.38486856897779,15.7523532317835));
#51305=CARTESIAN_POINT('Ctrl Pts',(-66.,4.40365488112712,15.7713360829087));
#51306=CARTESIAN_POINT('Ctrl Pts',(-66.,4.40398464539872,15.7716690379646));
#51307=CARTESIAN_POINT('',(-66.,5.69475795663189,15.3528615187977));
#51308=CARTESIAN_POINT('Origin',(-66.,0.,0.));
#51309=CARTESIAN_POINT('',(-66.,5.35024281477072,13.004953213026));
#51310=CARTESIAN_POINT('Ctrl Pts',(-66.,5.69475795663189,15.3528615187977));
#51311=CARTESIAN_POINT('Ctrl Pts',(-66.,5.69582242796104,15.3427584331158));
#51312=CARTESIAN_POINT('Ctrl Pts',(-66.,5.69908409756002,15.3112588271944));
#51313=CARTESIAN_POINT('Ctrl Pts',(-66.,5.70425360416528,15.2584127623331));
#51314=CARTESIAN_POINT('Ctrl Pts',(-66.,5.71076402066882,15.1843250159624));
#51315=CARTESIAN_POINT('Ctrl Pts',(-66.,5.71772294845736,15.0891770284618));
#51316=CARTESIAN_POINT('Ctrl Pts',(-66.,5.72359388237569,14.9831894879022));
#51317=CARTESIAN_POINT('Ctrl Pts',(-66.,5.72754386270271,14.8776118616624));
#51318=CARTESIAN_POINT('Ctrl Pts',(-66.,5.72966360991829,14.772423041662));
#51319=CARTESIAN_POINT('Ctrl Pts',(-66.,5.73009695097776,14.6675837685266));
#51320=CARTESIAN_POINT('Ctrl Pts',(-66.,5.72896217357436,14.5630648469857));
#51321=CARTESIAN_POINT('Ctrl Pts',(-66.,5.72627848390049,14.4588735885414));
#51322=CARTESIAN_POINT('Ctrl Pts',(-66.,5.72190090792526,14.3550772805332));
#51323=CARTESIAN_POINT('Ctrl Pts',(-66.,5.71542331821735,14.2518379845708));
#51324=CARTESIAN_POINT('Ctrl Pts',(-66.,5.70626231068308,14.1493832151514));
#51325=CARTESIAN_POINT('Ctrl Pts',(-66.,5.6938022661864,14.0479549027521));
#51326=CARTESIAN_POINT('Ctrl Pts',(-66.,5.67752537508807,13.9477637996424));
#51327=CARTESIAN_POINT('Ctrl Pts',(-66.,5.65713696965892,13.8489453830157));
#51328=CARTESIAN_POINT('Ctrl Pts',(-66.,5.63272454065023,13.7515043267519));
#51329=CARTESIAN_POINT('Ctrl Pts',(-66.,5.60468396737303,13.6553383842666));
#51330=CARTESIAN_POINT('Ctrl Pts',(-66.,5.57358602861192,13.5602826717323));
#51331=CARTESIAN_POINT('Ctrl Pts',(-66.,5.54006285706051,13.466147083991));
#51332=CARTESIAN_POINT('Ctrl Pts',(-66.,5.50469122725311,13.3727548702637));
#51333=CARTESIAN_POINT('Ctrl Pts',(-66.,5.46786602291259,13.2799842691689));
#51334=CARTESIAN_POINT('Ctrl Pts',(-66.,5.42982469604617,13.1877615232676));
#51335=CARTESIAN_POINT('Ctrl Pts',(-66.,5.39851683671257,13.1143907147436));
#51336=CARTESIAN_POINT('Ctrl Pts',(-66.,5.37456335134248,13.0595854308535));
#51337=CARTESIAN_POINT('Ctrl Pts',(-66.,5.35838461816811,13.0231474696198));
#51338=CARTESIAN_POINT('Ctrl Pts',(-66.,5.35024281477071,13.004953213026));
#51339=CARTESIAN_POINT('',(-66.,6.61011555120064,12.4121021043889));
#51340=CARTESIAN_POINT('Origin',(-66.,0.,0.));
#51341=CARTESIAN_POINT('',(-66.,8.1878799628551,14.1809466085264));
#51342=CARTESIAN_POINT('Ctrl Pts',(-66.,6.61011555120064,12.4121021043889));
#51343=CARTESIAN_POINT('Ctrl Pts',(-66.,6.62024469858602,12.4331652189947));
#51344=CARTESIAN_POINT('Ctrl Pts',(-66.,6.64070963141069,12.4752021829311));
#51345=CARTESIAN_POINT('Ctrl Pts',(-66.,6.67202693734873,12.5379898440923));
#51346=CARTESIAN_POINT('Ctrl Pts',(-66.,6.71502487170408,12.6211703482748));
#51347=CARTESIAN_POINT('Ctrl Pts',(-66.,6.77088341473902,12.7242133182155));
#51348=CARTESIAN_POINT('Ctrl Pts',(-66.,6.82896349408885,12.8262128034276));
#51349=CARTESIAN_POINT('Ctrl Pts',(-66.,6.88947152371961,12.9269554033179));
#51350=CARTESIAN_POINT('Ctrl Pts',(-66.,6.95274599364373,13.0260815233846));
#51351=CARTESIAN_POINT('Ctrl Pts',(-66.,7.01923234820612,13.1231478339735));
#51352=CARTESIAN_POINT('Ctrl Pts',(-66.,7.08945339219251,13.2177108743086));
#51353=CARTESIAN_POINT('Ctrl Pts',(-66.,7.16396936488986,13.3093996446649));
#51354=CARTESIAN_POINT('Ctrl Pts',(-66.,7.24337210327696,13.3980024357456));
#51355=CARTESIAN_POINT('Ctrl Pts',(-66.,7.32809149527493,13.4835059820612));
#51356=CARTESIAN_POINT('Ctrl Pts',(-66.,7.41806353883254,13.5661256612623));
#51357=CARTESIAN_POINT('Ctrl Pts',(-66.,7.51251671706145,13.646319383691));
#51358=CARTESIAN_POINT('Ctrl Pts',(-66.,7.60952388977251,13.7248581251904));
#51359=CARTESIAN_POINT('Ctrl Pts',(-66.,7.70633293122716,13.8026912802767));
#51360=CARTESIAN_POINT('Ctrl Pts',(-66.,7.80071803438238,13.8805332125637));
#51361=CARTESIAN_POINT('Ctrl Pts',(-66.,7.89196117727994,13.9585569512687));
#51362=CARTESIAN_POINT('Ctrl Pts',(-66.,7.9822355374912,14.0359611371119));
#51363=CARTESIAN_POINT('Ctrl Pts',(-66.,8.05846477023863,14.0961220179458));
#51364=CARTESIAN_POINT('Ctrl Pts',(-66.,8.12048134508164,14.1392443717028));
#51365=CARTESIAN_POINT('Ctrl Pts',(-66.,8.16456080746724,14.1669916188038));
#51366=CARTESIAN_POINT('Ctrl Pts',(-66.,8.18747775617919,14.1807061229053));
#51367=CARTESIAN_POINT('Ctrl Pts',(-66.,8.1878799628551,14.1809466085264));
#51368=CARTESIAN_POINT('',(-66.,9.33394806226437,13.4542944285812));
#51369=CARTESIAN_POINT('Origin',(-66.,0.,0.));
#51370=CARTESIAN_POINT('',(-66.,8.41635544546802,11.2658274114927));
#51371=CARTESIAN_POINT('Ctrl Pts',(-66.,9.33394806226437,13.4542944285812));
#51372=CARTESIAN_POINT('Ctrl Pts',(-66.,9.33246655603105,13.4442440266596));
#51373=CARTESIAN_POINT('Ctrl Pts',(-66.,9.32779212083946,13.4129228945374));
#51374=CARTESIAN_POINT('Ctrl Pts',(-66.,9.3196569359812,13.3604514819665));
#51375=CARTESIAN_POINT('Ctrl Pts',(-66.,9.30753794249323,13.2870722636402));
#51376=CARTESIAN_POINT('Ctrl Pts',(-66.,9.29061590049322,13.1931829101653));
#51377=CARTESIAN_POINT('Ctrl Pts',(-66.,9.26994435872398,13.0890651211961));
#51378=CARTESIAN_POINT('Ctrl Pts',(-66.,9.24751415519882,12.9858220900665));
#51379=CARTESIAN_POINT('Ctrl Pts',(-66.,9.22340791088078,12.8834108105793));
#51380=CARTESIAN_POINT('Ctrl Pts',(-66.,9.19775517072751,12.7817574884561));
#51381=CARTESIAN_POINT('Ctrl Pts',(-66.,9.17066324563836,12.6808044286968));
#51382=CARTESIAN_POINT('Ctrl Pts',(-66.,9.14215255670447,12.580553936713));
#51383=CARTESIAN_POINT('Ctrl Pts',(-66.,9.11209941820162,12.4811072394643));
#51384=CARTESIAN_POINT('Ctrl Pts',(-66.,9.08015076502197,12.3827223068819));
#51385=CARTESIAN_POINT('Ctrl Pts',(-66.,9.04579810233888,12.2857645923749));
#51386=CARTESIAN_POINT('Ctrl Pts',(-66.,9.00850531748659,12.1906215239832));
#51387=CARTESIAN_POINT('Ctrl Pts',(-66.,8.96782328072592,12.0976260068268));
#51388=CARTESIAN_POINT('Ctrl Pts',(-66.,8.9235002736643,12.0069825427185));
#51389=CARTESIAN_POINT('Ctrl Pts',(-66.,8.87562220071675,11.9186739006343));
#51390=CARTESIAN_POINT('Ctrl Pts',(-66.,8.82454707622628,11.8325025950734));
#51391=CARTESIAN_POINT('Ctrl Pts',(-66.,8.77078674197194,11.7481669754252));
#51392=CARTESIAN_POINT('Ctrl Pts',(-66.,8.71490619380604,11.6653257040265));
#51393=CARTESIAN_POINT('Ctrl Pts',(-66.,8.657420129699,11.5836641450553));
#51394=CARTESIAN_POINT('Ctrl Pts',(-66.,8.59868074655117,11.5029661588994));
#51395=CARTESIAN_POINT('Ctrl Pts',(-66.,8.53889969364915,11.4231012534324));
#51396=CARTESIAN_POINT('Ctrl Pts',(-66.,8.49032885019461,11.3598214717827));
#51397=CARTESIAN_POINT('Ctrl Pts',(-66.,8.45349838774813,11.3126949862398));
#51398=CARTESIAN_POINT('Ctrl Pts',(-66.,8.4287661867593,11.2814252778905));
#51399=CARTESIAN_POINT('Ctrl Pts',(-66.,8.416355445468,11.2658274114927));
#51400=CARTESIAN_POINT('',(-66.,9.48921088782658,10.3782842019456));
#51401=CARTESIAN_POINT('Origin',(-66.,0.,0.));
#51402=CARTESIAN_POINT('',(-66.,11.4573006693292,11.699183149801));
#51403=CARTESIAN_POINT('Ctrl Pts',(-66.,9.48921088782658,10.3782842019456));
#51404=CARTESIAN_POINT('Ctrl Pts',(-66.,9.5042599930153,10.3961665635534));
#51405=CARTESIAN_POINT('Ctrl Pts',(-66.,9.53453615016101,10.4317934371322));
#51406=CARTESIAN_POINT('Ctrl Pts',(-66.,9.58048422171402,10.4848202111794));
#51407=CARTESIAN_POINT('Ctrl Pts',(-66.,9.64281744709338,10.5546942954216));
#51408=CARTESIAN_POINT('Ctrl Pts',(-66.,9.72254683584991,10.6406085262144));
#51409=CARTESIAN_POINT('Ctrl Pts',(-66.,9.80416846317344,10.7249595816546));
#51410=CARTESIAN_POINT('Ctrl Pts',(-66.,9.88782918758628,10.8074894324552));
#51411=CARTESIAN_POINT('Ctrl Pts',(-66.,9.97376743729857,10.8877656023939));
#51412=CARTESIAN_POINT('Ctrl Pts',(-66.,10.0623044106004,10.9652479123292));
#51413=CARTESIAN_POINT('Ctrl Pts',(-66.,10.1538362031934,11.0393768173572));
#51414=CARTESIAN_POINT('Ctrl Pts',(-66.,10.2488131895374,11.1096536475468));
#51415=CARTESIAN_POINT('Ctrl Pts',(-66.,10.347755963003,11.1757261609666));
#51416=CARTESIAN_POINT('Ctrl Pts',(-66.,10.4510776067987,11.237474600108));
#51417=CARTESIAN_POINT('Ctrl Pts',(-66.,10.558769691859,11.2951234927996));
#51418=CARTESIAN_POINT('Ctrl Pts',(-66.,10.6701988175887,11.3493082317362));
#51419=CARTESIAN_POINT('Ctrl Pts',(-66.,10.7836901223469,11.4012548314131));
#51420=CARTESIAN_POINT('Ctrl Pts',(-66.,10.896814048301,11.4525672852113));
#51421=CARTESIAN_POINT('Ctrl Pts',(-66.,11.0075923712357,11.5044910494005));
#51422=CARTESIAN_POINT('Ctrl Pts',(-66.,11.1153726577894,11.5573722819667));
#51423=CARTESIAN_POINT('Ctrl Pts',(-66.,11.2220605212152,11.6098943525204));
#51424=CARTESIAN_POINT('Ctrl Pts',(-66.,11.3108562751064,11.6492077293642));
#51425=CARTESIAN_POINT('Ctrl Pts',(-66.,11.3816485785003,11.6755524200814));
#51426=CARTESIAN_POINT('Ctrl Pts',(-66.,11.4312436632693,11.6914658198642));
#51427=CARTESIAN_POINT('Ctrl Pts',(-66.,11.4568512923737,11.6990502442108));
#51428=CARTESIAN_POINT('Ctrl Pts',(-66.,11.4573006693292,11.699183149801));
#51429=CARTESIAN_POINT('',(-66.,12.3866518832851,10.7103445379834));
#51430=CARTESIAN_POINT('Origin',(-66.,0.,0.));
#51431=CARTESIAN_POINT('',(-66.,10.9536375103364,8.81882824088046));
#51432=CARTESIAN_POINT('Ctrl Pts',(-66.,12.3866518832851,10.7103445379834));
#51433=CARTESIAN_POINT('Ctrl Pts',(-66.,12.3827174879745,10.7009783235375));
#51434=CARTESIAN_POINT('Ctrl Pts',(-66.,12.3704006599468,10.6718036871368));
#51435=CARTESIAN_POINT('Ctrl Pts',(-66.,12.3494719472088,10.6230038986845));
#51436=CARTESIAN_POINT('Ctrl Pts',(-66.,12.3194850246607,10.5549438945599));
#51437=CARTESIAN_POINT('Ctrl Pts',(-66.,12.2797452870059,10.4682125884904));
#51438=CARTESIAN_POINT('Ctrl Pts',(-66.,12.2338301385431,10.3725066547111));
#51439=CARTESIAN_POINT('Ctrl Pts',(-66.,12.1864291233458,10.2780853580389));
#51440=CARTESIAN_POINT('Ctrl Pts',(-66.,12.1376115714812,10.1848864963973));
#51441=CARTESIAN_POINT('Ctrl Pts',(-66.,12.0874846061232,10.0928063773702));
#51442=CARTESIAN_POINT('Ctrl Pts',(-66.,12.0361378186387,10.0017624314164));
#51443=CARTESIAN_POINT('Ctrl Pts',(-66.,11.9835915618855,9.91175181299999));
#51444=CARTESIAN_POINT('Ctrl Pts',(-66.,11.9297512100749,9.82290332823825));
#51445=CARTESIAN_POINT('Ctrl Pts',(-66.,11.8743389448017,9.73555464618448));
#51446=CARTESIAN_POINT('Ctrl Pts',(-66.,11.8169531311064,9.65018619637799));
#51447=CARTESIAN_POINT('Ctrl Pts',(-66.,11.7571708487241,9.56730656089267));
#51448=CARTESIAN_POINT('Ctrl Pts',(-66.,11.6946398682888,9.48734988004618));
#51449=CARTESIAN_POINT('Ctrl Pts',(-66.,11.629167237137,9.41057683066949));
#51450=CARTESIAN_POINT('Ctrl Pts',(-66.,11.5608318756571,9.3369493595236));
#51451=CARTESIAN_POINT('Ctrl Pts',(-66.,11.4899314378663,9.26618715093123));
#51452=CARTESIAN_POINT('Ctrl Pts',(-66.,11.4168866676366,9.19787074131628));
#51453=CARTESIAN_POINT('Ctrl Pts',(-66.,11.3421599232118,9.13152900801114));
#51454=CARTESIAN_POINT('Ctrl Pts',(-66.,11.2661714856319,9.06672919987649));
#51455=CARTESIAN_POINT('Ctrl Pts',(-66.,11.1892087351483,9.00317437991606));
#51456=CARTESIAN_POINT('Ctrl Pts',(-66.,11.1114442196238,8.9406855206164));
#51457=CARTESIAN_POINT('Ctrl Pts',(-66.,11.0486622767737,8.89147286724882));
#51458=CARTESIAN_POINT('Ctrl Pts',(-66.,11.0012690306593,8.85498631045878));
#51459=CARTESIAN_POINT('Ctrl Pts',(-66.,10.9695373770028,8.83084964577152));
#51460=CARTESIAN_POINT('Ctrl Pts',(-66.,10.9536375103364,8.81882824088047));
#51461=CARTESIAN_POINT('',(-66.,11.7720642054939,7.69236053443469));
#51462=CARTESIAN_POINT('Origin',(-66.,0.,0.));
#51463=CARTESIAN_POINT('',(-66.,14.0068170377451,8.48231698718778));
#51464=CARTESIAN_POINT('Ctrl Pts',(-66.,11.7720642054939,7.69236053443469));
#51465=CARTESIAN_POINT('Ctrl Pts',(-66.,11.7910876778603,7.70593852849788));
#51466=CARTESIAN_POINT('Ctrl Pts',(-66.,11.8292726970256,7.73291674422561));
#51467=CARTESIAN_POINT('Ctrl Pts',(-66.,11.8869644478727,7.77285076392682));
#51468=CARTESIAN_POINT('Ctrl Pts',(-66.,11.96471633848,7.82502798253687));
#51469=CARTESIAN_POINT('Ctrl Pts',(-66.,12.0633068822383,7.88841516709048));
#51470=CARTESIAN_POINT('Ctrl Pts',(-66.,12.1633414705075,7.94981770572398));
#51471=CARTESIAN_POINT('Ctrl Pts',(-66.,12.2648981787049,8.00894915338555));
#51472=CARTESIAN_POINT('Ctrl Pts',(-66.,12.3681003919172,8.06533132620399));
#51473=CARTESIAN_POINT('Ctrl Pts',(-66.,12.4731248803097,8.11836113699226));
#51474=CARTESIAN_POINT('Ctrl Pts',(-66.,12.5802161423503,8.16739811498339));
#51475=CARTESIAN_POINT('Ctrl Pts',(-66.,12.6896863889879,8.21184725330542));
#51476=CARTESIAN_POINT('Ctrl Pts',(-66.,12.8019522591891,8.25123791004828));
#51477=CARTESIAN_POINT('Ctrl Pts',(-66.,12.9173840759125,8.28535136048938));
#51478=CARTESIAN_POINT('Ctrl Pts',(-66.,13.0360295127074,8.31440717472604));
#51479=CARTESIAN_POINT('Ctrl Pts',(-66.,13.1574330841607,8.33917830374554));
#51480=CARTESIAN_POINT('Ctrl Pts',(-66.,13.2802774448963,8.36126876569594));
#51481=CARTESIAN_POINT('Ctrl Pts',(-66.,13.4026082630414,8.38283636801991));
#51482=CARTESIAN_POINT('Ctrl Pts',(-66.,13.5228191963114,8.40557940304509));
#51483=CARTESIAN_POINT('Ctrl Pts',(-66.,13.640364394729,8.42999540714673));
#51484=CARTESIAN_POINT('Ctrl Pts',(-66.,13.7567621705396,8.45433520755552));
#51485=CARTESIAN_POINT('Ctrl Pts',(-66.,13.8525450817897,8.47033087635756));
#51486=CARTESIAN_POINT('Ctrl Pts',(-66.,13.9276649729564,8.47824257022821));
#51487=CARTESIAN_POINT('Ctrl Pts',(-66.,13.9796594385348,8.481322225259));
#51488=CARTESIAN_POINT('Ctrl Pts',(-66.,14.0063487265167,8.48230001257543));
#51489=CARTESIAN_POINT('Ctrl Pts',(-66.,14.0068170377451,8.48231698718778));
#51490=CARTESIAN_POINT('',(-66.,14.66105681156,7.2934243101722));
#51491=CARTESIAN_POINT('Origin',(-66.,0.,0.));
#51492=CARTESIAN_POINT('',(-66.,12.8026622457696,5.81770965851215));
#51493=CARTESIAN_POINT('Ctrl Pts',(-66.,14.66105681156,7.2934243101722));
#51494=CARTESIAN_POINT('Ctrl Pts',(-66.,14.6549167396993,7.28533079690226));
#51495=CARTESIAN_POINT('Ctrl Pts',(-66.,14.6357314304385,7.26013580592497));
#51496=CARTESIAN_POINT('Ctrl Pts',(-66.,14.6033242178125,7.21807391177268));
#51497=CARTESIAN_POINT('Ctrl Pts',(-66.,14.5573535548322,7.15960958221619));
#51498=CARTESIAN_POINT('Ctrl Pts',(-66.,14.497293115392,7.08548597048793));
#51499=CARTESIAN_POINT('Ctrl Pts',(-66.,14.4290193778776,7.00420544769957));
#51500=CARTESIAN_POINT('Ctrl Pts',(-66.,14.3596259311217,6.92453872281182));
#51501=CARTESIAN_POINT('Ctrl Pts',(-66.,14.2891644580326,6.84640830625432));
#51502=CARTESIAN_POINT('Ctrl Pts',(-66.,14.2177129290574,6.76968712284877));
#51503=CARTESIAN_POINT('Ctrl Pts',(-66.,14.1453375866756,6.69427291666095));
#51504=CARTESIAN_POINT('Ctrl Pts',(-66.,14.0720574366665,6.62015787000295));
#51505=CARTESIAN_POINT('Ctrl Pts',(-66.,13.9978128588633,6.54749027478764));
#51506=CARTESIAN_POINT('Ctrl Pts',(-66.,13.9224187379158,6.47666628220192));
#51507=CARTESIAN_POINT('Ctrl Pts',(-66.,13.845605534933,6.40825111076043));
#51508=CARTESIAN_POINT('Ctrl Pts',(-66.,13.7670900956865,6.342842540489));
#51509=CARTESIAN_POINT('Ctrl Pts',(-66.,13.6866392230503,6.28094866827011));
#51510=CARTESIAN_POINT('Ctrl Pts',(-66.,13.6041308540151,6.22286996666888));
#51511=CARTESIAN_POINT('Ctrl Pts',(-66.,13.5196319660845,6.16854995125629));
#51512=CARTESIAN_POINT('Ctrl Pts',(-66.,13.4333611502533,6.11764308944358));
#51513=CARTESIAN_POINT('Ctrl Pts',(-66.,13.3456216156017,6.06963846112818));
#51514=CARTESIAN_POINT('Ctrl Pts',(-66.,13.2567440310958,6.02396476100794));
#51515=CARTESIAN_POINT('Ctrl Pts',(-66.,13.1670278530422,5.98009831397194));
#51516=CARTESIAN_POINT('Ctrl Pts',(-66.,13.0766775878848,5.93768004328337));
#51517=CARTESIAN_POINT('Ctrl Pts',(-66.,12.9858158402462,5.89649363499879));
#51518=CARTESIAN_POINT('Ctrl Pts',(-66.,12.9127676183656,5.86444032191588));
#51519=CARTESIAN_POINT('Ctrl Pts',(-66.,12.8577894805368,5.84088627843006));
#51520=CARTESIAN_POINT('Ctrl Pts',(-66.,12.8210521907127,5.82539925281556));
#51521=CARTESIAN_POINT('Ctrl Pts',(-66.,12.8026622457696,5.81770965851216));
#51522=CARTESIAN_POINT('',(-66.,13.3152354345065,4.52309756402217));
#51523=CARTESIAN_POINT('Origin',(-66.,0.,0.));
#51524=CARTESIAN_POINT('',(-66.,15.6762335782098,4.73247565248983));
#51525=CARTESIAN_POINT('Ctrl Pts',(-66.,13.3152354345065,4.52309756402217));
#51526=CARTESIAN_POINT('Ctrl Pts',(-66.,13.3370379593182,4.53151803523741));
#51527=CARTESIAN_POINT('Ctrl Pts',(-66.,13.3807325353144,4.54815245260096));
#51528=CARTESIAN_POINT('Ctrl Pts',(-66.,13.4465429805744,4.57248451663122));
#51529=CARTESIAN_POINT('Ctrl Pts',(-66.,13.5348280991712,4.60368638306948));
#51530=CARTESIAN_POINT('Ctrl Pts',(-66.,13.6460849914764,4.64056367145667));
#51531=CARTESIAN_POINT('Ctrl Pts',(-66.,13.7582469996088,4.67515954595839));
#51532=CARTESIAN_POINT('Ctrl Pts',(-66.,13.8713185101153,4.70717714415409));
#51533=CARTESIAN_POINT('Ctrl Pts',(-66.,13.9853001122203,4.73612262057495));
#51534=CARTESIAN_POINT('Ctrl Pts',(-66.,14.1002130408447,4.76136787417443));
#51535=CARTESIAN_POINT('Ctrl Pts',(-66.,14.2161348344847,4.78223175145606));
#51536=CARTESIAN_POINT('Ctrl Pts',(-66.,14.3332199232164,4.79806029507722));
#51537=CARTESIAN_POINT('Ctrl Pts',(-66.,14.4517548126435,4.80829403531135));
#51538=CARTESIAN_POINT('Ctrl Pts',(-66.,14.5720437967212,4.81262902350044));
#51539=CARTESIAN_POINT('Ctrl Pts',(-66.,14.6941876561096,4.81126607561379));
#51540=CARTESIAN_POINT('Ctrl Pts',(-66.,14.8179374404009,4.80506713357809));
#51541=CARTESIAN_POINT('Ctrl Pts',(-66.,14.9424160941388,4.79591343283465));
#51542=CARTESIAN_POINT('Ctrl Pts',(-66.,15.0662673092696,4.78638101191027));
#51543=CARTESIAN_POINT('Ctrl Pts',(-66.,15.1883575578327,4.77851428923771));
#51544=CARTESIAN_POINT('Ctrl Pts',(-66.,15.3082818709966,4.77293091754137));
#51545=CARTESIAN_POINT('Ctrl Pts',(-66.,15.4270758588568,4.76755908862997));
#51546=CARTESIAN_POINT('Ctrl Pts',(-66.,15.5238275348871,4.7592319826915));
#51547=CARTESIAN_POINT('Ctrl Pts',(-66.,15.598554954793,4.74821355889253));
#51548=CARTESIAN_POINT('Ctrl Pts',(-66.,15.6496817976862,4.73826596311956));
#51549=CARTESIAN_POINT('Ctrl Pts',(-66.,15.6757757584253,4.73257567543269));
#51550=CARTESIAN_POINT('Ctrl Pts',(-66.,15.6762335782098,4.73247565248983));
#51551=CARTESIAN_POINT('',(-66.,16.0142536207693,3.41823140961462));
#51552=CARTESIAN_POINT('Origin',(-66.,0.,0.));
#51553=CARTESIAN_POINT('',(-66.,13.847248627403,2.45104298226008));
#51554=CARTESIAN_POINT('Ctrl Pts',(-66.,16.0142536207693,3.41823140961462));
#51555=CARTESIAN_POINT('Ctrl Pts',(-66.,16.0062936756551,3.41191914272521));
#51556=CARTESIAN_POINT('Ctrl Pts',(-66.,15.9814453687008,3.39228689111509));
#51557=CARTESIAN_POINT('Ctrl Pts',(-66.,15.9395959205415,3.35960579476531));
#51558=CARTESIAN_POINT('Ctrl Pts',(-66.,15.8805300229522,3.31441066861968));
#51559=CARTESIAN_POINT('Ctrl Pts',(-66.,15.8039227000236,3.2575522103651));
#51560=CARTESIAN_POINT('Ctrl Pts',(-66.,15.7175802634788,3.19580425274334));
#51561=CARTESIAN_POINT('Ctrl Pts',(-66.,15.6305546306352,3.13589785295852));
#51562=CARTESIAN_POINT('Ctrl Pts',(-66.,15.542876589815,3.07774510290095));
#51563=CARTESIAN_POINT('Ctrl Pts',(-66.,15.4545900595684,3.02120352923108));
#51564=CARTESIAN_POINT('Ctrl Pts',(-66.,15.3657337712291,2.96615761473811));
#51565=CARTESIAN_POINT('Ctrl Pts',(-66.,15.2763241892947,2.9125950607961));
#51566=CARTESIAN_POINT('Ctrl Pts',(-66.,15.1863404453747,2.86067432738731));
#51567=CARTESIAN_POINT('Ctrl Pts',(-66.,15.0957017586521,2.81082515619622));
#51568=CARTESIAN_POINT('Ctrl Pts',(-66.,15.0042876224246,2.76366203995482));
#51569=CARTESIAN_POINT('Ctrl Pts',(-66.,14.9119724401214,2.71983439592332));
#51570=CARTESIAN_POINT('Ctrl Pts',(-66.,14.8186566994895,2.67989235195328));
#51571=CARTESIAN_POINT('Ctrl Pts',(-66.,14.7242968968419,2.64415729654763));
#51572=CARTESIAN_POINT('Ctrl Pts',(-66.,14.6289438583545,2.61255786321175));
#51573=CARTESIAN_POINT('Ctrl Pts',(-66.,14.5327233771235,2.58470501352874));
#51574=CARTESIAN_POINT('Ctrl Pts',(-66.,14.4358020756955,2.56002847385863));
#51575=CARTESIAN_POINT('Ctrl Pts',(-66.,14.338358156612,2.53789265347798));
#51576=CARTESIAN_POINT('Ctrl Pts',(-66.,14.2405514355047,2.51771585773738));
#51577=CARTESIAN_POINT('Ctrl Pts',(-66.,14.1424906951186,2.49909943227153));
#51578=CARTESIAN_POINT('Ctrl Pts',(-66.,14.0442408931361,2.48180336850756));
#51579=CARTESIAN_POINT('Ctrl Pts',(-66.,13.9655162806582,2.46892342325417));
#51580=CARTESIAN_POINT('Ctrl Pts',(-66.,13.9064077297103,2.45978188025048));
#51581=CARTESIAN_POINT('Ctrl Pts',(-66.,13.8669731427486,2.45391760048539));
#51582=CARTESIAN_POINT('Ctrl Pts',(-66.,13.847248627403,2.45104298226009));
#51583=CARTESIAN_POINT('',(-66.,14.0217614511585,1.06963173887291));
#51584=CARTESIAN_POINT('Origin',(-66.,0.,0.));
#51585=CARTESIAN_POINT('',(-66.,16.3606547098013,0.685275467717996));
#51586=CARTESIAN_POINT('Ctrl Pts',(-66.,14.0217614511585,1.06963173887291));
#51587=CARTESIAN_POINT('Ctrl Pts',(-66.,14.0449730955977,1.07236559806543));
#51588=CARTESIAN_POINT('Ctrl Pts',(-66.,14.0914317375174,1.07761101544474));
#51589=CARTESIAN_POINT('Ctrl Pts',(-66.,14.1612257648809,1.08481225073396));
#51590=CARTESIAN_POINT('Ctrl Pts',(-66.,14.2544968327758,1.09307823697967));
#51591=CARTESIAN_POINT('Ctrl Pts',(-66.,14.3714293939101,1.1011284935459));
#51592=CARTESIAN_POINT('Ctrl Pts',(-66.,14.4886712704316,1.10674391788617));
#51593=CARTESIAN_POINT('Ctrl Pts',(-66.,14.6061528843942,1.10963588316888));
#51594=CARTESIAN_POINT('Ctrl Pts',(-66.,14.7237519921366,1.10932591245462));
#51595=CARTESIAN_POINT('Ctrl Pts',(-66.,14.8413329590673,1.10520035673609));
#51596=CARTESIAN_POINT('Ctrl Pts',(-66.,14.9588014916819,1.09658017916666));
#51597=CARTESIAN_POINT('Ctrl Pts',(-66.,15.0761445357738,1.08279356247792));
#51598=CARTESIAN_POINT('Ctrl Pts',(-66.,15.1935004613832,1.06322736266735));
#51599=CARTESIAN_POINT('Ctrl Pts',(-66.,15.3110884135537,1.03751150535353));
#51600=CARTESIAN_POINT('Ctrl Pts',(-66.,15.4290559476364,1.00581543437186));
#51601=CARTESIAN_POINT('Ctrl Pts',(-66.,15.5473762906989,0.969035923607179));
#51602=CARTESIAN_POINT('Ctrl Pts',(-66.,15.6656677858244,0.929213220852553));
#51603=CARTESIAN_POINT('Ctrl Pts',(-66.,15.7832573706013,0.889179733744299));
#51604=CARTESIAN_POINT('Ctrl Pts',(-66.,15.8995555551237,0.851197548491309));
#51605=CARTESIAN_POINT('Ctrl Pts',(-66.,16.014323697387,0.815965624774873));
#51606=CARTESIAN_POINT('Ctrl Pts',(-66.,16.1280496341459,0.78121969830999));
#51607=CARTESIAN_POINT('Ctrl Pts',(-66.,16.2196908113235,0.749093040322084));
#51608=CARTESIAN_POINT('Ctrl Pts',(-66.,16.2893303613477,0.719836826943709));
#51609=CARTESIAN_POINT('Ctrl Pts',(-66.,16.3363770939854,0.697487024394078));
#51610=CARTESIAN_POINT('Ctrl Pts',(-66.,16.3602361479617,0.6854862034067));
#51611=CARTESIAN_POINT('Ctrl Pts',(-66.,16.3606547098013,0.685275467717996));
#51612=CARTESIAN_POINT('Origin',(-66.,0.,0.));
#51613=CARTESIAN_POINT('Ctrl Pts',(-50.,10.5997841913839,0.0676394565978705));
#51614=CARTESIAN_POINT('Ctrl Pts',(-21.,10.5997841913839,0.0676394565978705));
#51615=CARTESIAN_POINT('Ctrl Pts',(-50.,10.5813335008211,0.0524740444052774));
#51616=CARTESIAN_POINT('Ctrl Pts',(-21.,10.5813335008211,0.0524740444052774));
#51617=CARTESIAN_POINT('Ctrl Pts',(-50.,10.5443614263321,0.0223524300248218));
#51618=CARTESIAN_POINT('Ctrl Pts',(-21.,10.5443614263321,0.0223524300248218));
#51619=CARTESIAN_POINT('Ctrl Pts',(-50.,10.4886912348662,-0.0222023607441713));
#51620=CARTESIAN_POINT('Ctrl Pts',(-21.,10.4886912348662,-0.0222023607441713));
#51621=CARTESIAN_POINT('Ctrl Pts',(-50.,10.4140395862599,-0.0803518244312862));
#51622=CARTESIAN_POINT('Ctrl Pts',(-21.,10.4140395862599,-0.0803518244312862));
#51623=CARTESIAN_POINT('Ctrl Pts',(-50.,10.3200154257224,-0.150928577557962));
#51624=CARTESIAN_POINT('Ctrl Pts',(-21.,10.3200154257224,-0.150928577557962));
#51625=CARTESIAN_POINT('Ctrl Pts',(-50.,10.2252821497258,-0.21936662469166));
#51626=CARTESIAN_POINT('Ctrl Pts',(-21.,10.2252821497258,-0.21936662469166));
#51627=CARTESIAN_POINT('Ctrl Pts',(-50.,10.1298451744404,-0.285621225675487));
#51628=CARTESIAN_POINT('Ctrl Pts',(-21.,10.1298451744404,-0.285621225675487));
#51629=CARTESIAN_POINT('Ctrl Pts',(-50.,10.0337173245343,-0.349629916443317));
#51630=CARTESIAN_POINT('Ctrl Pts',(-21.,10.0337173245343,-0.349629916443317));
#51631=CARTESIAN_POINT('Ctrl Pts',(-50.,9.93692222450759,-0.411308601209036));
#51632=CARTESIAN_POINT('Ctrl Pts',(-21.,9.93692222450759,-0.411308601209036));
#51633=CARTESIAN_POINT('Ctrl Pts',(-50.,9.83949259364292,-0.470562407132084));
#51634=CARTESIAN_POINT('Ctrl Pts',(-21.,9.83949259364292,-0.470562407132084));
#51635=CARTESIAN_POINT('Ctrl Pts',(-50.,9.74146724538631,-0.527299895441833));
#51636=CARTESIAN_POINT('Ctrl Pts',(-21.,9.74146724538631,-0.527299895441833));
#51637=CARTESIAN_POINT('Ctrl Pts',(-50.,9.64288855622378,-0.581447879194613));
#51638=CARTESIAN_POINT('Ctrl Pts',(-21.,9.64288855622378,-0.581447879194613));
#51639=CARTESIAN_POINT('Ctrl Pts',(-50.,9.54380000381903,-0.632963053309266));
#51640=CARTESIAN_POINT('Ctrl Pts',(-21.,9.54380000381903,-0.632963053309266));
#51641=CARTESIAN_POINT('Ctrl Pts',(-50.,9.44424332627553,-0.681853728650741));
#51642=CARTESIAN_POINT('Ctrl Pts',(-21.,9.44424332627553,-0.681853728650741));
#51643=CARTESIAN_POINT('Ctrl Pts',(-50.,9.34425800352241,-0.728158030239757));
#51644=CARTESIAN_POINT('Ctrl Pts',(-21.,9.34425800352241,-0.728158030239757));
#51645=CARTESIAN_POINT('Ctrl Pts',(-50.,9.24388219451327,-0.771898853704204));
#51646=CARTESIAN_POINT('Ctrl Pts',(-21.,9.24388219451327,-0.771898853704204));
#51647=CARTESIAN_POINT('Ctrl Pts',(-50.,9.14315312384119,-0.813043722977556));
#51648=CARTESIAN_POINT('Ctrl Pts',(-21.,9.14315312384119,-0.813043722977556));
#51649=CARTESIAN_POINT('Ctrl Pts',(-50.,9.04210805084257,-0.851468211346448));
#51650=CARTESIAN_POINT('Ctrl Pts',(-21.,9.04210805084257,-0.851468211346448));
#51651=CARTESIAN_POINT('Ctrl Pts',(-50.,8.94078425956014,-0.886903960171006));
#51652=CARTESIAN_POINT('Ctrl Pts',(-21.,8.94078425956014,-0.886903960171006));
#51653=CARTESIAN_POINT('Ctrl Pts',(-50.,8.83922276353739,-0.91895289219465));
#51654=CARTESIAN_POINT('Ctrl Pts',(-21.,8.83922276353739,-0.91895289219465));
#51655=CARTESIAN_POINT('Ctrl Pts',(-50.,8.73747423363077,-0.947150867813171));
#51656=CARTESIAN_POINT('Ctrl Pts',(-21.,8.73747423363077,-0.947150867813171));
#51657=CARTESIAN_POINT('Ctrl Pts',(-50.,8.63560512714608,-0.971017102543952));
#51658=CARTESIAN_POINT('Ctrl Pts',(-21.,8.63560512714608,-0.971017102543952));
#51659=CARTESIAN_POINT('Ctrl Pts',(-50.,8.53370212161309,-0.990109101007578));
#51660=CARTESIAN_POINT('Ctrl Pts',(-21.,8.53370212161309,-0.990109101007578));
#51661=CARTESIAN_POINT('Ctrl Pts',(-50.,8.43188165539955,-1.00407739851957));
#51662=CARTESIAN_POINT('Ctrl Pts',(-21.,8.43188165539955,-1.00407739851957));
#51663=CARTESIAN_POINT('Ctrl Pts',(-50.,8.33027821569813,-1.01271355471894));
#51664=CARTESIAN_POINT('Ctrl Pts',(-21.,8.33027821569813,-1.01271355471894));
#51665=CARTESIAN_POINT('Ctrl Pts',(-50.,8.2290192302709,-1.01599010763451));
#51666=CARTESIAN_POINT('Ctrl Pts',(-21.,8.2290192302709,-1.01599010763451));
#51667=CARTESIAN_POINT('Ctrl Pts',(-50.,8.12820273854248,-1.01410892133532));
#51668=CARTESIAN_POINT('Ctrl Pts',(-21.,8.12820273854248,-1.01410892133532));
#51669=CARTESIAN_POINT('Ctrl Pts',(-50.,8.02787639670185,-1.00753800115478));
#51670=CARTESIAN_POINT('Ctrl Pts',(-21.,8.02787639670185,-1.00753800115478));
#51671=CARTESIAN_POINT('Ctrl Pts',(-50.,7.92800888935854,-0.997080466154163));
#51672=CARTESIAN_POINT('Ctrl Pts',(-21.,7.92800888935854,-0.997080466154163));
#51673=CARTESIAN_POINT('Ctrl Pts',(-50.,7.82850348500033,-0.983785216334556));
#51674=CARTESIAN_POINT('Ctrl Pts',(-21.,7.82850348500033,-0.983785216334556));
#51675=CARTESIAN_POINT('Ctrl Pts',(-50.,7.7292275500742,-0.968799418422936));
#51676=CARTESIAN_POINT('Ctrl Pts',(-21.,7.7292275500742,-0.968799418422936));
#51677=CARTESIAN_POINT('Ctrl Pts',(-50.,7.63003710778607,-0.953237934402832));
#51678=CARTESIAN_POINT('Ctrl Pts',(-21.,7.63003710778607,-0.953237934402832));
#51679=CARTESIAN_POINT('Ctrl Pts',(-50.,7.53080214904746,-0.938052795086853));
#51680=CARTESIAN_POINT('Ctrl Pts',(-21.,7.53080214904746,-0.938052795086853));
#51681=CARTESIAN_POINT('Ctrl Pts',(-50.,7.43143474677318,-0.923884053007732));
#51682=CARTESIAN_POINT('Ctrl Pts',(-21.,7.43143474677318,-0.923884053007732));
#51683=CARTESIAN_POINT('Ctrl Pts',(-50.,7.33188369780814,-0.9111053356665));
#51684=CARTESIAN_POINT('Ctrl Pts',(-21.,7.33188369780814,-0.9111053356665));
#51685=CARTESIAN_POINT('Ctrl Pts',(-50.,7.25207582250743,-0.902140734147995));
#51686=CARTESIAN_POINT('Ctrl Pts',(-21.,7.25207582250743,-0.902140734147995));
#51687=CARTESIAN_POINT('Ctrl Pts',(-50.,7.19212249719958,-0.896150298874621));
#51688=CARTESIAN_POINT('Ctrl Pts',(-21.,7.19212249719958,-0.896150298874621));
#51689=CARTESIAN_POINT('Ctrl Pts',(-50.,7.15211036864424,-0.892482057440589));
#51690=CARTESIAN_POINT('Ctrl Pts',(-21.,7.15211036864424,-0.892482057440589));
#51691=CARTESIAN_POINT('Ctrl Pts',(-50.,7.13209349341826,-0.890729280500493));
#51692=CARTESIAN_POINT('Ctrl Pts',(-21.,7.13209349341826,-0.890729280500493));
#51693=CARTESIAN_POINT('',(-21.5,9.99295703981581,-0.375246053138014));
#51694=CARTESIAN_POINT('Ctrl Pts',(-21.,9.47665840807863,-0.665541446186865));
#51695=CARTESIAN_POINT('Ctrl Pts',(-21.0648600646548,9.54397725881005,-0.632805485548985));
#51696=CARTESIAN_POINT('Ctrl Pts',(-21.1289204403021,9.61037774908651,-0.598586462588316));
#51697=CARTESIAN_POINT('Ctrl Pts',(-21.1924157855725,9.67606071178067,-0.562824879825102));
#51698=CARTESIAN_POINT('Ctrl Pts',(-21.2961101180279,9.78332764514829,-0.504422591651166));
#51699=CARTESIAN_POINT('Ctrl Pts',(-21.3982975032035,9.88867999737488,-0.441915547517655));
#51700=CARTESIAN_POINT('Ctrl Pts',(-21.5,9.99295703981581,-0.375246053138014));
#51701=CARTESIAN_POINT('',(-50.,7.13209349341826,-0.890729280500487));
#51702=CARTESIAN_POINT('',(-50.,7.13209349341826,-0.890729280500487));
#51703=CARTESIAN_POINT('',(-50.,9.99295703981581,-0.375246053138014));
#51704=CARTESIAN_POINT('Ctrl Pts',(-50.,7.13209349341826,-0.890729280500493));
#51705=CARTESIAN_POINT('Ctrl Pts',(-50.,7.15211036864424,-0.892482057440589));
#51706=CARTESIAN_POINT('Ctrl Pts',(-50.,7.19212249719958,-0.896150298874621));
#51707=CARTESIAN_POINT('Ctrl Pts',(-50.,7.25207582250743,-0.902140734147995));
#51708=CARTESIAN_POINT('Ctrl Pts',(-50.,7.33188369780814,-0.9111053356665));
#51709=CARTESIAN_POINT('Ctrl Pts',(-50.,7.43143474677318,-0.923884053007732));
#51710=CARTESIAN_POINT('Ctrl Pts',(-50.,7.53080214904746,-0.938052795086853));
#51711=CARTESIAN_POINT('Ctrl Pts',(-50.,7.63003710778607,-0.953237934402832));
#51712=CARTESIAN_POINT('Ctrl Pts',(-50.,7.7292275500742,-0.968799418422936));
#51713=CARTESIAN_POINT('Ctrl Pts',(-50.,7.82850348500033,-0.983785216334556));
#51714=CARTESIAN_POINT('Ctrl Pts',(-50.,7.92800888935854,-0.997080466154163));
#51715=CARTESIAN_POINT('Ctrl Pts',(-50.,8.02787639670185,-1.00753800115478));
#51716=CARTESIAN_POINT('Ctrl Pts',(-50.,8.12820273854248,-1.01410892133532));
#51717=CARTESIAN_POINT('Ctrl Pts',(-50.,8.2290192302709,-1.01599010763451));
#51718=CARTESIAN_POINT('Ctrl Pts',(-50.,8.33027821569813,-1.01271355471894));
#51719=CARTESIAN_POINT('Ctrl Pts',(-50.,8.43188165539955,-1.00407739851957));
#51720=CARTESIAN_POINT('Ctrl Pts',(-50.,8.53370212161309,-0.990109101007578));
#51721=CARTESIAN_POINT('Ctrl Pts',(-50.,8.63560512714608,-0.971017102543952));
#51722=CARTESIAN_POINT('Ctrl Pts',(-50.,8.73747423363077,-0.947150867813171));
#51723=CARTESIAN_POINT('Ctrl Pts',(-50.,8.83922276353739,-0.91895289219465));
#51724=CARTESIAN_POINT('Ctrl Pts',(-50.,8.94078425956014,-0.886903960171006));
#51725=CARTESIAN_POINT('Ctrl Pts',(-50.,9.04210805084257,-0.851468211346448));
#51726=CARTESIAN_POINT('Ctrl Pts',(-50.,9.14315312384119,-0.813043722977556));
#51727=CARTESIAN_POINT('Ctrl Pts',(-50.,9.24388219451327,-0.771898853704204));
#51728=CARTESIAN_POINT('Ctrl Pts',(-50.,9.34425800352241,-0.728158030239757));
#51729=CARTESIAN_POINT('Ctrl Pts',(-50.,9.44424332627553,-0.681853728650741));
#51730=CARTESIAN_POINT('Ctrl Pts',(-50.,9.54380000381903,-0.632963053309266));
#51731=CARTESIAN_POINT('Ctrl Pts',(-50.,9.64288855622378,-0.581447879194613));
#51732=CARTESIAN_POINT('Ctrl Pts',(-50.,9.74146724538631,-0.527299895441833));
#51733=CARTESIAN_POINT('Ctrl Pts',(-50.,9.83125393359042,-0.475330978595796));
#51734=CARTESIAN_POINT('Ctrl Pts',(-50.,9.9010538538092,-0.433097260939648));
#51735=CARTESIAN_POINT('Ctrl Pts',(-50.,9.95114599336045,-0.401850266969568));
#51736=CARTESIAN_POINT('Ctrl Pts',(-50.,9.98174010098887,-0.382417599458989));
#51737=CARTESIAN_POINT('Ctrl Pts',(-50.,9.99295703981614,-0.375246053137802));
#51738=CARTESIAN_POINT('Ctrl Pts',(-21.5,9.99295703981581,-0.375246053138015));
#51739=CARTESIAN_POINT('Ctrl Pts',(-26.3333333333333,9.99295703981581,-0.375246053138015));
#51740=CARTESIAN_POINT('Ctrl Pts',(-31.1666666666667,9.99295703981581,-0.375246053138015));
#51741=CARTESIAN_POINT('Ctrl Pts',(-40.6666666666667,9.99295703981581,-0.375246053138015));
#51742=CARTESIAN_POINT('Ctrl Pts',(-45.3333333333333,9.99295703981581,-0.375246053138014));
#51743=CARTESIAN_POINT('Ctrl Pts',(-50.,9.99295703981581,-0.375246053138014));
#51744=CARTESIAN_POINT('Origin',(-50.,0.,0.));
#51745=CARTESIAN_POINT('',(-50.,6.8122671513043,-2.29198004120026));
#51746=CARTESIAN_POINT('Origin',(-50.,0.,0.));
#51747=CARTESIAN_POINT('',(-50.,6.8122671513043,-2.29198004120026));
#51748=CARTESIAN_POINT('Ctrl Pts',(-50.,6.8122671513043,-2.29198004120026));
#51749=CARTESIAN_POINT('Ctrl Pts',(-21.,6.8122671513043,-2.29198004120026));
#51750=CARTESIAN_POINT('Ctrl Pts',(-50.,6.83461600336474,-2.30016217089616));
#51751=CARTESIAN_POINT('Ctrl Pts',(-21.,6.83461600336474,-2.30016217089616));
#51752=CARTESIAN_POINT('Ctrl Pts',(-50.,6.8793763726903,-2.31637371632821));
#51753=CARTESIAN_POINT('Ctrl Pts',(-21.,6.8793763726903,-2.31637371632821));
#51754=CARTESIAN_POINT('Ctrl Pts',(-50.,6.94670492800217,-2.3402328805745));
#51755=CARTESIAN_POINT('Ctrl Pts',(-21.,6.94670492800217,-2.3402328805745));
#51756=CARTESIAN_POINT('Ctrl Pts',(-50.,7.03685278876406,-2.37112767623027));
#51757=CARTESIAN_POINT('Ctrl Pts',(-21.,7.03685278876406,-2.37112767623027));
#51758=CARTESIAN_POINT('Ctrl Pts',(-50.,7.15012820840451,-2.4083053284885));
#51759=CARTESIAN_POINT('Ctrl Pts',(-21.,7.15012820840451,-2.4083053284885));
#51760=CARTESIAN_POINT('Ctrl Pts',(-50.,7.26387759821705,-2.44432136933076));
#51761=CARTESIAN_POINT('Ctrl Pts',(-21.,7.26387759821705,-2.44432136933076));
#51762=CARTESIAN_POINT('Ctrl Pts',(-50.,7.37786505179862,-2.47974127678492));
#51763=CARTESIAN_POINT('Ctrl Pts',(-21.,7.37786505179862,-2.47974127678492));
#51764=CARTESIAN_POINT('Ctrl Pts',(-50.,7.49168859641892,-2.51552733857386));
#51765=CARTESIAN_POINT('Ctrl Pts',(-21.,7.49168859641892,-2.51552733857386));
#51766=CARTESIAN_POINT('Ctrl Pts',(-50.,7.60482241577417,-2.55297760756074));
#51767=CARTESIAN_POINT('Ctrl Pts',(-21.,7.60482241577417,-2.55297760756074));
#51768=CARTESIAN_POINT('Ctrl Pts',(-50.,7.71666617412861,-2.59365833862295));
#51769=CARTESIAN_POINT('Ctrl Pts',(-21.,7.71666617412861,-2.59365833862295));
#51770=CARTESIAN_POINT('Ctrl Pts',(-50.,7.82659266808561,-2.63932460382938));
#51771=CARTESIAN_POINT('Ctrl Pts',(-21.,7.82659266808561,-2.63932460382938));
#51772=CARTESIAN_POINT('Ctrl Pts',(-50.,7.93399262158453,-2.69188736687836));
#51773=CARTESIAN_POINT('Ctrl Pts',(-21.,7.93399262158453,-2.69188736687836));
#51774=CARTESIAN_POINT('Ctrl Pts',(-50.,8.03835937937461,-2.75296659957235));
#51775=CARTESIAN_POINT('Ctrl Pts',(-21.,8.03835937937461,-2.75296659957235));
#51776=CARTESIAN_POINT('Ctrl Pts',(-50.,8.13939365460193,-2.82329483425037));
#51777=CARTESIAN_POINT('Ctrl Pts',(-21.,8.13939365460193,-2.82329483425037));
#51778=CARTESIAN_POINT('Ctrl Pts',(-50.,8.2370828133169,-2.90227874531213));
#51779=CARTESIAN_POINT('Ctrl Pts',(-21.,8.2370828133169,-2.90227874531213));
#51780=CARTESIAN_POINT('Ctrl Pts',(-50.,8.33184183835821,-2.98721060740199));
#51781=CARTESIAN_POINT('Ctrl Pts',(-21.,8.33184183835821,-2.98721060740199));
#51782=CARTESIAN_POINT('Ctrl Pts',(-50.,8.4243384303954,-3.07426635319921));
#51783=CARTESIAN_POINT('Ctrl Pts',(-21.,8.4243384303954,-3.07426635319921));
#51784=CARTESIAN_POINT('Ctrl Pts',(-50.,8.51516539363766,-3.16038325236223));
#51785=CARTESIAN_POINT('Ctrl Pts',(-21.,8.51516539363766,-3.16038325236223));
#51786=CARTESIAN_POINT('Ctrl Pts',(-50.,8.60460841273967,-3.24456764186082));
#51787=CARTESIAN_POINT('Ctrl Pts',(-21.,8.60460841273967,-3.24456764186082));
#51788=CARTESIAN_POINT('Ctrl Pts',(-50.,8.69226485417113,-3.33012809006974));
#51789=CARTESIAN_POINT('Ctrl Pts',(-21.,8.69226485417113,-3.33012809006974));
#51790=CARTESIAN_POINT('Ctrl Pts',(-50.,8.77716058006919,-3.42378642402312));
#51791=CARTESIAN_POINT('Ctrl Pts',(-21.,8.77716058006919,-3.42378642402312));
#51792=CARTESIAN_POINT('Ctrl Pts',(-50.,8.85834857876282,-3.53174964938136));
#51793=CARTESIAN_POINT('Ctrl Pts',(-21.,8.85834857876282,-3.53174964938136));
#51794=CARTESIAN_POINT('Ctrl Pts',(-50.,8.93534116084886,-3.65684682750522));
#51795=CARTESIAN_POINT('Ctrl Pts',(-21.,8.93534116084886,-3.65684682750522));
#51796=CARTESIAN_POINT('Ctrl Pts',(-50.,9.0086889241718,-3.79469796977264));
#51797=CARTESIAN_POINT('Ctrl Pts',(-21.,9.0086889241718,-3.79469796977264));
#51798=CARTESIAN_POINT('Ctrl Pts',(-50.,9.08026462895257,-3.93186755639596));
#51799=CARTESIAN_POINT('Ctrl Pts',(-21.,9.08026462895257,-3.93186755639596));
#51800=CARTESIAN_POINT('Ctrl Pts',(-50.,9.15270492381554,-4.04971509082727));
#51801=CARTESIAN_POINT('Ctrl Pts',(-21.,9.15270492381554,-4.04971509082727));
#51802=CARTESIAN_POINT('Ctrl Pts',(-50.,9.22899343053301,-4.12729029694314));
#51803=CARTESIAN_POINT('Ctrl Pts',(-21.,9.22899343053301,-4.12729029694314));
#51804=CARTESIAN_POINT('Ctrl Pts',(-50.,9.31200173345042,-4.1445121148068));
#51805=CARTESIAN_POINT('Ctrl Pts',(-21.,9.31200173345042,-4.1445121148068));
#51806=CARTESIAN_POINT('Ctrl Pts',(-50.,9.4040191976898,-4.08543198173291));
#51807=CARTESIAN_POINT('Ctrl Pts',(-21.,9.4040191976898,-4.08543198173291));
#51808=CARTESIAN_POINT('Ctrl Pts',(-50.,9.50679569557631,-3.93791789477537));
#51809=CARTESIAN_POINT('Ctrl Pts',(-21.,9.50679569557631,-3.93791789477537));
#51810=CARTESIAN_POINT('Ctrl Pts',(-50.,9.6216277792442,-3.69303758521427));
#51811=CARTESIAN_POINT('Ctrl Pts',(-21.,9.6216277792442,-3.69303758521427));
#51812=CARTESIAN_POINT('Ctrl Pts',(-50.,9.74942513377921,-3.34458014605708));
#51813=CARTESIAN_POINT('Ctrl Pts',(-21.,9.74942513377921,-3.34458014605708));
#51814=CARTESIAN_POINT('Ctrl Pts',(-50.,9.89078169235227,-2.88854649339194));
#51815=CARTESIAN_POINT('Ctrl Pts',(-21.,9.89078169235227,-2.88854649339194));
#51816=CARTESIAN_POINT('Ctrl Pts',(-50.,10.0460413192499,-2.32267878361756));
#51817=CARTESIAN_POINT('Ctrl Pts',(-21.,10.0460413192499,-2.32267878361756));
#51818=CARTESIAN_POINT('Ctrl Pts',(-50.,10.2153627041086,-1.64599643173284));
#51819=CARTESIAN_POINT('Ctrl Pts',(-21.,10.2153627041086,-1.64599643173284));
#51820=CARTESIAN_POINT('Ctrl Pts',(-50.,10.3620979683038,-1.01587958589522));
#51821=CARTESIAN_POINT('Ctrl Pts',(-21.,10.3620979683038,-1.01587958589522));
#51822=CARTESIAN_POINT('Ctrl Pts',(-50.,10.478481770919,-0.493469650218984));
#51823=CARTESIAN_POINT('Ctrl Pts',(-21.,10.478481770919,-0.493469650218984));
#51824=CARTESIAN_POINT('Ctrl Pts',(-50.,10.5588816113278,-0.123082548500186));
#51825=CARTESIAN_POINT('Ctrl Pts',(-21.,10.5588816113278,-0.123082548500186));
#51826=CARTESIAN_POINT('Ctrl Pts',(-50.,10.5997841913839,0.0676394565978705));
#51827=CARTESIAN_POINT('Ctrl Pts',(-21.,10.5997841913839,0.0676394565978705));
#51828=CARTESIAN_POINT('',(-21.5,9.14990386923577,-4.03475639707582));
#51829=CARTESIAN_POINT('Ctrl Pts',(-21.5,9.14990386923577,-4.03475639707581));
#51830=CARTESIAN_POINT('Ctrl Pts',(-21.4716714037531,9.13031726529337,-4.00896291438969));
#51831=CARTESIAN_POINT('Ctrl Pts',(-21.4424150110748,9.11133064989716,-3.97941274406063));
#51832=CARTESIAN_POINT('Ctrl Pts',(-21.2909879716453,9.01605057347099,-3.81864524910466));
#51833=CARTESIAN_POINT('Ctrl Pts',(-21.1630186724944,8.94508544457216,-3.65653131387786));
#51834=CARTESIAN_POINT('Ctrl Pts',(-21.,8.83189477299562,-3.49966208636385));
#51835=CARTESIAN_POINT('',(-50.,9.14990386923577,-4.03475639707582));
#51836=CARTESIAN_POINT('Ctrl Pts',(-50.,9.14990386923578,-4.03475639707582));
#51837=CARTESIAN_POINT('Ctrl Pts',(-45.1666666666667,9.14990386923578,-4.03475639707582));
#51838=CARTESIAN_POINT('Ctrl Pts',(-40.3333333333333,9.14990386923578,-4.03475639707582));
#51839=CARTESIAN_POINT('Ctrl Pts',(-30.8333333333333,9.14990386923578,-4.03475639707582));
#51840=CARTESIAN_POINT('Ctrl Pts',(-26.1666666666667,9.14990386923578,-4.03475639707582));
#51841=CARTESIAN_POINT('Ctrl Pts',(-21.5,9.14990386923578,-4.03475639707582));
#51842=CARTESIAN_POINT('Ctrl Pts',(-50.,9.14990386923577,-4.03475639707581));
#51843=CARTESIAN_POINT('Ctrl Pts',(-50.,9.13577160343033,-4.01614569996669));
#51844=CARTESIAN_POINT('Ctrl Pts',(-50.,9.10709633384263,-3.97431669461607));
#51845=CARTESIAN_POINT('Ctrl Pts',(-50.,9.06450371311672,-3.90166326358648));
#51846=CARTESIAN_POINT('Ctrl Pts',(-50.,9.00794825534563,-3.79330594308901));
#51847=CARTESIAN_POINT('Ctrl Pts',(-50.,8.93534116084886,-3.65684682750522));
#51848=CARTESIAN_POINT('Ctrl Pts',(-50.,8.85834857876282,-3.53174964938136));
#51849=CARTESIAN_POINT('Ctrl Pts',(-50.,8.77716058006919,-3.42378642402312));
#51850=CARTESIAN_POINT('Ctrl Pts',(-50.,8.69226485417113,-3.33012809006974));
#51851=CARTESIAN_POINT('Ctrl Pts',(-50.,8.60460841273967,-3.24456764186082));
#51852=CARTESIAN_POINT('Ctrl Pts',(-50.,8.51516539363766,-3.16038325236223));
#51853=CARTESIAN_POINT('Ctrl Pts',(-50.,8.4243384303954,-3.07426635319921));
#51854=CARTESIAN_POINT('Ctrl Pts',(-50.,8.33184183835821,-2.98721060740199));
#51855=CARTESIAN_POINT('Ctrl Pts',(-50.,8.2370828133169,-2.90227874531213));
#51856=CARTESIAN_POINT('Ctrl Pts',(-50.,8.13939365460193,-2.82329483425037));
#51857=CARTESIAN_POINT('Ctrl Pts',(-50.,8.03835937937461,-2.75296659957235));
#51858=CARTESIAN_POINT('Ctrl Pts',(-50.,7.93399262158453,-2.69188736687836));
#51859=CARTESIAN_POINT('Ctrl Pts',(-50.,7.82659266808561,-2.63932460382938));
#51860=CARTESIAN_POINT('Ctrl Pts',(-50.,7.71666617412861,-2.59365833862295));
#51861=CARTESIAN_POINT('Ctrl Pts',(-50.,7.60482241577417,-2.55297760756074));
#51862=CARTESIAN_POINT('Ctrl Pts',(-50.,7.49168859641892,-2.51552733857386));
#51863=CARTESIAN_POINT('Ctrl Pts',(-50.,7.37786505179862,-2.47974127678492));
#51864=CARTESIAN_POINT('Ctrl Pts',(-50.,7.26387759821705,-2.44432136933076));
#51865=CARTESIAN_POINT('Ctrl Pts',(-50.,7.15012820840451,-2.4083053284885));
#51866=CARTESIAN_POINT('Ctrl Pts',(-50.,7.03685278876406,-2.37112767623027));
#51867=CARTESIAN_POINT('Ctrl Pts',(-50.,6.94670492800217,-2.3402328805745));
#51868=CARTESIAN_POINT('Ctrl Pts',(-50.,6.8793763726903,-2.31637371632821));
#51869=CARTESIAN_POINT('Ctrl Pts',(-50.,6.83461600336474,-2.30016217089616));
#51870=CARTESIAN_POINT('Ctrl Pts',(-50.,6.8122671513043,-2.29198004120026));
#51871=CARTESIAN_POINT('Origin',(-21.25,0.,0.));
#51872=CARTESIAN_POINT('',(-21.5,9.99439372247306,0.334804600014791));
#51873=CARTESIAN_POINT('Origin',(-21.5,0.,0.));
#51874=CARTESIAN_POINT('Ctrl Pts',(-21.5,9.99439372247306,0.334804600014791));
#51875=CARTESIAN_POINT('Ctrl Pts',(-21.4716714037526,9.96555542937976,0.349545415954904));
#51876=CARTESIAN_POINT('Ctrl Pts',(-21.4424150110737,9.93562774160641,0.367931215781723));
#51877=CARTESIAN_POINT('Ctrl Pts',(-21.2909879716438,9.78002895717459,0.471437247885104));
#51878=CARTESIAN_POINT('Ctrl Pts',(-21.1630186724941,9.64575298495204,0.586706241102918));
#51879=CARTESIAN_POINT('Ctrl Pts',(-21.,9.47570870673866,0.678928939607903));
#51880=CARTESIAN_POINT('Origin',(-35.75,0.,0.));
#51881=CARTESIAN_POINT('',(-50.,9.99439372247306,0.334804600014791));
#51882=CARTESIAN_POINT('Origin',(-50.,0.,0.));
#51883=CARTESIAN_POINT('Ctrl Pts',(-50.,9.99439372247306,0.334804600014792));
#51884=CARTESIAN_POINT('Ctrl Pts',(-45.1666666666667,9.99439372247306,0.334804600014792));
#51885=CARTESIAN_POINT('Ctrl Pts',(-40.3333333333333,9.99439372247306,0.334804600014792));
#51886=CARTESIAN_POINT('Ctrl Pts',(-30.8333333333333,9.99439372247306,0.334804600014792));
#51887=CARTESIAN_POINT('Ctrl Pts',(-26.1666666666667,9.99439372247306,0.334804600014792));
#51888=CARTESIAN_POINT('Ctrl Pts',(-21.5,9.99439372247306,0.334804600014792));
#51889=CARTESIAN_POINT('Ctrl Pts',(-50.,5.14318775290069,-5.02073460645076));
#51890=CARTESIAN_POINT('Ctrl Pts',(-21.,5.14318775290069,-5.02073460645076));
#51891=CARTESIAN_POINT('Ctrl Pts',(-50.,5.1597732798141,-5.03780325407688));
#51892=CARTESIAN_POINT('Ctrl Pts',(-21.,5.1597732798141,-5.03780325407688));
#51893=CARTESIAN_POINT('Ctrl Pts',(-50.,5.19306705314332,-5.071830148219));
#51894=CARTESIAN_POINT('Ctrl Pts',(-21.,5.19306705314332,-5.071830148219));
#51895=CARTESIAN_POINT('Ctrl Pts',(-50.,5.24337588200475,-5.12253927774717));
#51896=CARTESIAN_POINT('Ctrl Pts',(-21.,5.24337588200475,-5.12253927774717));
#51897=CARTESIAN_POINT('Ctrl Pts',(-50.,5.31119154860082,-5.18948821771405));
#51898=CARTESIAN_POINT('Ctrl Pts',(-21.,5.31119154860082,-5.18948821771405));
#51899=CARTESIAN_POINT('Ctrl Pts',(-50.,5.39711839642203,-5.27213248760413));
#51900=CARTESIAN_POINT('Ctrl Pts',(-21.,5.39711839642203,-5.27213248760413));
#51901=CARTESIAN_POINT('Ctrl Pts',(-50.,5.48397628091718,-5.35393582972231));
#51902=CARTESIAN_POINT('Ctrl Pts',(-21.,5.48397628091718,-5.35393582972231));
#51903=CARTESIAN_POINT('Ctrl Pts',(-50.,5.57130730604024,-5.43530536621495));
#51904=CARTESIAN_POINT('Ctrl Pts',(-21.,5.57130730604024,-5.43530536621495));
#51905=CARTESIAN_POINT('Ctrl Pts',(-50.,5.65833178588016,-5.51693367893109));
#51906=CARTESIAN_POINT('Ctrl Pts',(-21.,5.65833178588016,-5.51693367893109));
#51907=CARTESIAN_POINT('Ctrl Pts',(-50.,5.74401277228714,-5.59976212994534));
#51908=CARTESIAN_POINT('Ctrl Pts',(-21.,5.74401277228714,-5.59976212994534));
#51909=CARTESIAN_POINT('Ctrl Pts',(-50.,5.82712980893039,-5.68494139022769));
#51910=CARTESIAN_POINT('Ctrl Pts',(-21.,5.82712980893039,-5.68494139022769));
#51911=CARTESIAN_POINT('Ctrl Pts',(-50.,5.906356307844,-5.77378059171821));
#51912=CARTESIAN_POINT('Ctrl Pts',(-21.,5.906356307844,-5.77378059171821));
#51913=CARTESIAN_POINT('Ctrl Pts',(-50.,5.98031419419066,-5.86773709824143));
#51914=CARTESIAN_POINT('Ctrl Pts',(-21.,5.98031419419066,-5.86773709824143));
#51915=CARTESIAN_POINT('Ctrl Pts',(-50.,6.04784410793973,-5.96805062448362));
#51916=CARTESIAN_POINT('Ctrl Pts',(-21.,6.04784410793973,-5.96805062448362));
#51917=CARTESIAN_POINT('Ctrl Pts',(-50.,6.108358567083,-6.07525130357771));
#51918=CARTESIAN_POINT('Ctrl Pts',(-21.,6.108358567083,-6.07525130357771));
#51919=CARTESIAN_POINT('Ctrl Pts',(-50.,6.16210362315516,-6.18879908596403));
#51920=CARTESIAN_POINT('Ctrl Pts',(-21.,6.16210362315516,-6.18879908596403));
#51921=CARTESIAN_POINT('Ctrl Pts',(-50.,6.2106280007764,-6.30643444970003));
#51922=CARTESIAN_POINT('Ctrl Pts',(-21.,6.2106280007764,-6.30643444970003));
#51923=CARTESIAN_POINT('Ctrl Pts',(-50.,6.25619247809081,-6.42500173364409));
#51924=CARTESIAN_POINT('Ctrl Pts',(-21.,6.25619247809081,-6.42500173364409));
#51925=CARTESIAN_POINT('Ctrl Pts',(-50.,6.30066002212815,-6.5419987212145));
#51926=CARTESIAN_POINT('Ctrl Pts',(-21.,6.30066002212815,-6.5419987212145));
#51927=CARTESIAN_POINT('Ctrl Pts',(-50.,6.34471916009928,-6.65665410688205));
#51928=CARTESIAN_POINT('Ctrl Pts',(-21.,6.34471916009928,-6.65665410688205));
#51929=CARTESIAN_POINT('Ctrl Pts',(-50.,6.38657159771068,-6.77177411160809));
#51930=CARTESIAN_POINT('Ctrl Pts',(-21.,6.38657159771068,-6.77177411160809));
#51931=CARTESIAN_POINT('Ctrl Pts',(-50.,6.42242317562759,-6.89299222970744));
#51932=CARTESIAN_POINT('Ctrl Pts',(-21.,6.42242317562759,-6.89299222970744));
#51933=CARTESIAN_POINT('Ctrl Pts',(-50.,6.44872754699223,-7.02548988707821));
#51934=CARTESIAN_POINT('Ctrl Pts',(-21.,6.44872754699223,-7.02548988707821));
#51935=CARTESIAN_POINT('Ctrl Pts',(-50.,6.46381783511374,-7.17160437943005));
#51936=CARTESIAN_POINT('Ctrl Pts',(-21.,6.46381783511374,-7.17160437943005));
#51937=CARTESIAN_POINT('Ctrl Pts',(-50.,6.47009051734937,-7.32762836882426));
#51938=CARTESIAN_POINT('Ctrl Pts',(-21.,6.47009051734937,-7.32762836882426));
#51939=CARTESIAN_POINT('Ctrl Pts',(-50.,6.47506234591768,-7.48226943041517));
#51940=CARTESIAN_POINT('Ctrl Pts',(-21.,6.47506234591768,-7.48226943041517));
#51941=CARTESIAN_POINT('Ctrl Pts',(-50.,6.48919666748604,-7.61987705609476));
#51942=CARTESIAN_POINT('Ctrl Pts',(-21.,6.48919666748604,-7.61987705609476));
#51943=CARTESIAN_POINT('Ctrl Pts',(-50.,6.52427161652488,-7.72287024427254));
#51944=CARTESIAN_POINT('Ctrl Pts',(-21.,6.52427161652488,-7.72287024427254));
#51945=CARTESIAN_POINT('Ctrl Pts',(-50.,6.59158724650179,-7.774402518864));
#51946=CARTESIAN_POINT('Ctrl Pts',(-21.,6.59158724650179,-7.774402518864));
#51947=CARTESIAN_POINT('Ctrl Pts',(-50.,6.70012602613047,-7.76109803970118));
#51948=CARTESIAN_POINT('Ctrl Pts',(-21.,6.70012602613047,-7.76109803970118));
#51949=CARTESIAN_POINT('Ctrl Pts',(-50.,6.8567284146999,-7.67278549097179));
#51950=CARTESIAN_POINT('Ctrl Pts',(-21.,6.8567284146999,-7.67278549097179));
#51951=CARTESIAN_POINT('Ctrl Pts',(-50.,7.06643813146967,-7.50197972952742));
#51952=CARTESIAN_POINT('Ctrl Pts',(-21.,7.06643813146967,-7.50197972952742));
#51953=CARTESIAN_POINT('Ctrl Pts',(-50.,7.33276958593085,-7.24347961909277));
#51954=CARTESIAN_POINT('Ctrl Pts',(-21.,7.33276958593085,-7.24347961909277));
#51955=CARTESIAN_POINT('Ctrl Pts',(-50.,7.65799303086079,-6.89393980750813));
#51956=CARTESIAN_POINT('Ctrl Pts',(-21.,7.65799303086079,-6.89393980750813));
#51957=CARTESIAN_POINT('Ctrl Pts',(-50.,8.04339791890053,-6.45147524510253));
#51958=CARTESIAN_POINT('Ctrl Pts',(-21.,8.04339791890053,-6.45147524510253));
#51959=CARTESIAN_POINT('Ctrl Pts',(-50.,8.48955268435888,-5.91527130817043));
#51960=CARTESIAN_POINT('Ctrl Pts',(-21.,8.48955268435888,-5.91527130817043));
#51961=CARTESIAN_POINT('Ctrl Pts',(-50.,8.89515404237518,-5.41122169201928));
#51962=CARTESIAN_POINT('Ctrl Pts',(-21.,8.89515404237518,-5.41122169201928));
#51963=CARTESIAN_POINT('Ctrl Pts',(-50.,9.22667740150299,-4.99104364314351));
#51964=CARTESIAN_POINT('Ctrl Pts',(-21.,9.22667740150299,-4.99104364314351));
#51965=CARTESIAN_POINT('Ctrl Pts',(-50.,9.45982009531033,-4.69222057880331));
#51966=CARTESIAN_POINT('Ctrl Pts',(-21.,9.45982009531033,-4.69222057880331));
#51967=CARTESIAN_POINT('Ctrl Pts',(-50.,9.57942322326164,-4.53813295416029));
#51968=CARTESIAN_POINT('Ctrl Pts',(-21.,9.57942322326164,-4.53813295416029));
#51969=CARTESIAN_POINT('',(-50.,6.49316333848958,-7.60518440668567));
#51970=CARTESIAN_POINT('',(-21.5,6.49316333848958,-7.60518440668567));
#51971=CARTESIAN_POINT('Ctrl Pts',(-50.,6.49316333848958,-7.60518440668567));
#51972=CARTESIAN_POINT('Ctrl Pts',(-45.1666666666667,6.49316333848958,-7.60518440668567));
#51973=CARTESIAN_POINT('Ctrl Pts',(-40.3333333333333,6.49316333848958,-7.60518440668567));
#51974=CARTESIAN_POINT('Ctrl Pts',(-30.8333333333333,6.49316333848958,-7.60518440668567));
#51975=CARTESIAN_POINT('Ctrl Pts',(-26.1666666666667,6.49316333848958,-7.60518440668567));
#51976=CARTESIAN_POINT('Ctrl Pts',(-21.5,6.49316333848958,-7.60518440668567));
#51977=CARTESIAN_POINT('',(-50.,5.14318775290069,-5.02073460645076));
#51978=CARTESIAN_POINT('Ctrl Pts',(-50.,6.49316333848958,-7.60518440668567));
#51979=CARTESIAN_POINT('Ctrl Pts',(-50.,6.48850548581524,-7.58228498765052));
#51980=CARTESIAN_POINT('Ctrl Pts',(-50.,6.48081888588311,-7.53215662286537));
#51981=CARTESIAN_POINT('Ctrl Pts',(-50.,6.47396740292153,-7.44821789782204));
#51982=CARTESIAN_POINT('Ctrl Pts',(-50.,6.47002717553801,-7.32605283195927));
#51983=CARTESIAN_POINT('Ctrl Pts',(-50.,6.46381783511374,-7.17160437943005));
#51984=CARTESIAN_POINT('Ctrl Pts',(-50.,6.44872754699223,-7.02548988707821));
#51985=CARTESIAN_POINT('Ctrl Pts',(-50.,6.42242317562759,-6.89299222970744));
#51986=CARTESIAN_POINT('Ctrl Pts',(-50.,6.38657159771068,-6.77177411160809));
#51987=CARTESIAN_POINT('Ctrl Pts',(-50.,6.34471916009928,-6.65665410688205));
#51988=CARTESIAN_POINT('Ctrl Pts',(-50.,6.30066002212815,-6.5419987212145));
#51989=CARTESIAN_POINT('Ctrl Pts',(-50.,6.25619247809081,-6.42500173364409));
#51990=CARTESIAN_POINT('Ctrl Pts',(-50.,6.2106280007764,-6.30643444970003));
#51991=CARTESIAN_POINT('Ctrl Pts',(-50.,6.16210362315516,-6.18879908596403));
#51992=CARTESIAN_POINT('Ctrl Pts',(-50.,6.108358567083,-6.07525130357771));
#51993=CARTESIAN_POINT('Ctrl Pts',(-50.,6.04784410793973,-5.96805062448362));
#51994=CARTESIAN_POINT('Ctrl Pts',(-50.,5.98031419419066,-5.86773709824143));
#51995=CARTESIAN_POINT('Ctrl Pts',(-50.,5.906356307844,-5.77378059171821));
#51996=CARTESIAN_POINT('Ctrl Pts',(-50.,5.82712980893039,-5.68494139022769));
#51997=CARTESIAN_POINT('Ctrl Pts',(-50.,5.74401277228714,-5.59976212994534));
#51998=CARTESIAN_POINT('Ctrl Pts',(-50.,5.65833178588016,-5.51693367893109));
#51999=CARTESIAN_POINT('Ctrl Pts',(-50.,5.57130730604024,-5.43530536621495));
#52000=CARTESIAN_POINT('Ctrl Pts',(-50.,5.48397628091718,-5.35393582972231));
#52001=CARTESIAN_POINT('Ctrl Pts',(-50.,5.39711839642203,-5.27213248760413));
#52002=CARTESIAN_POINT('Ctrl Pts',(-50.,5.31119154860082,-5.18948821771405));
#52003=CARTESIAN_POINT('Ctrl Pts',(-50.,5.24337588200475,-5.12253927774717));
#52004=CARTESIAN_POINT('Ctrl Pts',(-50.,5.19306705314332,-5.071830148219));
#52005=CARTESIAN_POINT('Ctrl Pts',(-50.,5.1597732798141,-5.03780325407688));
#52006=CARTESIAN_POINT('Ctrl Pts',(-50.,5.14318775290069,-5.02073460645076));
#52007=CARTESIAN_POINT('',(-50.,5.14318775290069,-5.02073460645076));
#52008=CARTESIAN_POINT('Ctrl Pts',(-21.5,6.49316333848958,-7.60518440668567));
#52009=CARTESIAN_POINT('Ctrl Pts',(-21.4716714037525,6.4867077908221,-7.57344697283478));
#52010=CARTESIAN_POINT('Ctrl Pts',(-21.4424150110734,6.48242277983716,-7.53858520564487));
#52011=CARTESIAN_POINT('Ctrl Pts',(-21.2909879716434,6.46633279908612,-7.35239822189483));
#52012=CARTESIAN_POINT('Ctrl Pts',(-21.1630186724938,6.47273402762071,-7.17554799773058));
#52013=CARTESIAN_POINT('Ctrl Pts',(-21.,6.43881576337965,-6.98510211559241));
#52014=CARTESIAN_POINT('Origin',(-50.,0.,0.));
#52015=CARTESIAN_POINT('',(-50.,6.03932124977422,-3.89701874412038));
#52016=CARTESIAN_POINT('Origin',(-50.,0.,0.));
#52017=CARTESIAN_POINT('',(-50.,6.03932124977422,-3.89701874412038));
#52018=CARTESIAN_POINT('Ctrl Pts',(-50.,9.57942322326164,-4.53813295416029));
#52019=CARTESIAN_POINT('Ctrl Pts',(-21.,9.57942322326164,-4.53813295416029));
#52020=CARTESIAN_POINT('Ctrl Pts',(-50.,9.55621969972587,-4.54379106380403));
#52021=CARTESIAN_POINT('Ctrl Pts',(-21.,9.55621969972587,-4.54379106380403));
#52022=CARTESIAN_POINT('Ctrl Pts',(-50.,9.50983973295391,-4.55488811868959));
#52023=CARTESIAN_POINT('Ctrl Pts',(-21.,9.50983973295391,-4.55488811868959));
#52024=CARTESIAN_POINT('Ctrl Pts',(-50.,9.44035102435851,-4.57087620725774));
#52025=CARTESIAN_POINT('Ctrl Pts',(-21.,9.44035102435851,-4.57087620725774));
#52026=CARTESIAN_POINT('Ctrl Pts',(-50.,9.34786210629442,-4.59087692729648));
#52027=CARTESIAN_POINT('Ctrl Pts',(-21.,9.34786210629442,-4.59087692729648));
#52028=CARTESIAN_POINT('Ctrl Pts',(-50.,9.23252715927802,-4.61366883031981));
#52029=CARTESIAN_POINT('Ctrl Pts',(-21.,9.23252715927802,-4.61366883031981));
#52030=CARTESIAN_POINT('Ctrl Pts',(-50.,9.11748127106242,-4.63422615215906));
#52031=CARTESIAN_POINT('Ctrl Pts',(-21.,9.11748127106242,-4.63422615215906));
#52032=CARTESIAN_POINT('Ctrl Pts',(-50.,9.00274873347492,-4.65251093331389));
#52033=CARTESIAN_POINT('Ctrl Pts',(-21.,9.00274873347492,-4.65251093331389));
#52034=CARTESIAN_POINT('Ctrl Pts',(-50.,8.8883682032848,-4.66847246002033));
#52035=CARTESIAN_POINT('Ctrl Pts',(-21.,8.8883682032848,-4.66847246002033));
#52036=CARTESIAN_POINT('Ctrl Pts',(-50.,8.7743974532252,-4.68204521487955));
#52037=CARTESIAN_POINT('Ctrl Pts',(-21.,8.7743974532252,-4.68204521487955));
#52038=CARTESIAN_POINT('Ctrl Pts',(-50.,8.66090712613407,-4.69315791678054));
#52039=CARTESIAN_POINT('Ctrl Pts',(-21.,8.66090712613407,-4.69315791678054));
#52040=CARTESIAN_POINT('Ctrl Pts',(-50.,8.5479718655136,-4.70174502276072));
#52041=CARTESIAN_POINT('Ctrl Pts',(-21.,8.5479718655136,-4.70174502276072));
#52042=CARTESIAN_POINT('Ctrl Pts',(-50.,8.4356616058832,-4.70775898013052));
#52043=CARTESIAN_POINT('Ctrl Pts',(-21.,8.4356616058832,-4.70775898013052));
#52044=CARTESIAN_POINT('Ctrl Pts',(-50.,8.32403430863484,-4.71117963661127));
#52045=CARTESIAN_POINT('Ctrl Pts',(-21.,8.32403430863484,-4.71117963661127));
#52046=CARTESIAN_POINT('Ctrl Pts',(-50.,8.21312397255121,-4.71203258951797));
#52047=CARTESIAN_POINT('Ctrl Pts',(-21.,8.21312397255121,-4.71203258951797));
#52048=CARTESIAN_POINT('Ctrl Pts',(-50.,8.1029496259928,-4.71036931800664));
#52049=CARTESIAN_POINT('Ctrl Pts',(-21.,8.1029496259928,-4.71036931800664));
#52050=CARTESIAN_POINT('Ctrl Pts',(-50.,7.99353571494822,-4.70622700687469));
#52051=CARTESIAN_POINT('Ctrl Pts',(-21.,7.99353571494822,-4.70622700687469));
#52052=CARTESIAN_POINT('Ctrl Pts',(-50.,7.8849298684541,-4.69959254734285));
#52053=CARTESIAN_POINT('Ctrl Pts',(-21.,7.8849298684541,-4.69959254734285));
#52054=CARTESIAN_POINT('Ctrl Pts',(-50.,7.77721964274024,-4.69037000103626));
#52055=CARTESIAN_POINT('Ctrl Pts',(-21.,7.77721964274024,-4.69037000103626));
#52056=CARTESIAN_POINT('Ctrl Pts',(-50.,7.6705550660185,-4.67833376211481));
#52057=CARTESIAN_POINT('Ctrl Pts',(-21.,7.6705550660185,-4.67833376211481));
#52058=CARTESIAN_POINT('Ctrl Pts',(-50.,7.56514580946327,-4.66314297047291));
#52059=CARTESIAN_POINT('Ctrl Pts',(-21.,7.56514580946327,-4.66314297047291));
#52060=CARTESIAN_POINT('Ctrl Pts',(-50.,7.46123890856565,-4.64440143603747));
#52061=CARTESIAN_POINT('Ctrl Pts',(-21.,7.46123890856565,-4.64440143603747));
#52062=CARTESIAN_POINT('Ctrl Pts',(-50.,7.35910284385827,-4.62170482170181));
#52063=CARTESIAN_POINT('Ctrl Pts',(-21.,7.35910284385827,-4.62170482170181));
#52064=CARTESIAN_POINT('Ctrl Pts',(-50.,7.25900770064673,-4.59469206087561));
#52065=CARTESIAN_POINT('Ctrl Pts',(-21.,7.25900770064673,-4.59469206087561));
#52066=CARTESIAN_POINT('Ctrl Pts',(-50.,7.16121001331941,-4.56309881747208));
#52067=CARTESIAN_POINT('Ctrl Pts',(-21.,7.16121001331941,-4.56309881747208));
#52068=CARTESIAN_POINT('Ctrl Pts',(-50.,7.06592138953324,-4.5267956450212));
#52069=CARTESIAN_POINT('Ctrl Pts',(-21.,7.06592138953324,-4.5267956450212));
#52070=CARTESIAN_POINT('Ctrl Pts',(-50.,6.9732685530375,-4.48581308997575));
#52071=CARTESIAN_POINT('Ctrl Pts',(-21.,6.9732685530375,-4.48581308997575));
#52072=CARTESIAN_POINT('Ctrl Pts',(-50.,6.88325224876452,-4.44037556328962));
#52073=CARTESIAN_POINT('Ctrl Pts',(-21.,6.88325224876452,-4.44037556328962));
#52074=CARTESIAN_POINT('Ctrl Pts',(-50.,6.79571235355295,-4.39092540044368));
#52075=CARTESIAN_POINT('Ctrl Pts',(-21.,6.79571235355295,-4.39092540044368));
#52076=CARTESIAN_POINT('Ctrl Pts',(-50.,6.71027219290963,-4.33817259947066));
#52077=CARTESIAN_POINT('Ctrl Pts',(-21.,6.71027219290963,-4.33817259947066));
#52078=CARTESIAN_POINT('Ctrl Pts',(-50.,6.62638951409907,-4.28302021638686));
#52079=CARTESIAN_POINT('Ctrl Pts',(-21.,6.62638951409907,-4.28302021638686));
#52080=CARTESIAN_POINT('Ctrl Pts',(-50.,6.54344708143028,-4.22644426515767));
#52081=CARTESIAN_POINT('Ctrl Pts',(-21.,6.54344708143028,-4.22644426515767));
#52082=CARTESIAN_POINT('Ctrl Pts',(-50.,6.46083145580807,-4.1693867325325));
#52083=CARTESIAN_POINT('Ctrl Pts',(-21.,6.46083145580807,-4.1693867325325));
#52084=CARTESIAN_POINT('Ctrl Pts',(-50.,6.37801243240243,-4.11264895980536));
#52085=CARTESIAN_POINT('Ctrl Pts',(-21.,6.37801243240243,-4.11264895980536));
#52086=CARTESIAN_POINT('Ctrl Pts',(-50.,6.29463308326085,-4.05676946424956));
#52087=CARTESIAN_POINT('Ctrl Pts',(-21.,6.29463308326085,-4.05676946424956));
#52088=CARTESIAN_POINT('Ctrl Pts',(-50.,6.21048516503746,-4.00206265639536));
#52089=CARTESIAN_POINT('Ctrl Pts',(-21.,6.21048516503746,-4.00206265639536));
#52090=CARTESIAN_POINT('Ctrl Pts',(-50.,6.14247034880463,-3.95935849016754));
#52091=CARTESIAN_POINT('Ctrl Pts',(-21.,6.14247034880463,-3.95935849016754));
#52092=CARTESIAN_POINT('Ctrl Pts',(-50.,6.09105342163039,-3.92794852152395));
#52093=CARTESIAN_POINT('Ctrl Pts',(-21.,6.09105342163039,-3.92794852152395));
#52094=CARTESIAN_POINT('Ctrl Pts',(-50.,6.0565953297729,-3.90728293824429));
#52095=CARTESIAN_POINT('Ctrl Pts',(-21.,6.0565953297729,-3.90728293824429));
#52096=CARTESIAN_POINT('Ctrl Pts',(-50.,6.03932124977421,-3.89701874412039));
#52097=CARTESIAN_POINT('Ctrl Pts',(-21.,6.03932124977421,-3.89701874412039));
#52098=CARTESIAN_POINT('',(-21.5,8.84053003053573,-4.67386657695702));
#52099=CARTESIAN_POINT('',(-50.,8.84053003053573,-4.67386657695701));
#52100=CARTESIAN_POINT('Ctrl Pts',(-21.5,8.84053003053573,-4.67386657695702));
#52101=CARTESIAN_POINT('Ctrl Pts',(-26.3333333333333,8.84053003053573,-4.67386657695702));
#52102=CARTESIAN_POINT('Ctrl Pts',(-31.1666666666667,8.84053003053573,-4.67386657695702));
#52103=CARTESIAN_POINT('Ctrl Pts',(-40.6666666666667,8.84053003053573,-4.67386657695702));
#52104=CARTESIAN_POINT('Ctrl Pts',(-45.3333333333333,8.84053003053573,-4.67386657695702));
#52105=CARTESIAN_POINT('Ctrl Pts',(-50.,8.84053003053573,-4.67386657695702));
#52106=CARTESIAN_POINT('Ctrl Pts',(-21.,8.24940658621528,-4.71140010775012));
#52107=CARTESIAN_POINT('Ctrl Pts',(-21.1171767611032,8.38464171183386,-4.71088427266306));
#52108=CARTESIAN_POINT('Ctrl Pts',(-21.2874825276494,8.58376433439636,-4.70484095794145));
#52109=CARTESIAN_POINT('Ctrl Pts',(-21.5,8.84053003053573,-4.67386657695702));
#52110=CARTESIAN_POINT('Ctrl Pts',(-50.,6.03932124977421,-3.89701874412039));
#52111=CARTESIAN_POINT('Ctrl Pts',(-50.,6.0565953297729,-3.90728293824429));
#52112=CARTESIAN_POINT('Ctrl Pts',(-50.,6.09105342163039,-3.92794852152395));
#52113=CARTESIAN_POINT('Ctrl Pts',(-50.,6.14247034880463,-3.95935849016754));
#52114=CARTESIAN_POINT('Ctrl Pts',(-50.,6.21048516503746,-4.00206265639536));
#52115=CARTESIAN_POINT('Ctrl Pts',(-50.,6.29463308326085,-4.05676946424956));
#52116=CARTESIAN_POINT('Ctrl Pts',(-50.,6.37801243240243,-4.11264895980536));
#52117=CARTESIAN_POINT('Ctrl Pts',(-50.,6.46083145580807,-4.1693867325325));
#52118=CARTESIAN_POINT('Ctrl Pts',(-50.,6.54344708143028,-4.22644426515767));
#52119=CARTESIAN_POINT('Ctrl Pts',(-50.,6.62638951409907,-4.28302021638686));
#52120=CARTESIAN_POINT('Ctrl Pts',(-50.,6.71027219290963,-4.33817259947066));
#52121=CARTESIAN_POINT('Ctrl Pts',(-50.,6.79571235355295,-4.39092540044368));
#52122=CARTESIAN_POINT('Ctrl Pts',(-50.,6.88325224876452,-4.44037556328962));
#52123=CARTESIAN_POINT('Ctrl Pts',(-50.,6.9732685530375,-4.48581308997575));
#52124=CARTESIAN_POINT('Ctrl Pts',(-50.,7.06592138953324,-4.5267956450212));
#52125=CARTESIAN_POINT('Ctrl Pts',(-50.,7.16121001331941,-4.56309881747208));
#52126=CARTESIAN_POINT('Ctrl Pts',(-50.,7.25900770064673,-4.59469206087561));
#52127=CARTESIAN_POINT('Ctrl Pts',(-50.,7.35910284385827,-4.62170482170181));
#52128=CARTESIAN_POINT('Ctrl Pts',(-50.,7.46123890856565,-4.64440143603747));
#52129=CARTESIAN_POINT('Ctrl Pts',(-50.,7.56514580946327,-4.66314297047291));
#52130=CARTESIAN_POINT('Ctrl Pts',(-50.,7.6705550660185,-4.67833376211481));
#52131=CARTESIAN_POINT('Ctrl Pts',(-50.,7.77721964274024,-4.69037000103626));
#52132=CARTESIAN_POINT('Ctrl Pts',(-50.,7.8849298684541,-4.69959254734285));
#52133=CARTESIAN_POINT('Ctrl Pts',(-50.,7.99353571494822,-4.70622700687469));
#52134=CARTESIAN_POINT('Ctrl Pts',(-50.,8.1029496259928,-4.71036931800664));
#52135=CARTESIAN_POINT('Ctrl Pts',(-50.,8.21312397255121,-4.71203258951797));
#52136=CARTESIAN_POINT('Ctrl Pts',(-50.,8.32403430863484,-4.71117963661127));
#52137=CARTESIAN_POINT('Ctrl Pts',(-50.,8.4356616058832,-4.70775898013052));
#52138=CARTESIAN_POINT('Ctrl Pts',(-50.,8.5479718655136,-4.70174502276072));
#52139=CARTESIAN_POINT('Ctrl Pts',(-50.,8.65141534429653,-4.69387963058482));
#52140=CARTESIAN_POINT('Ctrl Pts',(-50.,8.73262742272914,-4.68611341617549));
#52141=CARTESIAN_POINT('Ctrl Pts',(-50.,8.79131644357128,-4.67969501220182));
#52142=CARTESIAN_POINT('Ctrl Pts',(-50.,8.82731230052618,-4.67546106956729));
#52143=CARTESIAN_POINT('Ctrl Pts',(-50.,8.84053003053573,-4.67386657695701));
#52144=CARTESIAN_POINT('Origin',(-50.,10.,0.));
#52145=CARTESIAN_POINT('',(-50.,14.0217614511585,-1.06963173887292));
#52146=CARTESIAN_POINT('',(-50.,16.3612159786808,-0.671741541784792));
#52147=CARTESIAN_POINT('Ctrl Pts',(-50.,14.0217614511585,-1.06963173887291));
#52148=CARTESIAN_POINT('Ctrl Pts',(-50.,14.0415811730659,-1.0717527195609));
#52149=CARTESIAN_POINT('Ctrl Pts',(-50.,14.0812352370361,-1.07587965991017));
#52150=CARTESIAN_POINT('Ctrl Pts',(-50.,14.1407601934611,-1.08172501415579));
#52151=CARTESIAN_POINT('Ctrl Pts',(-50.,14.2202146396052,-1.08882773106131));
#52152=CARTESIAN_POINT('Ctrl Pts',(-50.,14.3196790995356,-1.09650878711472));
#52153=CARTESIAN_POINT('Ctrl Pts',(-50.,14.4192887981899,-1.10286394535002));
#52154=CARTESIAN_POINT('Ctrl Pts',(-50.,14.5190405063557,-1.10764458318629));
#52155=CARTESIAN_POINT('Ctrl Pts',(-50.,14.6189280002071,-1.11043751754959));
#52156=CARTESIAN_POINT('Ctrl Pts',(-50.,14.7189411465911,-1.11063958426619));
#52157=CARTESIAN_POINT('Ctrl Pts',(-50.,14.8190654065121,-1.10759084369408));
#52158=CARTESIAN_POINT('Ctrl Pts',(-50.,14.9192812134642,-1.100697501046));
#52159=CARTESIAN_POINT('Ctrl Pts',(-50.,15.0195634762927,-1.08955145679141));
#52160=CARTESIAN_POINT('Ctrl Pts',(-50.,15.1198807137451,-1.07407094658941));
#52161=CARTESIAN_POINT('Ctrl Pts',(-50.,15.2201951366894,-1.05457808085916));
#52162=CARTESIAN_POINT('Ctrl Pts',(-50.,15.3204663197849,-1.03163045186508));
#52163=CARTESIAN_POINT('Ctrl Pts',(-50.,15.42065441025,-1.00588830882699));
#52164=CARTESIAN_POINT('Ctrl Pts',(-50.,15.5207233107191,-0.977976807855906));
#52165=CARTESIAN_POINT('Ctrl Pts',(-50.,15.6206443917204,-0.948332278883351));
#52166=CARTESIAN_POINT('Ctrl Pts',(-50.,15.7203984586304,-0.917113393337539));
#52167=CARTESIAN_POINT('Ctrl Pts',(-50.,15.8199726227578,-0.884304144422378));
#52168=CARTESIAN_POINT('Ctrl Pts',(-50.,15.9193580975472,-0.849783012021725));
#52169=CARTESIAN_POINT('Ctrl Pts',(-50.,16.018547775909,-0.813401076758624));
#52170=CARTESIAN_POINT('Ctrl Pts',(-50.,16.1175336986507,-0.775065535573949));
#52171=CARTESIAN_POINT('Ctrl Pts',(-50.,16.2058743852262,-0.739044856835963));
#52172=CARTESIAN_POINT('Ctrl Pts',(-50.,16.2743241898497,-0.709958710092983));
#52173=CARTESIAN_POINT('Ctrl Pts',(-50.,16.322986318803,-0.688711885022031));
#52174=CARTESIAN_POINT('Ctrl Pts',(-50.,16.3519363129391,-0.675875939350104));
#52175=CARTESIAN_POINT('Ctrl Pts',(-50.,16.3612159786808,-0.671741541784792));
#52176=CARTESIAN_POINT('',(-50.,16.3606547098013,0.685275467717997));
#52177=CARTESIAN_POINT('Origin',(-50.,0.,0.));
#52178=CARTESIAN_POINT('',(-50.,14.0217614511585,1.06963173887291));
#52179=CARTESIAN_POINT('Ctrl Pts',(-50.,16.3606547098013,0.685275467717997));
#52180=CARTESIAN_POINT('Ctrl Pts',(-50.,16.3602361479617,0.685486203406702));
#52181=CARTESIAN_POINT('Ctrl Pts',(-50.,16.3363770939854,0.697487024394078));
#52182=CARTESIAN_POINT('Ctrl Pts',(-50.,16.2893303613477,0.719836826943709));
#52183=CARTESIAN_POINT('Ctrl Pts',(-50.,16.2196908113235,0.749093040322084));
#52184=CARTESIAN_POINT('Ctrl Pts',(-50.,16.1280496341459,0.78121969830999));
#52185=CARTESIAN_POINT('Ctrl Pts',(-50.,16.014323697387,0.815965624774873));
#52186=CARTESIAN_POINT('Ctrl Pts',(-50.,15.8995555551237,0.851197548491309));
#52187=CARTESIAN_POINT('Ctrl Pts',(-50.,15.7832573706013,0.889179733744299));
#52188=CARTESIAN_POINT('Ctrl Pts',(-50.,15.6656677858244,0.929213220852553));
#52189=CARTESIAN_POINT('Ctrl Pts',(-50.,15.5473762906989,0.969035923607179));
#52190=CARTESIAN_POINT('Ctrl Pts',(-50.,15.4290559476364,1.00581543437186));
#52191=CARTESIAN_POINT('Ctrl Pts',(-50.,15.3110884135537,1.03751150535353));
#52192=CARTESIAN_POINT('Ctrl Pts',(-50.,15.1935004613832,1.06322736266735));
#52193=CARTESIAN_POINT('Ctrl Pts',(-50.,15.0761445357738,1.08279356247792));
#52194=CARTESIAN_POINT('Ctrl Pts',(-50.,14.9588014916819,1.09658017916666));
#52195=CARTESIAN_POINT('Ctrl Pts',(-50.,14.8413329590673,1.10520035673609));
#52196=CARTESIAN_POINT('Ctrl Pts',(-50.,14.7237519921366,1.10932591245462));
#52197=CARTESIAN_POINT('Ctrl Pts',(-50.,14.6061528843942,1.10963588316888));
#52198=CARTESIAN_POINT('Ctrl Pts',(-50.,14.4886712704316,1.10674391788617));
#52199=CARTESIAN_POINT('Ctrl Pts',(-50.,14.3714293939101,1.1011284935459));
#52200=CARTESIAN_POINT('Ctrl Pts',(-50.,14.2544968327758,1.09307823697967));
#52201=CARTESIAN_POINT('Ctrl Pts',(-50.,14.1612257648809,1.08481225073396));
#52202=CARTESIAN_POINT('Ctrl Pts',(-50.,14.0914317375174,1.07761101544474));
#52203=CARTESIAN_POINT('Ctrl Pts',(-50.,14.0449730955977,1.07236559806543));
#52204=CARTESIAN_POINT('Ctrl Pts',(-50.,14.0217614511585,1.06963173887291));
#52205=CARTESIAN_POINT('',(-50.,13.847248627403,2.45104298226008));
#52206=CARTESIAN_POINT('Origin',(-50.,0.,0.));
#52207=CARTESIAN_POINT('',(-50.,16.0142536207693,3.41823140961461));
#52208=CARTESIAN_POINT('Ctrl Pts',(-50.,13.847248627403,2.45104298226009));
#52209=CARTESIAN_POINT('Ctrl Pts',(-50.,13.8669731427486,2.45391760048539));
#52210=CARTESIAN_POINT('Ctrl Pts',(-50.,13.9064077297103,2.45978188025048));
#52211=CARTESIAN_POINT('Ctrl Pts',(-50.,13.9655162806582,2.46892342325417));
#52212=CARTESIAN_POINT('Ctrl Pts',(-50.,14.0442408931361,2.48180336850756));
#52213=CARTESIAN_POINT('Ctrl Pts',(-50.,14.1424906951186,2.49909943227153));
#52214=CARTESIAN_POINT('Ctrl Pts',(-50.,14.2405514355047,2.51771585773738));
#52215=CARTESIAN_POINT('Ctrl Pts',(-50.,14.338358156612,2.53789265347798));
#52216=CARTESIAN_POINT('Ctrl Pts',(-50.,14.4358020756955,2.56002847385863));
#52217=CARTESIAN_POINT('Ctrl Pts',(-50.,14.5327233771235,2.58470501352874));
#52218=CARTESIAN_POINT('Ctrl Pts',(-50.,14.6289438583545,2.61255786321175));
#52219=CARTESIAN_POINT('Ctrl Pts',(-50.,14.7242968968419,2.64415729654763));
#52220=CARTESIAN_POINT('Ctrl Pts',(-50.,14.8186566994895,2.67989235195328));
#52221=CARTESIAN_POINT('Ctrl Pts',(-50.,14.9119724401214,2.71983439592332));
#52222=CARTESIAN_POINT('Ctrl Pts',(-50.,15.0042876224246,2.76366203995482));
#52223=CARTESIAN_POINT('Ctrl Pts',(-50.,15.0957017586521,2.81082515619622));
#52224=CARTESIAN_POINT('Ctrl Pts',(-50.,15.1863404453747,2.86067432738731));
#52225=CARTESIAN_POINT('Ctrl Pts',(-50.,15.2763241892947,2.9125950607961));
#52226=CARTESIAN_POINT('Ctrl Pts',(-50.,15.3657337712291,2.96615761473811));
#52227=CARTESIAN_POINT('Ctrl Pts',(-50.,15.4545900595684,3.02120352923108));
#52228=CARTESIAN_POINT('Ctrl Pts',(-50.,15.542876589815,3.07774510290095));
#52229=CARTESIAN_POINT('Ctrl Pts',(-50.,15.6305546306352,3.13589785295852));
#52230=CARTESIAN_POINT('Ctrl Pts',(-50.,15.7175802634788,3.19580425274334));
#52231=CARTESIAN_POINT('Ctrl Pts',(-50.,15.8039227000236,3.2575522103651));
#52232=CARTESIAN_POINT('Ctrl Pts',(-50.,15.8805300229522,3.31441066861968));
#52233=CARTESIAN_POINT('Ctrl Pts',(-50.,15.9395959205415,3.35960579476531));
#52234=CARTESIAN_POINT('Ctrl Pts',(-50.,15.9814453687008,3.39228689111509));
#52235=CARTESIAN_POINT('Ctrl Pts',(-50.,16.0062936756551,3.41191914272521));
#52236=CARTESIAN_POINT('Ctrl Pts',(-50.,16.0142536207693,3.41823140961461));
#52237=CARTESIAN_POINT('',(-50.,15.6762335782097,4.73247565248984));
#52238=CARTESIAN_POINT('Origin',(-50.,0.,0.));
#52239=CARTESIAN_POINT('',(-50.,13.3152354345065,4.52309756402217));
#52240=CARTESIAN_POINT('Ctrl Pts',(-50.,15.6762335782097,4.73247565248984));
#52241=CARTESIAN_POINT('Ctrl Pts',(-50.,15.6757757584253,4.73257567543269));
#52242=CARTESIAN_POINT('Ctrl Pts',(-50.,15.6496817976862,4.73826596311956));
#52243=CARTESIAN_POINT('Ctrl Pts',(-50.,15.598554954793,4.74821355889253));
#52244=CARTESIAN_POINT('Ctrl Pts',(-50.,15.5238275348871,4.7592319826915));
#52245=CARTESIAN_POINT('Ctrl Pts',(-50.,15.4270758588568,4.76755908862997));
#52246=CARTESIAN_POINT('Ctrl Pts',(-50.,15.3082818709966,4.77293091754137));
#52247=CARTESIAN_POINT('Ctrl Pts',(-50.,15.1883575578327,4.77851428923771));
#52248=CARTESIAN_POINT('Ctrl Pts',(-50.,15.0662673092696,4.78638101191027));
#52249=CARTESIAN_POINT('Ctrl Pts',(-50.,14.9424160941388,4.79591343283465));
#52250=CARTESIAN_POINT('Ctrl Pts',(-50.,14.8179374404009,4.80506713357809));
#52251=CARTESIAN_POINT('Ctrl Pts',(-50.,14.6941876561096,4.81126607561379));
#52252=CARTESIAN_POINT('Ctrl Pts',(-50.,14.5720437967212,4.81262902350044));
#52253=CARTESIAN_POINT('Ctrl Pts',(-50.,14.4517548126435,4.80829403531135));
#52254=CARTESIAN_POINT('Ctrl Pts',(-50.,14.3332199232164,4.79806029507722));
#52255=CARTESIAN_POINT('Ctrl Pts',(-50.,14.2161348344847,4.78223175145606));
#52256=CARTESIAN_POINT('Ctrl Pts',(-50.,14.1002130408447,4.76136787417443));
#52257=CARTESIAN_POINT('Ctrl Pts',(-50.,13.9853001122203,4.73612262057495));
#52258=CARTESIAN_POINT('Ctrl Pts',(-50.,13.8713185101153,4.70717714415409));
#52259=CARTESIAN_POINT('Ctrl Pts',(-50.,13.7582469996088,4.67515954595839));
#52260=CARTESIAN_POINT('Ctrl Pts',(-50.,13.6460849914764,4.64056367145667));
#52261=CARTESIAN_POINT('Ctrl Pts',(-50.,13.5348280991712,4.60368638306948));
#52262=CARTESIAN_POINT('Ctrl Pts',(-50.,13.4465429805744,4.57248451663122));
#52263=CARTESIAN_POINT('Ctrl Pts',(-50.,13.3807325353144,4.54815245260096));
#52264=CARTESIAN_POINT('Ctrl Pts',(-50.,13.3370379593182,4.53151803523741));
#52265=CARTESIAN_POINT('Ctrl Pts',(-50.,13.3152354345065,4.52309756402217));
#52266=CARTESIAN_POINT('',(-50.,12.8026622457696,5.81770965851215));
#52267=CARTESIAN_POINT('Origin',(-50.,0.,0.));
#52268=CARTESIAN_POINT('',(-50.,14.66105681156,7.29342431017219));
#52269=CARTESIAN_POINT('Ctrl Pts',(-50.,12.8026622457696,5.81770965851216));
#52270=CARTESIAN_POINT('Ctrl Pts',(-50.,12.8210521907127,5.82539925281556));
#52271=CARTESIAN_POINT('Ctrl Pts',(-50.,12.8577894805368,5.84088627843006));
#52272=CARTESIAN_POINT('Ctrl Pts',(-50.,12.9127676183656,5.86444032191588));
#52273=CARTESIAN_POINT('Ctrl Pts',(-50.,12.9858158402462,5.89649363499879));
#52274=CARTESIAN_POINT('Ctrl Pts',(-50.,13.0766775878848,5.93768004328337));
#52275=CARTESIAN_POINT('Ctrl Pts',(-50.,13.1670278530422,5.98009831397194));
#52276=CARTESIAN_POINT('Ctrl Pts',(-50.,13.2567440310958,6.02396476100794));
#52277=CARTESIAN_POINT('Ctrl Pts',(-50.,13.3456216156017,6.06963846112818));
#52278=CARTESIAN_POINT('Ctrl Pts',(-50.,13.4333611502533,6.11764308944358));
#52279=CARTESIAN_POINT('Ctrl Pts',(-50.,13.5196319660845,6.16854995125629));
#52280=CARTESIAN_POINT('Ctrl Pts',(-50.,13.6041308540151,6.22286996666888));
#52281=CARTESIAN_POINT('Ctrl Pts',(-50.,13.6866392230503,6.28094866827011));
#52282=CARTESIAN_POINT('Ctrl Pts',(-50.,13.7670900956865,6.342842540489));
#52283=CARTESIAN_POINT('Ctrl Pts',(-50.,13.845605534933,6.40825111076043));
#52284=CARTESIAN_POINT('Ctrl Pts',(-50.,13.9224187379158,6.47666628220192));
#52285=CARTESIAN_POINT('Ctrl Pts',(-50.,13.9978128588633,6.54749027478764));
#52286=CARTESIAN_POINT('Ctrl Pts',(-50.,14.0720574366665,6.62015787000295));
#52287=CARTESIAN_POINT('Ctrl Pts',(-50.,14.1453375866756,6.69427291666095));
#52288=CARTESIAN_POINT('Ctrl Pts',(-50.,14.2177129290574,6.76968712284877));
#52289=CARTESIAN_POINT('Ctrl Pts',(-50.,14.2891644580326,6.84640830625432));
#52290=CARTESIAN_POINT('Ctrl Pts',(-50.,14.3596259311217,6.92453872281182));
#52291=CARTESIAN_POINT('Ctrl Pts',(-50.,14.4290193778776,7.00420544769957));
#52292=CARTESIAN_POINT('Ctrl Pts',(-50.,14.497293115392,7.08548597048793));
#52293=CARTESIAN_POINT('Ctrl Pts',(-50.,14.5573535548322,7.15960958221619));
#52294=CARTESIAN_POINT('Ctrl Pts',(-50.,14.6033242178125,7.21807391177268));
#52295=CARTESIAN_POINT('Ctrl Pts',(-50.,14.6357314304385,7.26013580592497));
#52296=CARTESIAN_POINT('Ctrl Pts',(-50.,14.6549167396993,7.28533079690226));
#52297=CARTESIAN_POINT('Ctrl Pts',(-50.,14.66105681156,7.29342431017219));
#52298=CARTESIAN_POINT('',(-50.,14.0068170377451,8.48231698718778));
#52299=CARTESIAN_POINT('Origin',(-50.,0.,0.));
#52300=CARTESIAN_POINT('',(-50.,11.7720642054939,7.69236053443469));
#52301=CARTESIAN_POINT('Ctrl Pts',(-50.,14.0068170377451,8.48231698718778));
#52302=CARTESIAN_POINT('Ctrl Pts',(-50.,14.0063487265167,8.48230001257543));
#52303=CARTESIAN_POINT('Ctrl Pts',(-50.,13.9796594385348,8.481322225259));
#52304=CARTESIAN_POINT('Ctrl Pts',(-50.,13.9276649729564,8.47824257022821));
#52305=CARTESIAN_POINT('Ctrl Pts',(-50.,13.8525450817897,8.47033087635756));
#52306=CARTESIAN_POINT('Ctrl Pts',(-50.,13.7567621705396,8.45433520755552));
#52307=CARTESIAN_POINT('Ctrl Pts',(-50.,13.640364394729,8.42999540714673));
#52308=CARTESIAN_POINT('Ctrl Pts',(-50.,13.5228191963114,8.40557940304509));
#52309=CARTESIAN_POINT('Ctrl Pts',(-50.,13.4026082630414,8.38283636801991));
#52310=CARTESIAN_POINT('Ctrl Pts',(-50.,13.2802774448963,8.36126876569594));
#52311=CARTESIAN_POINT('Ctrl Pts',(-50.,13.1574330841607,8.33917830374554));
#52312=CARTESIAN_POINT('Ctrl Pts',(-50.,13.0360295127074,8.31440717472604));
#52313=CARTESIAN_POINT('Ctrl Pts',(-50.,12.9173840759125,8.28535136048938));
#52314=CARTESIAN_POINT('Ctrl Pts',(-50.,12.8019522591891,8.25123791004828));
#52315=CARTESIAN_POINT('Ctrl Pts',(-50.,12.6896863889879,8.21184725330542));
#52316=CARTESIAN_POINT('Ctrl Pts',(-50.,12.5802161423503,8.16739811498339));
#52317=CARTESIAN_POINT('Ctrl Pts',(-50.,12.4731248803097,8.11836113699226));
#52318=CARTESIAN_POINT('Ctrl Pts',(-50.,12.3681003919172,8.06533132620399));
#52319=CARTESIAN_POINT('Ctrl Pts',(-50.,12.2648981787049,8.00894915338555));
#52320=CARTESIAN_POINT('Ctrl Pts',(-50.,12.1633414705075,7.94981770572398));
#52321=CARTESIAN_POINT('Ctrl Pts',(-50.,12.0633068822383,7.88841516709048));
#52322=CARTESIAN_POINT('Ctrl Pts',(-50.,11.96471633848,7.82502798253687));
#52323=CARTESIAN_POINT('Ctrl Pts',(-50.,11.8869644478727,7.77285076392682));
#52324=CARTESIAN_POINT('Ctrl Pts',(-50.,11.8292726970256,7.73291674422561));
#52325=CARTESIAN_POINT('Ctrl Pts',(-50.,11.7910876778603,7.70593852849788));
#52326=CARTESIAN_POINT('Ctrl Pts',(-50.,11.7720642054939,7.69236053443469));
#52327=CARTESIAN_POINT('',(-50.,10.9536375103364,8.81882824088046));
#52328=CARTESIAN_POINT('Origin',(-50.,0.,0.));
#52329=CARTESIAN_POINT('',(-50.,12.3866518832851,10.7103445379834));
#52330=CARTESIAN_POINT('Ctrl Pts',(-50.,10.9536375103364,8.81882824088047));
#52331=CARTESIAN_POINT('Ctrl Pts',(-50.,10.9695373770028,8.83084964577152));
#52332=CARTESIAN_POINT('Ctrl Pts',(-50.,11.0012690306593,8.85498631045878));
#52333=CARTESIAN_POINT('Ctrl Pts',(-50.,11.0486622767737,8.89147286724882));
#52334=CARTESIAN_POINT('Ctrl Pts',(-50.,11.1114442196238,8.9406855206164));
#52335=CARTESIAN_POINT('Ctrl Pts',(-50.,11.1892087351483,9.00317437991606));
#52336=CARTESIAN_POINT('Ctrl Pts',(-50.,11.2661714856319,9.06672919987649));
#52337=CARTESIAN_POINT('Ctrl Pts',(-50.,11.3421599232118,9.13152900801114));
#52338=CARTESIAN_POINT('Ctrl Pts',(-50.,11.4168866676366,9.19787074131628));
#52339=CARTESIAN_POINT('Ctrl Pts',(-50.,11.4899314378663,9.26618715093123));
#52340=CARTESIAN_POINT('Ctrl Pts',(-50.,11.5608318756571,9.3369493595236));
#52341=CARTESIAN_POINT('Ctrl Pts',(-50.,11.629167237137,9.41057683066949));
#52342=CARTESIAN_POINT('Ctrl Pts',(-50.,11.6946398682888,9.48734988004618));
#52343=CARTESIAN_POINT('Ctrl Pts',(-50.,11.7571708487241,9.56730656089267));
#52344=CARTESIAN_POINT('Ctrl Pts',(-50.,11.8169531311064,9.65018619637799));
#52345=CARTESIAN_POINT('Ctrl Pts',(-50.,11.8743389448017,9.73555464618448));
#52346=CARTESIAN_POINT('Ctrl Pts',(-50.,11.9297512100749,9.82290332823825));
#52347=CARTESIAN_POINT('Ctrl Pts',(-50.,11.9835915618855,9.91175181299999));
#52348=CARTESIAN_POINT('Ctrl Pts',(-50.,12.0361378186387,10.0017624314164));
#52349=CARTESIAN_POINT('Ctrl Pts',(-50.,12.0874846061232,10.0928063773702));
#52350=CARTESIAN_POINT('Ctrl Pts',(-50.,12.1376115714812,10.1848864963973));
#52351=CARTESIAN_POINT('Ctrl Pts',(-50.,12.1864291233458,10.2780853580389));
#52352=CARTESIAN_POINT('Ctrl Pts',(-50.,12.2338301385431,10.3725066547111));
#52353=CARTESIAN_POINT('Ctrl Pts',(-50.,12.2797452870059,10.4682125884904));
#52354=CARTESIAN_POINT('Ctrl Pts',(-50.,12.3194850246607,10.5549438945599));
#52355=CARTESIAN_POINT('Ctrl Pts',(-50.,12.3494719472088,10.6230038986845));
#52356=CARTESIAN_POINT('Ctrl Pts',(-50.,12.3704006599468,10.6718036871368));
#52357=CARTESIAN_POINT('Ctrl Pts',(-50.,12.3827174879745,10.7009783235375));
#52358=CARTESIAN_POINT('Ctrl Pts',(-50.,12.3866518832851,10.7103445379834));
#52359=CARTESIAN_POINT('',(-50.,11.4573006693292,11.699183149801));
#52360=CARTESIAN_POINT('Origin',(-50.,0.,0.));
#52361=CARTESIAN_POINT('',(-50.,9.48921088782658,10.3782842019456));
#52362=CARTESIAN_POINT('Ctrl Pts',(-50.,11.4573006693292,11.699183149801));
#52363=CARTESIAN_POINT('Ctrl Pts',(-50.,11.4568512923737,11.6990502442108));
#52364=CARTESIAN_POINT('Ctrl Pts',(-50.,11.4312436632693,11.6914658198642));
#52365=CARTESIAN_POINT('Ctrl Pts',(-50.,11.3816485785003,11.6755524200814));
#52366=CARTESIAN_POINT('Ctrl Pts',(-50.,11.3108562751064,11.6492077293642));
#52367=CARTESIAN_POINT('Ctrl Pts',(-50.,11.2220605212152,11.6098943525204));
#52368=CARTESIAN_POINT('Ctrl Pts',(-50.,11.1153726577894,11.5573722819667));
#52369=CARTESIAN_POINT('Ctrl Pts',(-50.,11.0075923712357,11.5044910494005));
#52370=CARTESIAN_POINT('Ctrl Pts',(-50.,10.896814048301,11.4525672852113));
#52371=CARTESIAN_POINT('Ctrl Pts',(-50.,10.7836901223469,11.4012548314131));
#52372=CARTESIAN_POINT('Ctrl Pts',(-50.,10.6701988175887,11.3493082317362));
#52373=CARTESIAN_POINT('Ctrl Pts',(-50.,10.558769691859,11.2951234927996));
#52374=CARTESIAN_POINT('Ctrl Pts',(-50.,10.4510776067987,11.237474600108));
#52375=CARTESIAN_POINT('Ctrl Pts',(-50.,10.347755963003,11.1757261609666));
#52376=CARTESIAN_POINT('Ctrl Pts',(-50.,10.2488131895374,11.1096536475468));
#52377=CARTESIAN_POINT('Ctrl Pts',(-50.,10.1538362031934,11.0393768173572));
#52378=CARTESIAN_POINT('Ctrl Pts',(-50.,10.0623044106004,10.9652479123292));
#52379=CARTESIAN_POINT('Ctrl Pts',(-50.,9.97376743729857,10.8877656023939));
#52380=CARTESIAN_POINT('Ctrl Pts',(-50.,9.88782918758628,10.8074894324552));
#52381=CARTESIAN_POINT('Ctrl Pts',(-50.,9.80416846317344,10.7249595816546));
#52382=CARTESIAN_POINT('Ctrl Pts',(-50.,9.72254683584991,10.6406085262144));
#52383=CARTESIAN_POINT('Ctrl Pts',(-50.,9.64281744709338,10.5546942954216));
#52384=CARTESIAN_POINT('Ctrl Pts',(-50.,9.58048422171402,10.4848202111794));
#52385=CARTESIAN_POINT('Ctrl Pts',(-50.,9.53453615016101,10.4317934371322));
#52386=CARTESIAN_POINT('Ctrl Pts',(-50.,9.5042599930153,10.3961665635534));
#52387=CARTESIAN_POINT('Ctrl Pts',(-50.,9.48921088782658,10.3782842019456));
#52388=CARTESIAN_POINT('',(-50.,8.41635544546802,11.2658274114927));
#52389=CARTESIAN_POINT('Origin',(-50.,0.,0.));
#52390=CARTESIAN_POINT('',(-50.,9.33394806226437,13.4542944285812));
#52391=CARTESIAN_POINT('Ctrl Pts',(-50.,8.416355445468,11.2658274114927));
#52392=CARTESIAN_POINT('Ctrl Pts',(-50.,8.4287661867593,11.2814252778905));
#52393=CARTESIAN_POINT('Ctrl Pts',(-50.,8.45349838774813,11.3126949862398));
#52394=CARTESIAN_POINT('Ctrl Pts',(-50.,8.49032885019461,11.3598214717827));
#52395=CARTESIAN_POINT('Ctrl Pts',(-50.,8.53889969364915,11.4231012534324));
#52396=CARTESIAN_POINT('Ctrl Pts',(-50.,8.59868074655117,11.5029661588994));
#52397=CARTESIAN_POINT('Ctrl Pts',(-50.,8.657420129699,11.5836641450553));
#52398=CARTESIAN_POINT('Ctrl Pts',(-50.,8.71490619380604,11.6653257040265));
#52399=CARTESIAN_POINT('Ctrl Pts',(-50.,8.77078674197194,11.7481669754252));
#52400=CARTESIAN_POINT('Ctrl Pts',(-50.,8.82454707622628,11.8325025950734));
#52401=CARTESIAN_POINT('Ctrl Pts',(-50.,8.87562220071675,11.9186739006343));
#52402=CARTESIAN_POINT('Ctrl Pts',(-50.,8.9235002736643,12.0069825427185));
#52403=CARTESIAN_POINT('Ctrl Pts',(-50.,8.96782328072592,12.0976260068268));
#52404=CARTESIAN_POINT('Ctrl Pts',(-50.,9.00850531748659,12.1906215239832));
#52405=CARTESIAN_POINT('Ctrl Pts',(-50.,9.04579810233888,12.2857645923749));
#52406=CARTESIAN_POINT('Ctrl Pts',(-50.,9.08015076502197,12.3827223068819));
#52407=CARTESIAN_POINT('Ctrl Pts',(-50.,9.11209941820162,12.4811072394643));
#52408=CARTESIAN_POINT('Ctrl Pts',(-50.,9.14215255670447,12.580553936713));
#52409=CARTESIAN_POINT('Ctrl Pts',(-50.,9.17066324563836,12.6808044286968));
#52410=CARTESIAN_POINT('Ctrl Pts',(-50.,9.19775517072751,12.7817574884561));
#52411=CARTESIAN_POINT('Ctrl Pts',(-50.,9.22340791088078,12.8834108105793));
#52412=CARTESIAN_POINT('Ctrl Pts',(-50.,9.24751415519882,12.9858220900665));
#52413=CARTESIAN_POINT('Ctrl Pts',(-50.,9.26994435872398,13.0890651211961));
#52414=CARTESIAN_POINT('Ctrl Pts',(-50.,9.29061590049322,13.1931829101653));
#52415=CARTESIAN_POINT('Ctrl Pts',(-50.,9.30753794249323,13.2870722636402));
#52416=CARTESIAN_POINT('Ctrl Pts',(-50.,9.3196569359812,13.3604514819665));
#52417=CARTESIAN_POINT('Ctrl Pts',(-50.,9.32779212083946,13.4129228945374));
#52418=CARTESIAN_POINT('Ctrl Pts',(-50.,9.33246655603105,13.4442440266596));
#52419=CARTESIAN_POINT('Ctrl Pts',(-50.,9.33394806226437,13.4542944285812));
#52420=CARTESIAN_POINT('',(-50.,8.1878799628551,14.1809466085264));
#52421=CARTESIAN_POINT('Origin',(-50.,0.,0.));
#52422=CARTESIAN_POINT('',(-50.,6.61011555120064,12.4121021043889));
#52423=CARTESIAN_POINT('Ctrl Pts',(-50.,8.1878799628551,14.1809466085264));
#52424=CARTESIAN_POINT('Ctrl Pts',(-50.,8.18747775617919,14.1807061229053));
#52425=CARTESIAN_POINT('Ctrl Pts',(-50.,8.16456080746724,14.1669916188038));
#52426=CARTESIAN_POINT('Ctrl Pts',(-50.,8.12048134508164,14.1392443717028));
#52427=CARTESIAN_POINT('Ctrl Pts',(-50.,8.05846477023863,14.0961220179458));
#52428=CARTESIAN_POINT('Ctrl Pts',(-50.,7.9822355374912,14.0359611371119));
#52429=CARTESIAN_POINT('Ctrl Pts',(-50.,7.89196117727994,13.9585569512687));
#52430=CARTESIAN_POINT('Ctrl Pts',(-50.,7.80071803438238,13.8805332125637));
#52431=CARTESIAN_POINT('Ctrl Pts',(-50.,7.70633293122716,13.8026912802767));
#52432=CARTESIAN_POINT('Ctrl Pts',(-50.,7.60952388977251,13.7248581251904));
#52433=CARTESIAN_POINT('Ctrl Pts',(-50.,7.51251671706145,13.646319383691));
#52434=CARTESIAN_POINT('Ctrl Pts',(-50.,7.41806353883254,13.5661256612623));
#52435=CARTESIAN_POINT('Ctrl Pts',(-50.,7.32809149527493,13.4835059820612));
#52436=CARTESIAN_POINT('Ctrl Pts',(-50.,7.24337210327696,13.3980024357456));
#52437=CARTESIAN_POINT('Ctrl Pts',(-50.,7.16396936488986,13.3093996446649));
#52438=CARTESIAN_POINT('Ctrl Pts',(-50.,7.08945339219251,13.2177108743086));
#52439=CARTESIAN_POINT('Ctrl Pts',(-50.,7.01923234820612,13.1231478339735));
#52440=CARTESIAN_POINT('Ctrl Pts',(-50.,6.95274599364373,13.0260815233846));
#52441=CARTESIAN_POINT('Ctrl Pts',(-50.,6.88947152371961,12.9269554033179));
#52442=CARTESIAN_POINT('Ctrl Pts',(-50.,6.82896349408885,12.8262128034276));
#52443=CARTESIAN_POINT('Ctrl Pts',(-50.,6.77088341473902,12.7242133182155));
#52444=CARTESIAN_POINT('Ctrl Pts',(-50.,6.71502487170408,12.6211703482748));
#52445=CARTESIAN_POINT('Ctrl Pts',(-50.,6.67202693734873,12.5379898440923));
#52446=CARTESIAN_POINT('Ctrl Pts',(-50.,6.64070963141069,12.4752021829311));
#52447=CARTESIAN_POINT('Ctrl Pts',(-50.,6.62024469858602,12.4331652189947));
#52448=CARTESIAN_POINT('Ctrl Pts',(-50.,6.61011555120064,12.4121021043889));
#52449=CARTESIAN_POINT('',(-50.,5.35024281477072,13.004953213026));
#52450=CARTESIAN_POINT('Origin',(-50.,0.,0.));
#52451=CARTESIAN_POINT('',(-50.,5.69475795663189,15.3528615187976));
#52452=CARTESIAN_POINT('Ctrl Pts',(-50.,5.35024281477071,13.004953213026));
#52453=CARTESIAN_POINT('Ctrl Pts',(-50.,5.35838461816811,13.0231474696198));
#52454=CARTESIAN_POINT('Ctrl Pts',(-50.,5.37456335134248,13.0595854308535));
#52455=CARTESIAN_POINT('Ctrl Pts',(-50.,5.39851683671257,13.1143907147436));
#52456=CARTESIAN_POINT('Ctrl Pts',(-50.,5.42982469604617,13.1877615232676));
#52457=CARTESIAN_POINT('Ctrl Pts',(-50.,5.46786602291259,13.2799842691689));
#52458=CARTESIAN_POINT('Ctrl Pts',(-50.,5.50469122725311,13.3727548702637));
#52459=CARTESIAN_POINT('Ctrl Pts',(-50.,5.54006285706051,13.466147083991));
#52460=CARTESIAN_POINT('Ctrl Pts',(-50.,5.57358602861192,13.5602826717323));
#52461=CARTESIAN_POINT('Ctrl Pts',(-50.,5.60468396737303,13.6553383842666));
#52462=CARTESIAN_POINT('Ctrl Pts',(-50.,5.63272454065023,13.7515043267519));
#52463=CARTESIAN_POINT('Ctrl Pts',(-50.,5.65713696965892,13.8489453830157));
#52464=CARTESIAN_POINT('Ctrl Pts',(-50.,5.67752537508807,13.9477637996424));
#52465=CARTESIAN_POINT('Ctrl Pts',(-50.,5.6938022661864,14.0479549027521));
#52466=CARTESIAN_POINT('Ctrl Pts',(-50.,5.70626231068308,14.1493832151514));
#52467=CARTESIAN_POINT('Ctrl Pts',(-50.,5.71542331821735,14.2518379845708));
#52468=CARTESIAN_POINT('Ctrl Pts',(-50.,5.72190090792526,14.3550772805332));
#52469=CARTESIAN_POINT('Ctrl Pts',(-50.,5.72627848390049,14.4588735885414));
#52470=CARTESIAN_POINT('Ctrl Pts',(-50.,5.72896217357436,14.5630648469857));
#52471=CARTESIAN_POINT('Ctrl Pts',(-50.,5.73009695097776,14.6675837685266));
#52472=CARTESIAN_POINT('Ctrl Pts',(-50.,5.72966360991829,14.772423041662));
#52473=CARTESIAN_POINT('Ctrl Pts',(-50.,5.72754386270271,14.8776118616624));
#52474=CARTESIAN_POINT('Ctrl Pts',(-50.,5.72359388237569,14.9831894879022));
#52475=CARTESIAN_POINT('Ctrl Pts',(-50.,5.71772294845736,15.0891770284618));
#52476=CARTESIAN_POINT('Ctrl Pts',(-50.,5.71076402066882,15.1843250159624));
#52477=CARTESIAN_POINT('Ctrl Pts',(-50.,5.70425360416528,15.2584127623331));
#52478=CARTESIAN_POINT('Ctrl Pts',(-50.,5.69908409756002,15.3112588271944));
#52479=CARTESIAN_POINT('Ctrl Pts',(-50.,5.69582242796104,15.3427584331158));
#52480=CARTESIAN_POINT('Ctrl Pts',(-50.,5.69475795663189,15.3528615187976));
#52481=CARTESIAN_POINT('',(-50.,4.40398464539872,15.7716690379646));
#52482=CARTESIAN_POINT('Origin',(-50.,0.,0.));
#52483=CARTESIAN_POINT('',(-50.,3.31568234418832,13.6660219830951));
#52484=CARTESIAN_POINT('Ctrl Pts',(-50.,4.40398464539872,15.7716690379646));
#52485=CARTESIAN_POINT('Ctrl Pts',(-50.,4.40365488112711,15.7713360829087));
#52486=CARTESIAN_POINT('Ctrl Pts',(-50.,4.38486856897779,15.7523532317834));
#52487=CARTESIAN_POINT('Ctrl Pts',(-50.,4.34907440371019,15.7145155989467));
#52488=CARTESIAN_POINT('Ctrl Pts',(-50.,4.29973028689649,15.6573251182294));
#52489=CARTESIAN_POINT('Ctrl Pts',(-50.,4.24085733833789,15.5800968628044));
#52490=CARTESIAN_POINT('Ctrl Pts',(-50.,4.17266875139903,15.482674151341));
#52491=CARTESIAN_POINT('Ctrl Pts',(-50.,4.10369589439471,15.3844104249513));
#52492=CARTESIAN_POINT('Ctrl Pts',(-50.,4.03163457417435,15.2855414194547));
#52493=CARTESIAN_POINT('Ctrl Pts',(-50.,3.95722328533246,15.1860781064647));
#52494=CARTESIAN_POINT('Ctrl Pts',(-50.,3.88279556209739,15.0858821011164));
#52495=CARTESIAN_POINT('Ctrl Pts',(-50.,3.81125317193191,14.9847182617076));
#52496=CARTESIAN_POINT('Ctrl Pts',(-50.,3.74465444426779,14.8823190942953));
#52497=CARTESIAN_POINT('Ctrl Pts',(-50.,3.68386053504292,14.7784329430806));
#52498=CARTESIAN_POINT('Ctrl Pts',(-50.,3.62898699781003,14.6728671135607));
#52499=CARTESIAN_POINT('Ctrl Pts',(-50.,3.57961415137445,14.5655275456869));
#52500=CARTESIAN_POINT('Ctrl Pts',(-50.,3.53511610244324,14.4564721136477));
#52501=CARTESIAN_POINT('Ctrl Pts',(-50.,3.49485794879717,14.3459208356842));
#52502=CARTESIAN_POINT('Ctrl Pts',(-50.,3.45822302631379,14.2341732241738));
#52503=CARTESIAN_POINT('Ctrl Pts',(-50.,3.42466963349977,14.1215479032503));
#52504=CARTESIAN_POINT('Ctrl Pts',(-50.,3.39378048711278,14.0083089910501));
#52505=CARTESIAN_POINT('Ctrl Pts',(-50.,3.36530258749166,13.8946118507282));
#52506=CARTESIAN_POINT('Ctrl Pts',(-50.,3.34434166251121,13.8033514635997));
#52507=CARTESIAN_POINT('Ctrl Pts',(-50.,3.32962290369722,13.7347480949923));
#52508=CARTESIAN_POINT('Ctrl Pts',(-50.,3.32025508218772,13.6889423777435));
#52509=CARTESIAN_POINT('Ctrl Pts',(-50.,3.31568234418832,13.6660219830951));
#52510=CARTESIAN_POINT('',(-50.,1.94795475120473,13.9269299753125));
#52511=CARTESIAN_POINT('Origin',(-50.,0.,0.));
#52512=CARTESIAN_POINT('',(-50.,1.69774526472952,16.2867518559131));
#52513=CARTESIAN_POINT('Ctrl Pts',(-50.,1.94795475120472,13.9269299753125));
#52514=CARTESIAN_POINT('Ctrl Pts',(-50.,1.9513160372573,13.9465774100468));
#52515=CARTESIAN_POINT('Ctrl Pts',(-50.,1.95792473331065,13.9858940930512));
#52516=CARTESIAN_POINT('Ctrl Pts',(-50.,1.96749615602378,14.044934557742));
#52517=CARTESIAN_POINT('Ctrl Pts',(-50.,1.97957384329226,14.1237862354018));
#52518=CARTESIAN_POINT('Ctrl Pts',(-50.,1.99348516764985,14.2225721274408));
#52519=CARTESIAN_POINT('Ctrl Pts',(-50.,2.00608233016073,14.3215862254212));
#52520=CARTESIAN_POINT('Ctrl Pts',(-50.,2.01711699607993,14.4208409176437));
#52521=CARTESIAN_POINT('Ctrl Pts',(-50.,2.02617640685866,14.5203559365434));
#52522=CARTESIAN_POINT('Ctrl Pts',(-50.,2.03265795226397,14.6201590419547));
#52523=CARTESIAN_POINT('Ctrl Pts',(-50.,2.03590208198289,14.7202771615244));
#52524=CARTESIAN_POINT('Ctrl Pts',(-50.,2.03531494435546,14.8207280520398));
#52525=CARTESIAN_POINT('Ctrl Pts',(-50.,2.03048766965571,14.9215122966393));
#52526=CARTESIAN_POINT('Ctrl Pts',(-50.,2.02133667816179,15.022603610217));
#52527=CARTESIAN_POINT('Ctrl Pts',(-50.,2.00818107188229,15.1239440527286));
#52528=CARTESIAN_POINT('Ctrl Pts',(-50.,1.99157480447254,15.2254582670956));
#52529=CARTESIAN_POINT('Ctrl Pts',(-50.,1.97217431992445,15.3270650217851));
#52530=CARTESIAN_POINT('Ctrl Pts',(-50.,1.95060127417394,15.4286890367845));
#52531=CARTESIAN_POINT('Ctrl Pts',(-50.,1.92728933849566,15.5302743417326));
#52532=CARTESIAN_POINT('Ctrl Pts',(-50.,1.90239566597564,15.6317918168208));
#52533=CARTESIAN_POINT('Ctrl Pts',(-50.,1.87590347211591,15.7332296038656));
#52534=CARTESIAN_POINT('Ctrl Pts',(-50.,1.84769092488014,15.8345865639611));
#52535=CARTESIAN_POINT('Ctrl Pts',(-50.,1.8176089524919,15.9358649547671));
#52536=CARTESIAN_POINT('Ctrl Pts',(-50.,1.78556443525587,16.0370626599488));
#52537=CARTESIAN_POINT('Ctrl Pts',(-50.,1.75516179270489,16.1274907834907));
#52538=CARTESIAN_POINT('Ctrl Pts',(-50.,1.73043103962239,16.1976318523256));
#52539=CARTESIAN_POINT('Ctrl Pts',(-50.,1.71228166066573,16.2475320568679));
#52540=CARTESIAN_POINT('Ctrl Pts',(-50.,1.70128882897267,16.2772309005009));
#52541=CARTESIAN_POINT('Ctrl Pts',(-50.,1.69774526472952,16.2867518559131));
#52542=CARTESIAN_POINT('',(-50.,0.343370775949385,16.3713994976063));
#52543=CARTESIAN_POINT('Origin',(-50.,0.,0.));
#52544=CARTESIAN_POINT('',(-50.,-0.187087378736033,14.0612554404903));
#52545=CARTESIAN_POINT('Ctrl Pts',(-50.,0.343370775949385,16.3713994976063));
#52546=CARTESIAN_POINT('Ctrl Pts',(-50.,0.343134174384057,16.3709949939062));
#52547=CARTESIAN_POINT('Ctrl Pts',(-50.,0.329658911880923,16.3479365581074));
#52548=CARTESIAN_POINT('Ctrl Pts',(-50.,0.304399122776818,16.3023860171632));
#52549=CARTESIAN_POINT('Ctrl Pts',(-50.,0.270827936326797,16.2347208977209));
#52550=CARTESIAN_POINT('Ctrl Pts',(-50.,0.233010475834533,16.1452778030188));
#52551=CARTESIAN_POINT('Ctrl Pts',(-50.,0.191192201865526,16.0339579931922));
#52552=CARTESIAN_POINT('Ctrl Pts',(-50.,0.148823449024451,15.9216285504355));
#52553=CARTESIAN_POINT('Ctrl Pts',(-50.,0.103613789511375,15.8079447749594));
#52554=CARTESIAN_POINT('Ctrl Pts',(-50.,0.0562757882257695,15.6931009498213));
#52555=CARTESIAN_POINT('Ctrl Pts',(-50.,0.00910408204356977,15.5775433641354));
#52556=CARTESIAN_POINT('Ctrl Pts',(-50.,-0.035032248569878,15.4617659038311));
#52557=CARTESIAN_POINT('Ctrl Pts',(-50.,-0.0740730173483893,15.3460213644938));
#52558=CARTESIAN_POINT('Ctrl Pts',(-50.,-0.107121538899203,15.2302801573274));
#52559=CARTESIAN_POINT('Ctrl Pts',(-50.,-0.13401796882278,15.1143843786811));
#52560=CARTESIAN_POINT('Ctrl Pts',(-50.,-0.155145411474415,14.9981385531066));
#52561=CARTESIAN_POINT('Ctrl Pts',(-50.,-0.171124489283723,14.8814430832361));
#52562=CARTESIAN_POINT('Ctrl Pts',(-50.,-0.182624874160768,14.7643531812717));
#52563=CARTESIAN_POINT('Ctrl Pts',(-50.,-0.190318342289957,14.6470055917277));
#52564=CARTESIAN_POINT('Ctrl Pts',(-50.,-0.194808815215985,14.5295742128916));
#52565=CARTESIAN_POINT('Ctrl Pts',(-50.,-0.196566149970303,14.4122110910203));
#52566=CARTESIAN_POINT('Ctrl Pts',(-50.,-0.195874035010017,14.2950037897925));
#52567=CARTESIAN_POINT('Ctrl Pts',(-50.,-0.193480898610155,14.2013977454735));
#52568=CARTESIAN_POINT('Ctrl Pts',(-50.,-0.190676276552008,14.1312892713751));
#52569=CARTESIAN_POINT('Ctrl Pts',(-50.,-0.188358372068459,14.0845929424903));
#52570=CARTESIAN_POINT('Ctrl Pts',(-50.,-0.187087378736033,14.0612554404903));
#52571=CARTESIAN_POINT('',(-50.,-1.57673047345589,13.9738265075847));
#52572=CARTESIAN_POINT('Origin',(-50.,0.,0.));
#52573=CARTESIAN_POINT('',(-50.,-2.40594300602614,16.1972856754381));
#52574=CARTESIAN_POINT('Ctrl Pts',(-50.,-1.57673047345591,13.9738265075847));
#52575=CARTESIAN_POINT('Ctrl Pts',(-50.,-1.57836090671277,13.9936925998767));
#52576=CARTESIAN_POINT('Ctrl Pts',(-50.,-1.58173749645856,14.0334175928621));
#52577=CARTESIAN_POINT('Ctrl Pts',(-50.,-1.58714954409268,14.0929835088213));
#52578=CARTESIAN_POINT('Ctrl Pts',(-50.,-1.59506091439902,14.1723615147133));
#52579=CARTESIAN_POINT('Ctrl Pts',(-50.,-1.60615369222193,14.2715034719842));
#52580=CARTESIAN_POINT('Ctrl Pts',(-50.,-1.61857609759037,14.3705396469258));
#52581=CARTESIAN_POINT('Ctrl Pts',(-50.,-1.63257174420173,14.4694202802978));
#52582=CARTESIAN_POINT('Ctrl Pts',(-50.,-1.64854533029309,14.5680618357278));
#52583=CARTESIAN_POINT('Ctrl Pts',(-50.,-1.66708743757887,14.6663413378531));
#52584=CARTESIAN_POINT('Ctrl Pts',(-50.,-1.68884359201954,14.7641208448459));
#52585=CARTESIAN_POINT('Ctrl Pts',(-50.,-1.71439340426661,14.8612698707291));
#52586=CARTESIAN_POINT('Ctrl Pts',(-50.,-1.74413304367239,14.957687298555));
#52587=CARTESIAN_POINT('Ctrl Pts',(-50.,-1.77813692730802,15.0533268835806));
#52588=CARTESIAN_POINT('Ctrl Pts',(-50.,-1.81608156923822,15.1482118634974));
#52589=CARTESIAN_POINT('Ctrl Pts',(-50.,-1.85741167873706,15.2424070113801));
#52590=CARTESIAN_POINT('Ctrl Pts',(-50.,-1.901471233747,15.3359968987161));
#52591=CARTESIAN_POINT('Ctrl Pts',(-50.,-1.94763938741864,15.4290632100973));
#52592=CARTESIAN_POINT('Ctrl Pts',(-50.,-1.99548217379509,15.5216595832348));
#52593=CARTESIAN_POINT('Ctrl Pts',(-50.,-2.04484013524158,15.6137968955554));
#52594=CARTESIAN_POINT('Ctrl Pts',(-50.,-2.09572657992989,15.7054594872874));
#52595=CARTESIAN_POINT('Ctrl Pts',(-50.,-2.14825922908453,15.7966159569104));
#52596=CARTESIAN_POINT('Ctrl Pts',(-50.,-2.20258303257508,15.8872314185123));
#52597=CARTESIAN_POINT('Ctrl Pts',(-50.,-2.25878765825938,15.9772806643205));
#52598=CARTESIAN_POINT('Ctrl Pts',(-50.,-2.31072370572823,16.0573069923301));
#52599=CARTESIAN_POINT('Ctrl Pts',(-50.,-2.35212087122016,16.1190941623136));
#52600=CARTESIAN_POINT('Ctrl Pts',(-50.,-2.38210973029964,16.1629130931652));
#52601=CARTESIAN_POINT('Ctrl Pts',(-50.,-2.40014300404269,16.1889450869399));
#52602=CARTESIAN_POINT('Ctrl Pts',(-50.,-2.40594300602614,16.1972856754381));
#52603=CARTESIAN_POINT('',(-50.,-3.73881834218223,15.9424547170177));
#52604=CARTESIAN_POINT('Origin',(-50.,0.,0.));
#52605=CARTESIAN_POINT('',(-50.,-3.67810171359515,13.5729685048794));
#52606=CARTESIAN_POINT('Ctrl Pts',(-50.,-3.73881834218223,15.9424547170177));
#52607=CARTESIAN_POINT('Ctrl Pts',(-50.,-3.73894691449477,15.9420040811286));
#52608=CARTESIAN_POINT('Ctrl Pts',(-50.,-3.74626442705009,15.9163189069806));
#52609=CARTESIAN_POINT('Ctrl Pts',(-50.,-3.75940267454228,15.8659175659396));
#52610=CARTESIAN_POINT('Ctrl Pts',(-50.,-3.77509152951778,15.7920294560818));
#52611=CARTESIAN_POINT('Ctrl Pts',(-50.,-3.7894772918181,15.6959915606914));
#52612=CARTESIAN_POINT('Ctrl Pts',(-50.,-3.80229765686693,15.5777692855585));
#52613=CARTESIAN_POINT('Ctrl Pts',(-50.,-3.81540012098238,15.4584321984421));
#52614=CARTESIAN_POINT('Ctrl Pts',(-50.,-3.83091743061146,15.3370768226993));
#52615=CARTESIAN_POINT('Ctrl Pts',(-50.,-3.84820772362302,15.2140685453126));
#52616=CARTESIAN_POINT('Ctrl Pts',(-50.,-3.86515944096752,15.0904102873887));
#52617=CARTESIAN_POINT('Ctrl Pts',(-50.,-3.87911646405442,14.9672939298197));
#52618=CARTESIAN_POINT('Ctrl Pts',(-50.,-3.88814619886307,14.8454766736426));
#52619=CARTESIAN_POINT('Ctrl Pts',(-50.,-3.89137277258683,14.725152856237));
#52620=CARTESIAN_POINT('Ctrl Pts',(-50.,-3.88860209359085,14.6062092864715));
#52621=CARTESIAN_POINT('Ctrl Pts',(-50.,-3.88015661753544,14.4883613559395));
#52622=CARTESIAN_POINT('Ctrl Pts',(-50.,-3.86661269999714,14.3713582537855));
#52623=CARTESIAN_POINT('Ctrl Pts',(-50.,-3.84863270462788,14.2550869169872));
#52624=CARTESIAN_POINT('Ctrl Pts',(-50.,-3.82690130950572,14.1395127300348));
#52625=CARTESIAN_POINT('Ctrl Pts',(-50.,-3.80204670961501,14.0246539387008));
#52626=CARTESIAN_POINT('Ctrl Pts',(-50.,-3.77456181293102,13.910540963737));
#52627=CARTESIAN_POINT('Ctrl Pts',(-50.,-3.7447431715177,13.7971880673979));
#52628=CARTESIAN_POINT('Ctrl Pts',(-50.,-3.71914634329887,13.7071179779119));
#52629=CARTESIAN_POINT('Ctrl Pts',(-50.,-3.69899456508718,13.6399095715909));
#52630=CARTESIAN_POINT('Ctrl Pts',(-50.,-3.68513657707394,13.595256733151));
#52631=CARTESIAN_POINT('Ctrl Pts',(-50.,-3.67810171359515,13.5729685048794));
#52632=CARTESIAN_POINT('',(-50.,-5.00234392366024,13.1426961282463));
#52633=CARTESIAN_POINT('Origin',(-50.,0.,0.));
#52634=CARTESIAN_POINT('',(-50.,-6.35845702927375,15.0900844665257));
#52635=CARTESIAN_POINT('Ctrl Pts',(-50.,-5.00234392366025,13.1426961282463));
#52636=CARTESIAN_POINT('Ctrl Pts',(-50.,-5.00886363010872,13.1615326184551));
#52637=CARTESIAN_POINT('Ctrl Pts',(-50.,-5.02201334210169,13.1991698540138));
#52638=CARTESIAN_POINT('Ctrl Pts',(-50.,-5.04206880122609,13.2555184756737));
#52639=CARTESIAN_POINT('Ctrl Pts',(-50.,-5.06947212861492,13.3304351977558));
#52640=CARTESIAN_POINT('Ctrl Pts',(-50.,-5.10487200859133,13.4237037664646));
#52641=CARTESIAN_POINT('Ctrl Pts',(-50.,-5.14153343642338,13.5165392112663));
#52642=CARTESIAN_POINT('Ctrl Pts',(-50.,-5.17967999761633,13.6088327519355));
#52643=CARTESIAN_POINT('Ctrl Pts',(-50.,-5.21968290141691,13.7004028321899));
#52644=CARTESIAN_POINT('Ctrl Pts',(-50.,-5.2620835925999,13.7909834684638));
#52645=CARTESIAN_POINT('Ctrl Pts',(-50.,-5.30747301200313,13.8802805168475));
#52646=CARTESIAN_POINT('Ctrl Pts',(-50.,-5.35638011020072,13.9680234475133));
#52647=CARTESIAN_POINT('Ctrl Pts',(-50.,-5.40916346339393,14.0540157969766));
#52648=CARTESIAN_POINT('Ctrl Pts',(-50.,-5.46588365010489,14.1381942665852));
#52649=CARTESIAN_POINT('Ctrl Pts',(-50.,-5.52623312628269,14.2206618116565));
#52650=CARTESIAN_POINT('Ctrl Pts',(-50.,-5.5896901550893,14.301619265488));
#52651=CARTESIAN_POINT('Ctrl Pts',(-50.,-5.6556403566801,14.3813116886496));
#52652=CARTESIAN_POINT('Ctrl Pts',(-50.,-5.72350270338309,14.4599725977946));
#52653=CARTESIAN_POINT('Ctrl Pts',(-50.,-5.79287020223623,14.5377618684515));
#52654=CARTESIAN_POINT('Ctrl Pts',(-50.,-5.86359111036561,14.614729691814));
#52655=CARTESIAN_POINT('Ctrl Pts',(-50.,-5.93567442341548,14.6908575904833));
#52656=CARTESIAN_POINT('Ctrl Pts',(-50.,-6.00922635494104,14.7660858733973));
#52657=CARTESIAN_POINT('Ctrl Pts',(-50.,-6.08437862517161,14.8403447030824));
#52658=CARTESIAN_POINT('Ctrl Pts',(-50.,-6.16121181596629,14.913587364225));
#52659=CARTESIAN_POINT('Ctrl Pts',(-50.,-6.23141793548312,14.9781835481972));
#52660=CARTESIAN_POINT('Ctrl Pts',(-50.,-6.2868803772285,15.027734504202));
#52661=CARTESIAN_POINT('Ctrl Pts',(-50.,-6.32682440612351,15.0627188567828));
#52662=CARTESIAN_POINT('Ctrl Pts',(-50.,-6.35076502500555,15.0834483147912));
#52663=CARTESIAN_POINT('Ctrl Pts',(-50.,-6.35845702927375,15.0900844665257));
#52664=CARTESIAN_POINT('',(-50.,-7.58608375346252,14.5117868743119));
#52665=CARTESIAN_POINT('Origin',(-50.,0.,0.));
#52666=CARTESIAN_POINT('',(-50.,-6.93800739067721,12.2318420402206));
#52667=CARTESIAN_POINT('Ctrl Pts',(-50.,-7.58608375346252,14.5117868743119));
#52668=CARTESIAN_POINT('Ctrl Pts',(-50.,-7.58609621785102,14.511318421344));
#52669=CARTESIAN_POINT('Ctrl Pts',(-50.,-7.58679619423276,14.4846204028018));
#52670=CARTESIAN_POINT('Ctrl Pts',(-50.,-7.58698737570401,14.4325351632849));
#52671=CARTESIAN_POINT('Ctrl Pts',(-50.,-7.5838081107473,14.3570667246954));
#52672=CARTESIAN_POINT('Ctrl Pts',(-50.,-7.5738582645032,14.2604684427868));
#52673=CARTESIAN_POINT('Ctrl Pts',(-50.,-7.55687516994583,14.1427720426853));
#52674=CARTESIAN_POINT('Ctrl Pts',(-50.,-7.53988806932779,14.0239256992838));
#52675=CARTESIAN_POINT('Ctrl Pts',(-50.,-7.52473801944021,13.9025239278461));
#52676=CARTESIAN_POINT('Ctrl Pts',(-50.,-7.51089419147856,13.7790802606718));
#52677=CARTESIAN_POINT('Ctrl Pts',(-50.,-7.49656078124055,13.6550912336386));
#52678=CARTESIAN_POINT('Ctrl Pts',(-50.,-7.47946152571002,13.5323718323411));
#52679=CARTESIAN_POINT('Ctrl Pts',(-50.,-7.45791285510172,13.4121360855424));
#52680=CARTESIAN_POINT('Ctrl Pts',(-50.,-7.43111474350486,13.2947900458654));
#52681=CARTESIAN_POINT('Ctrl Pts',(-50.,-7.39885104754049,13.1802723469128));
#52682=CARTESIAN_POINT('Ctrl Pts',(-50.,-7.36136331309888,13.0682271303129));
#52683=CARTESIAN_POINT('Ctrl Pts',(-50.,-7.31914741436296,12.9582681310911));
#52684=CARTESIAN_POINT('Ctrl Pts',(-50.,-7.27281678798223,12.8501211151659));
#52685=CARTESIAN_POINT('Ctrl Pts',(-50.,-7.22302599308674,12.7435822820237));
#52686=CARTESIAN_POINT('Ctrl Pts',(-50.,-7.17038802629925,12.6385130784722));
#52687=CARTESIAN_POINT('Ctrl Pts',(-50.,-7.11538787531798,12.5348203883111));
#52688=CARTESIAN_POINT('Ctrl Pts',(-50.,-7.05831632235693,12.4324442762203));
#52689=CARTESIAN_POINT('Ctrl Pts',(-50.,-7.01112414517467,12.3515695765444));
#52690=CARTESIAN_POINT('Ctrl Pts',(-50.,-6.97489142114752,12.2914841893452));
#52691=CARTESIAN_POINT('Ctrl Pts',(-50.,-6.95036409795758,12.2516805434111));
#52692=CARTESIAN_POINT('Ctrl Pts',(-50.,-6.93800739067721,12.2318420402206));
#52693=CARTESIAN_POINT('',(-50.,-8.11364170780697,11.4857618157149));
#52694=CARTESIAN_POINT('Origin',(-50.,0.,0.));
#52695=CARTESIAN_POINT('',(-50.,-9.91144581260293,13.0347177531328));
#52696=CARTESIAN_POINT('Ctrl Pts',(-50.,-8.11364170780698,11.4857618157149));
#52697=CARTESIAN_POINT('Ctrl Pts',(-50.,-8.12464103031309,11.502385137885));
#52698=CARTESIAN_POINT('Ctrl Pts',(-50.,-8.14673761978747,11.5355697300868));
#52699=CARTESIAN_POINT('Ctrl Pts',(-50.,-8.18017633214654,11.5851604663126));
#52700=CARTESIAN_POINT('Ctrl Pts',(-50.,-8.22534976477564,11.6509086114121));
#52701=CARTESIAN_POINT('Ctrl Pts',(-50.,-8.28283244225497,11.732443384369));
#52702=CARTESIAN_POINT('Ctrl Pts',(-50.,-8.34142932020866,11.8132449066089));
#52703=CARTESIAN_POINT('Ctrl Pts',(-50.,-8.40132990725019,11.8931522119833));
#52704=CARTESIAN_POINT('Ctrl Pts',(-50.,-8.46284859919381,11.9718971321485));
#52705=CARTESIAN_POINT('Ctrl Pts',(-50.,-8.52644368290816,12.0490873880617));
#52706=CARTESIAN_POINT('Ctrl Pts',(-50.,-8.59261438312223,12.1242911158748));
#52707=CARTESIAN_POINT('Ctrl Pts',(-50.,-8.66180575442286,12.1971147402934));
#52708=CARTESIAN_POINT('Ctrl Pts',(-50.,-8.73431624919877,12.2672787958196));
#52709=CARTESIAN_POINT('Ctrl Pts',(-50.,-8.81018880105177,12.334706907179));
#52710=CARTESIAN_POINT('Ctrl Pts',(-50.,-8.88915113193907,12.3995752782536));
#52711=CARTESIAN_POINT('Ctrl Pts',(-50.,-8.9707478415549,12.4622081834688));
#52712=CARTESIAN_POINT('Ctrl Pts',(-50.,-9.05444479601274,12.5229957744206));
#52713=CARTESIAN_POINT('Ctrl Pts',(-50.,-9.13973729492348,12.5823087271131));
#52714=CARTESIAN_POINT('Ctrl Pts',(-50.,-9.22627089118454,12.6404031093252));
#52715=CARTESIAN_POINT('Ctrl Pts',(-50.,-9.31391109124575,12.69736527232));
#52716=CARTESIAN_POINT('Ctrl Pts',(-50.,-9.40266201299437,12.7531750820743));
#52717=CARTESIAN_POINT('Ctrl Pts',(-50.,-9.49261168852801,12.8077483085937));
#52718=CARTESIAN_POINT('Ctrl Pts',(-50.,-9.58387033196931,12.8609845509879));
#52719=CARTESIAN_POINT('Ctrl Pts',(-50.,-9.67650437592402,12.9128185216976));
#52720=CARTESIAN_POINT('Ctrl Pts',(-50.,-9.76056925879954,12.9579257458254));
#52721=CARTESIAN_POINT('Ctrl Pts',(-50.,-9.82661206760692,12.9921270190498));
#52722=CARTESIAN_POINT('Ctrl Pts',(-50.,-9.87400143607813,13.0160785978238));
#52723=CARTESIAN_POINT('Ctrl Pts',(-50.,-9.90234512296736,13.0302030119816));
#52724=CARTESIAN_POINT('Ctrl Pts',(-50.,-9.91144581260293,13.0347177531328));
#52725=CARTESIAN_POINT('',(-50.,-10.9566876228483,12.1692900916743));
#52726=CARTESIAN_POINT('Origin',(-50.,0.,0.));
#52727=CARTESIAN_POINT('',(-50.,-9.76197254719673,10.1221439546065));
#52728=CARTESIAN_POINT('Ctrl Pts',(-50.,-10.9566876228483,12.1692900916743));
#52729=CARTESIAN_POINT('Ctrl Pts',(-50.,-10.9565831961294,12.1688332562504));
#52730=CARTESIAN_POINT('Ctrl Pts',(-50.,-10.9506216542472,12.1427999280076));
#52731=CARTESIAN_POINT('Ctrl Pts',(-50.,-10.9378537570625,12.0923034971696));
#52732=CARTESIAN_POINT('Ctrl Pts',(-50.,-10.9160061370834,12.0199966893985));
#52733=CARTESIAN_POINT('Ctrl Pts',(-50.,-10.8823458677273,11.9289076462876));
#52734=CARTESIAN_POINT('Ctrl Pts',(-50.,-10.8366264238543,11.819132418893));
#52735=CARTESIAN_POINT('Ctrl Pts',(-50.,-10.7906171205087,11.7082443720486));
#52736=CARTESIAN_POINT('Ctrl Pts',(-50.,-10.7457516444569,11.5944243246999));
#52737=CARTESIAN_POINT('Ctrl Pts',(-50.,-10.7016435541469,11.4783016873407));
#52738=CARTESIAN_POINT('Ctrl Pts',(-50.,-10.6569256372063,11.3617725777663));
#52739=CARTESIAN_POINT('Ctrl Pts',(-50.,-10.6098445121699,11.2471610440543));
#52740=CARTESIAN_POINT('Ctrl Pts',(-50.,-10.5590714183695,11.1360616608015));
#52741=CARTESIAN_POINT('Ctrl Pts',(-50.,-10.5039324453602,11.0290666820944));
#52742=CARTESIAN_POINT('Ctrl Pts',(-50.,-10.4442029791024,10.9261704221467));
#52743=CARTESIAN_POINT('Ctrl Pts',(-50.,-10.3800284784999,10.8269681325114));
#52744=CARTESIAN_POINT('Ctrl Pts',(-50.,-10.3117931787431,10.7309623645438));
#52745=CARTESIAN_POINT('Ctrl Pts',(-50.,-10.2400230449985,10.6377349442392));
#52746=CARTESIAN_POINT('Ctrl Pts',(-50.,-10.1653013890907,10.5469256916157));
#52747=CARTESIAN_POINT('Ctrl Pts',(-50.,-10.0881874924486,10.4582479603236));
#52748=CARTESIAN_POINT('Ctrl Pts',(-50.,-10.0091279489326,10.371490948043));
#52749=CARTESIAN_POINT('Ctrl Pts',(-50.,-9.92838949999087,10.2865242878363));
#52750=CARTESIAN_POINT('Ctrl Pts',(-50.,-9.86256723189823,10.2199266327873));
#52751=CARTESIAN_POINT('Ctrl Pts',(-50.,-9.8125301973609,10.1707396505663));
#52752=CARTESIAN_POINT('Ctrl Pts',(-50.,-9.77887468091545,10.1382862065996));
#52753=CARTESIAN_POINT('Ctrl Pts',(-50.,-9.76197254719673,10.1221439546065));
#52754=CARTESIAN_POINT('',(-50.,-10.7151295435653,9.10713484662512));
#52755=CARTESIAN_POINT('Origin',(-50.,0.,0.));
#52756=CARTESIAN_POINT('',(-50.,-12.8416620037784,10.1603317849721));
#52757=CARTESIAN_POINT('Ctrl Pts',(-50.,-10.7151295435653,9.10713484662511));
#52758=CARTESIAN_POINT('Ctrl Pts',(-50.,-10.7299173542433,9.1205004962881));
#52759=CARTESIAN_POINT('Ctrl Pts',(-50.,-10.7595724112169,9.14714733516059));
#52760=CARTESIAN_POINT('Ctrl Pts',(-50.,-10.8042932995341,9.18686421761339));
#52761=CARTESIAN_POINT('Ctrl Pts',(-50.,-10.8643984244951,9.23931258796881));
#52762=CARTESIAN_POINT('Ctrl Pts',(-50.,-10.9403520514449,9.30399043552504));
#52763=CARTESIAN_POINT('Ctrl Pts',(-50.,-11.0172025221741,9.36768097839366));
#52764=CARTESIAN_POINT('Ctrl Pts',(-50.,-11.0950933608815,9.43018117859799));
#52765=CARTESIAN_POINT('Ctrl Pts',(-50.,-11.1742623953034,9.49115310573639));
#52766=CARTESIAN_POINT('Ctrl Pts',(-50.,-11.255055958553,9.55010283362399));
#52767=CARTESIAN_POINT('Ctrl Pts',(-50.,-11.3378501911246,9.60648791406797));
#52768=CARTESIAN_POINT('Ctrl Pts',(-50.,-11.4229782872014,9.65981645609066));
#52769=CARTESIAN_POINT('Ctrl Pts',(-50.,-11.5106598224983,9.70974355202577));
#52770=CARTESIAN_POINT('Ctrl Pts',(-50.,-11.6009173880207,9.75618454891596));
#52771=CARTESIAN_POINT('Ctrl Pts',(-50.,-11.6935310799647,9.79937782767));
#52772=CARTESIAN_POINT('Ctrl Pts',(-50.,-11.7881404490329,9.83975072848667));
#52773=CARTESIAN_POINT('Ctrl Pts',(-50.,-11.8843251688933,9.87781397932795));
#52774=CARTESIAN_POINT('Ctrl Pts',(-50.,-11.9816885786214,9.91405212461268));
#52775=CARTESIAN_POINT('Ctrl Pts',(-50.,-12.079951048189,9.94880133468933));
#52776=CARTESIAN_POINT('Ctrl Pts',(-50.,-12.179003784094,9.98217869512325));
#52777=CARTESIAN_POINT('Ctrl Pts',(-50.,-12.2788457677249,10.0141636803616));
#52778=CARTESIAN_POINT('Ctrl Pts',(-50.,-12.3795413183411,10.0446528139577));
#52779=CARTESIAN_POINT('Ctrl Pts',(-50.,-12.4811722187999,10.0735214401623));
#52780=CARTESIAN_POINT('Ctrl Pts',(-50.,-12.5837865782488,10.1006898014275));
#52781=CARTESIAN_POINT('Ctrl Pts',(-50.,-12.6764281187229,10.123473812926));
#52782=CARTESIAN_POINT('Ctrl Pts',(-50.,-12.7489015820264,10.14017641159));
#52783=CARTESIAN_POINT('Ctrl Pts',(-50.,-12.8007586417669,10.151590250775));
#52784=CARTESIAN_POINT('Ctrl Pts',(-50.,-12.8317244585753,10.1582221321948));
#52785=CARTESIAN_POINT('Ctrl Pts',(-50.,-12.8416620037784,10.1603317849721));
#52786=CARTESIAN_POINT('',(-50.,-13.6388425130122,9.0621520570585));
#52787=CARTESIAN_POINT('Origin',(-50.,0.,0.));
#52788=CARTESIAN_POINT('',(-50.,-11.9725570665522,7.37643433768309));
#52789=CARTESIAN_POINT('Ctrl Pts',(-50.,-13.6388425130122,9.0621520570585));
#52790=CARTESIAN_POINT('Ctrl Pts',(-50.,-13.6386277567007,9.0617355438285));
#52791=CARTESIAN_POINT('Ctrl Pts',(-50.,-13.626379282156,9.03800267564235));
#52792=CARTESIAN_POINT('Ctrl Pts',(-50.,-13.6014545602526,8.99226792994578));
#52793=CARTESIAN_POINT('Ctrl Pts',(-50.,-13.5623113515642,8.92766605565115));
#52794=CARTESIAN_POINT('Ctrl Pts',(-50.,-13.5070556576137,8.84780971091874));
#52795=CARTESIAN_POINT('Ctrl Pts',(-50.,-13.4354725852278,8.7528532374933));
#52796=CARTESIAN_POINT('Ctrl Pts',(-50.,-13.3633320128944,8.65689099100683));
#52797=CARTESIAN_POINT('Ctrl Pts',(-50.,-13.2915701735423,8.557804399923));
#52798=CARTESIAN_POINT('Ctrl Pts',(-50.,-13.2199692944164,8.45629920475326));
#52799=CARTESIAN_POINT('Ctrl Pts',(-50.,-13.1476766619554,8.35455196515643));
#52800=CARTESIAN_POINT('Ctrl Pts',(-50.,-13.0735719476516,8.2552497632047));
#52801=CARTESIAN_POINT('Ctrl Pts',(-50.,-12.9967646908729,8.16026752634251));
#52802=CARTESIAN_POINT('Ctrl Pts',(-50.,-12.9167494409123,8.07034649661759));
#52803=CARTESIAN_POINT('Ctrl Pts',(-50.,-12.8333072263957,7.98553702611316));
#52804=CARTESIAN_POINT('Ctrl Pts',(-50.,-12.7464782795223,7.9054109081407));
#52805=CARTESIAN_POINT('Ctrl Pts',(-50.,-12.6565110535803,7.82939076691323));
#52806=CARTESIAN_POINT('Ctrl Pts',(-50.,-12.5638109939272,7.75694076391353));
#52807=CARTESIAN_POINT('Ctrl Pts',(-50.,-12.4688535134548,7.68756697112423));
#52808=CARTESIAN_POINT('Ctrl Pts',(-50.,-12.3721090366891,7.62085266008235));
#52809=CARTESIAN_POINT('Ctrl Pts',(-50.,-12.2739577025182,7.5564825878338));
#52810=CARTESIAN_POINT('Ctrl Pts',(-50.,-12.174625451278,7.49426414725743));
#52811=CARTESIAN_POINT('Ctrl Pts',(-50.,-12.0943089474566,7.44612811243127));
#52812=CARTESIAN_POINT('Ctrl Pts',(-50.,-12.0336116133124,7.4109301341784));
#52813=CARTESIAN_POINT('Ctrl Pts',(-50.,-11.9929426034861,7.38786606141889));
#52814=CARTESIAN_POINT('Ctrl Pts',(-50.,-11.9725570665522,7.37643433768309));
#52815=CARTESIAN_POINT('',(-50.,-12.6433463826116,6.15627310142281));
#52816=CARTESIAN_POINT('Origin',(-50.,0.,0.));
#52817=CARTESIAN_POINT('',(-50.,-14.9649893429273,6.64753480367511));
#52818=CARTESIAN_POINT('Ctrl Pts',(-50.,-12.6433463826116,6.1562731014228));
#52819=CARTESIAN_POINT('Ctrl Pts',(-50.,-12.6609935089309,6.16554126565498));
#52820=CARTESIAN_POINT('Ctrl Pts',(-50.,-12.6963436971102,6.18397603231157));
#52821=CARTESIAN_POINT('Ctrl Pts',(-50.,-12.7495367835008,6.21132350319834));
#52822=CARTESIAN_POINT('Ctrl Pts',(-50.,-12.8207969747412,6.24717657480866));
#52823=CARTESIAN_POINT('Ctrl Pts',(-50.,-12.9104491054422,6.29093354993378));
#52824=CARTESIAN_POINT('Ctrl Pts',(-50.,-13.0007243712348,6.33351120238525));
#52825=CARTESIAN_POINT('Ctrl Pts',(-50.,-13.0917112937495,6.37467717998103));
#52826=CARTESIAN_POINT('Ctrl Pts',(-50.,-13.1835561890537,6.41404502367149));
#52827=CARTESIAN_POINT('Ctrl Pts',(-50.,-13.2764716751216,6.45105019532836));
#52828=CARTESIAN_POINT('Ctrl Pts',(-50.,-13.3706871739224,6.48507374642914));
#52829=CARTESIAN_POINT('Ctrl Pts',(-50.,-13.4664030834197,6.51555637763196));
#52830=CARTESIAN_POINT('Ctrl Pts',(-50.,-13.5637463059047,6.54210941091933));
#52831=CARTESIAN_POINT('Ctrl Pts',(-50.,-13.6627176703106,6.56464523470766));
#52832=CARTESIAN_POINT('Ctrl Pts',(-50.,-13.7631634644371,6.58344942858329));
#52833=CARTESIAN_POINT('Ctrl Pts',(-50.,-13.8648408383502,6.59902554716193));
#52834=CARTESIAN_POINT('Ctrl Pts',(-50.,-13.9674696839217,6.61197280385553));
#52835=CARTESIAN_POINT('Ctrl Pts',(-50.,-14.0707863033563,6.6228591657896));
#52836=CARTESIAN_POINT('Ctrl Pts',(-50.,-14.1746034538834,6.63207978306306));
#52837=CARTESIAN_POINT('Ctrl Pts',(-50.,-14.278844877945,6.63977511862666));
#52838=CARTESIAN_POINT('Ctrl Pts',(-50.,-14.3835044844334,6.64592554509403));
#52839=CARTESIAN_POINT('Ctrl Pts',(-50.,-14.4886188383546,6.65041484137187));
#52840=CARTESIAN_POINT('Ctrl Pts',(-50.,-14.5942361525827,6.65310192943101));
#52841=CARTESIAN_POINT('Ctrl Pts',(-50.,-14.7003831899324,6.65389759319505));
#52842=CARTESIAN_POINT('Ctrl Pts',(-50.,-14.7957803793054,6.65292678882822));
#52843=CARTESIAN_POINT('Ctrl Pts',(-50.,-14.870130722867,6.65108122722986));
#52844=CARTESIAN_POINT('Ctrl Pts',(-50.,-14.9231971040963,6.64924015333274));
#52845=CARTESIAN_POINT('Ctrl Pts',(-50.,-14.9548393546694,6.64796279651443));
#52846=CARTESIAN_POINT('Ctrl Pts',(-50.,-14.9649893429273,6.64753480367511));
#52847=CARTESIAN_POINT('',(-50.,-15.4640187679296,5.38560568043381));
#52848=CARTESIAN_POINT('Origin',(-50.,0.,0.));
#52849=CARTESIAN_POINT('',(-50.,-13.4308617934315,4.1672362226952));
#52850=CARTESIAN_POINT('Ctrl Pts',(-50.,-15.4640187679296,5.38560568043381));
#52851=CARTESIAN_POINT('Ctrl Pts',(-50.,-15.4637071759544,5.38525566045572));
#52852=CARTESIAN_POINT('Ctrl Pts',(-50.,-15.4459413854495,5.3653144757178));
#52853=CARTESIAN_POINT('Ctrl Pts',(-50.,-15.4104259507712,5.32721509743538));
#52854=CARTESIAN_POINT('Ctrl Pts',(-50.,-15.3564466651341,5.27437732996824));
#52855=CARTESIAN_POINT('Ctrl Pts',(-50.,-15.2830674650563,5.2107713514449));
#52856=CARTESIAN_POINT('Ctrl Pts',(-50.,-15.1901185918597,5.13660009643943));
#52857=CARTESIAN_POINT('Ctrl Pts',(-50.,-15.0963796080126,5.06159331118216));
#52858=CARTESIAN_POINT('Ctrl Pts',(-50.,-15.0022304656484,4.98346615129592));
#52859=CARTESIAN_POINT('Ctrl Pts',(-50.,-14.9076357442716,4.90295634303817));
#52860=CARTESIAN_POINT('Ctrl Pts',(-50.,-14.8123108082616,4.82238412668293));
#52861=CARTESIAN_POINT('Ctrl Pts',(-50.,-14.7158387764281,4.74463077904808));
#52862=CARTESIAN_POINT('Ctrl Pts',(-50.,-14.6178234390918,4.67173377183878));
#52863=CARTESIAN_POINT('Ctrl Pts',(-50.,-14.5179595646104,4.60453676010005));
#52864=CARTESIAN_POINT('Ctrl Pts',(-50.,-14.4160475830522,4.54314296997813));
#52865=CARTESIAN_POINT('Ctrl Pts',(-50.,-14.3120199719745,4.48712764234399));
#52866=CARTESIAN_POINT('Ctrl Pts',(-50.,-14.2059737915295,4.4358697529125));
#52867=CARTESIAN_POINT('Ctrl Pts',(-50.,-14.0981684916428,4.38874946735859));
#52868=CARTESIAN_POINT('Ctrl Pts',(-50.,-13.988941714333,4.34517014494338));
#52869=CARTESIAN_POINT('Ctrl Pts',(-50.,-13.8786454687203,4.30461115967259));
#52870=CARTESIAN_POINT('Ctrl Pts',(-50.,-13.7675695531958,4.26667263583206));
#52871=CARTESIAN_POINT('Ctrl Pts',(-50.,-13.655884910321,4.23111182833087));
#52872=CARTESIAN_POINT('Ctrl Pts',(-50.,-13.5661207520894,4.20446197782756));
#52873=CARTESIAN_POINT('Ctrl Pts',(-50.,-13.4985769550718,4.18546462196559));
#52874=CARTESIAN_POINT('Ctrl Pts',(-50.,-13.4534498353221,4.1732391209285));
#52875=CARTESIAN_POINT('Ctrl Pts',(-50.,-13.4308617934315,4.1672362226952));
#52876=CARTESIAN_POINT('',(-50.,-13.7771352694631,2.8185900760694));
#52877=CARTESIAN_POINT('Origin',(-50.,0.,0.));
#52878=CARTESIAN_POINT('',(-50.,-16.1480113642792,2.71704876274038));
#52879=CARTESIAN_POINT('Ctrl Pts',(-50.,-13.7771352694631,2.81859007606939));
#52880=CARTESIAN_POINT('Ctrl Pts',(-50.,-13.7965328775753,2.82317840202614));
#52881=CARTESIAN_POINT('Ctrl Pts',(-50.,-13.8353570146283,2.83224277227946));
#52882=CARTESIAN_POINT('Ctrl Pts',(-50.,-13.8936799818437,2.84550248942744));
#52883=CARTESIAN_POINT('Ctrl Pts',(-50.,-13.9716176994713,2.862507481945));
#52884=CARTESIAN_POINT('Ctrl Pts',(-50.,-14.0693351608341,2.882594172965));
#52885=CARTESIAN_POINT('Ctrl Pts',(-50.,-14.1673628947312,2.90138362450613));
#52886=CARTESIAN_POINT('Ctrl Pts',(-50.,-14.2657288580852,2.91862876972314));
#52887=CARTESIAN_POINT('Ctrl Pts',(-50.,-14.3644786617177,2.93391890356181));
#52888=CARTESIAN_POINT('Ctrl Pts',(-50.,-14.463677848895,2.94665434795724));
#52889=CARTESIAN_POINT('Ctrl Pts',(-50.,-14.5633947076351,2.95617854486928));
#52890=CARTESIAN_POINT('Ctrl Pts',(-50.,-14.6636842479405,2.96189992942649));
#52891=CARTESIAN_POINT('Ctrl Pts',(-50.,-14.7645727249416,2.96341047532946));
#52892=CARTESIAN_POINT('Ctrl Pts',(-50.,-14.8660391534142,2.96062511732634));
#52893=CARTESIAN_POINT('Ctrl Pts',(-50.,-14.9680056710645,2.95385868966535));
#52894=CARTESIAN_POINT('Ctrl Pts',(-50.,-15.0703622864763,2.94365932119071));
#52895=CARTESIAN_POINT('Ctrl Pts',(-50.,-15.1729867099492,2.9306770599819));
#52896=CARTESIAN_POINT('Ctrl Pts',(-50.,-15.2757647759192,2.91552760840775));
#52897=CARTESIAN_POINT('Ctrl Pts',(-50.,-15.3786133940255,2.89864026758367));
#52898=CARTESIAN_POINT('Ctrl Pts',(-50.,-15.4814936341966,2.88017005204204));
#52899=CARTESIAN_POINT('Ctrl Pts',(-50.,-15.5843947155558,2.86009946582377));
#52900=CARTESIAN_POINT('Ctrl Pts',(-50.,-15.6873231513416,2.83830684578773));
#52901=CARTESIAN_POINT('Ctrl Pts',(-50.,-15.7902905550528,2.81464355607623));
#52902=CARTESIAN_POINT('Ctrl Pts',(-50.,-15.8933006615651,2.78901652785862));
#52903=CARTESIAN_POINT('Ctrl Pts',(-50.,-15.9854593435823,2.76435190683515));
#52904=CARTESIAN_POINT('Ctrl Pts',(-50.,-16.0570148618746,2.74407414839715));
#52905=CARTESIAN_POINT('Ctrl Pts',(-50.,-16.1079562086956,2.72909384286184));
#52906=CARTESIAN_POINT('Ctrl Pts',(-50.,-16.1382866940579,2.7199875088322));
#52907=CARTESIAN_POINT('Ctrl Pts',(-50.,-16.1480113642792,2.71704876274038));
#52908=CARTESIAN_POINT('',(-50.,-16.3175338509752,1.37066189203528));
#52909=CARTESIAN_POINT('Origin',(-50.,0.,0.));
#52910=CARTESIAN_POINT('',(-50.,-14.045256078575,0.696195329812624));
#52911=CARTESIAN_POINT('Ctrl Pts',(-50.,-16.3175338509752,1.37066189203528));
#52912=CARTESIAN_POINT('Ctrl Pts',(-50.,-16.317145001806,1.37040035835161));
#52913=CARTESIAN_POINT('Ctrl Pts',(-50.,-16.2949781852964,1.35550383503756));
#52914=CARTESIAN_POINT('Ctrl Pts',(-50.,-16.2511036032208,1.32743374822648));
#52915=CARTESIAN_POINT('Ctrl Pts',(-50.,-16.1856799576735,1.28968007884051));
#52916=CARTESIAN_POINT('Ctrl Pts',(-50.,-16.0987879364791,1.2463210640833));
#52917=CARTESIAN_POINT('Ctrl Pts',(-50.,-15.9903135820168,1.19759548023257));
#52918=CARTESIAN_POINT('Ctrl Pts',(-50.,-15.8808661517589,1.14825710837788));
#52919=CARTESIAN_POINT('Ctrl Pts',(-50.,-15.7702454432537,1.09599839647648));
#52920=CARTESIAN_POINT('Ctrl Pts',(-50.,-15.6586006138651,1.04154270247793));
#52921=CARTESIAN_POINT('Ctrl Pts',(-50.,-15.5462329906162,0.987208158041752));
#52922=CARTESIAN_POINT('Ctrl Pts',(-50.,-15.4334553338124,0.935889193512498));
#52923=CARTESIAN_POINT('Ctrl Pts',(-50.,-15.3203905800386,0.889657803015486));
#52924=CARTESIAN_POINT('Ctrl Pts',(-50.,-15.2069528955437,0.849407044643804));
#52925=CARTESIAN_POINT('Ctrl Pts',(-50.,-15.0929746515511,0.81528653252832));
#52926=CARTESIAN_POINT('Ctrl Pts',(-50.,-14.97828481366,0.786901644277719));
#52927=CARTESIAN_POINT('Ctrl Pts',(-50.,-14.8628229502399,0.763626728348506));
#52928=CARTESIAN_POINT('Ctrl Pts',(-50.,-14.7466862135917,0.744796901078022));
#52929=CARTESIAN_POINT('Ctrl Pts',(-50.,-14.6300532595709,0.7297502981378));
#52930=CARTESIAN_POINT('Ctrl Pts',(-50.,-14.5131355638642,0.717895108848178));
#52931=CARTESIAN_POINT('Ctrl Pts',(-50.,-14.3961143752671,0.708771950396692));
#52932=CARTESIAN_POINT('Ctrl Pts',(-50.,-14.279094897617,0.702103192289484));
#52933=CARTESIAN_POINT('Ctrl Pts',(-50.,-14.1855232971663,0.698614034227448));
#52934=CARTESIAN_POINT('Ctrl Pts',(-50.,-14.1153770624506,0.697010974492569));
#52935=CARTESIAN_POINT('Ctrl Pts',(-50.,-14.0686273356774,0.696392218370307));
#52936=CARTESIAN_POINT('Ctrl Pts',(-50.,-14.045256078575,0.696195329812624));
#52937=CARTESIAN_POINT('',(-50.,-14.045256078575,-0.696195329812616));
#52938=CARTESIAN_POINT('Origin',(-50.,0.,0.));
#52939=CARTESIAN_POINT('',(-50.,-16.3163944433819,-1.38415944456368));
#52940=CARTESIAN_POINT('Ctrl Pts',(-50.,-14.045256078575,-0.696195329812629));
#52941=CARTESIAN_POINT('Ctrl Pts',(-50.,-14.0651853454231,-0.696575143525857));
#52942=CARTESIAN_POINT('Ctrl Pts',(-50.,-14.1050439680336,-0.697450717395246));
#52943=CARTESIAN_POINT('Ctrl Pts',(-50.,-14.1648321695468,-0.699111910780302));
#52944=CARTESIAN_POINT('Ctrl Pts',(-50.,-14.2445503001281,-0.702023483575367));
#52945=CARTESIAN_POINT('Ctrl Pts',(-50.,-14.3441931446757,-0.706869197330954));
#52946=CARTESIAN_POINT('Ctrl Pts',(-50.,-14.4438139036356,-0.71304855704325));
#52947=CARTESIAN_POINT('Ctrl Pts',(-50.,-14.5433782125866,-0.72080782010221));
#52948=CARTESIAN_POINT('Ctrl Pts',(-50.,-14.6428281112089,-0.730556131457601));
#52949=CARTESIAN_POINT('Ctrl Pts',(-50.,-14.7420779497362,-0.742890629132665));
#52950=CARTESIAN_POINT('Ctrl Pts',(-50.,-14.8410305914479,-0.758464226728878));
#52951=CARTESIAN_POINT('Ctrl Pts',(-50.,-14.939592201905,-0.777863584450799));
#52952=CARTESIAN_POINT('Ctrl Pts',(-50.,-15.0376867393704,-0.801490439086723));
#52953=CARTESIAN_POINT('Ctrl Pts',(-50.,-15.1352727230412,-0.829421964594113));
#52954=CARTESIAN_POINT('Ctrl Pts',(-50.,-15.2323530329047,-0.861333854256595));
#52955=CARTESIAN_POINT('Ctrl Pts',(-50.,-15.3289574472276,-0.89666784595261));
#52956=CARTESIAN_POINT('Ctrl Pts',(-50.,-15.4251291786488,-0.934763901846662));
#52957=CARTESIAN_POINT('Ctrl Pts',(-50.,-15.5209107672782,-0.974997271170846));
#52958=CARTESIAN_POINT('Ctrl Pts',(-50.,-15.6163284960372,-1.01693147636119));
#52959=CARTESIAN_POINT('Ctrl Pts',(-50.,-15.7113832084608,-1.06040669143688));
#52960=CARTESIAN_POINT('Ctrl Pts',(-50.,-15.8060601113054,-1.10543718159424));
#52961=CARTESIAN_POINT('Ctrl Pts',(-50.,-15.900335256791,-1.15214240747963));
#52962=CARTESIAN_POINT('Ctrl Pts',(-50.,-15.9941829293225,-1.20066922344171));
#52963=CARTESIAN_POINT('Ctrl Pts',(-50.,-16.0875836011606,-1.25110870320843));
#52964=CARTESIAN_POINT('Ctrl Pts',(-50.,-16.170713106895,-1.29791737203952));
#52965=CARTESIAN_POINT('Ctrl Pts',(-50.,-16.2349777035408,-1.33535320117812));
#52966=CARTESIAN_POINT('Ctrl Pts',(-50.,-16.2805931837835,-1.36253147066111));
#52967=CARTESIAN_POINT('Ctrl Pts',(-50.,-16.307706127992,-1.37889459744425));
#52968=CARTESIAN_POINT('Ctrl Pts',(-50.,-16.3163944433819,-1.38415944456368));
#52969=CARTESIAN_POINT('',(-50.,-16.1457582704724,-2.73040562398164));
#52970=CARTESIAN_POINT('Origin',(-50.,0.,0.));
#52971=CARTESIAN_POINT('',(-50.,-13.7771352694631,-2.8185900760694));
#52972=CARTESIAN_POINT('Ctrl Pts',(-50.,-16.1457582704724,-2.73040562398164));
#52973=CARTESIAN_POINT('Ctrl Pts',(-50.,-16.1453165969326,-2.73056223824769));
#52974=CARTESIAN_POINT('Ctrl Pts',(-50.,-16.1201415770235,-2.73947809679247));
#52975=CARTESIAN_POINT('Ctrl Pts',(-50.,-16.0706646489018,-2.75575514534332));
#52976=CARTESIAN_POINT('Ctrl Pts',(-50.,-15.9979074517054,-2.77605251475231));
#52977=CARTESIAN_POINT('Ctrl Pts',(-50.,-15.9029623546524,-2.7964401593829));
#52978=CARTESIAN_POINT('Ctrl Pts',(-50.,-15.7857783615561,-2.81665846444538));
#52979=CARTESIAN_POINT('Ctrl Pts',(-50.,-15.6674994694501,-2.83722831154002));
#52980=CARTESIAN_POINT('Ctrl Pts',(-50.,-15.5473579007536,-2.86033496839371));
#52981=CARTESIAN_POINT('Ctrl Pts',(-50.,-15.4256780185848,-2.88531489660512));
#52982=CARTESIAN_POINT('Ctrl Pts',(-50.,-15.3033281791249,-2.90999772986683));
#52983=CARTESIAN_POINT('Ctrl Pts',(-50.,-15.181331132295,-2.93165775201116));
#52984=CARTESIAN_POINT('Ctrl Pts',(-50.,-15.0603212363863,-2.9483186375038));
#52985=CARTESIAN_POINT('Ctrl Pts',(-50.,-14.9404374487894,-2.959094039328));
#52986=CARTESIAN_POINT('Ctrl Pts',(-50.,-14.8215546146151,-2.96379735617437));
#52987=CARTESIAN_POINT('Ctrl Pts',(-50.,-14.703408934225,-2.96276827812033));
#52988=CARTESIAN_POINT('Ctrl Pts',(-50.,-14.5857862813476,-2.95659777198027));
#52989=CARTESIAN_POINT('Ctrl Pts',(-50.,-14.4686154062224,-2.94595399366867));
#52990=CARTESIAN_POINT('Ctrl Pts',(-50.,-14.3519047529378,-2.93152244373364));
#52991=CARTESIAN_POINT('Ctrl Pts',(-50.,-14.2357119759516,-2.91392893189869));
#52992=CARTESIAN_POINT('Ctrl Pts',(-50.,-14.1200983859353,-2.89366348336299));
#52993=CARTESIAN_POINT('Ctrl Pts',(-50.,-14.0050968376581,-2.87102116947837));
#52994=CARTESIAN_POINT('Ctrl Pts',(-50.,-13.913597242777,-2.85113039846586));
#52995=CARTESIAN_POINT('Ctrl Pts',(-50.,-13.8452561162702,-2.83523843593487));
#52996=CARTESIAN_POINT('Ctrl Pts',(-50.,-13.7998212397401,-2.82421156841951));
#52997=CARTESIAN_POINT('Ctrl Pts',(-50.,-13.7771352694631,-2.8185900760694));
#52998=CARTESIAN_POINT('',(-50.,-13.4308617934315,-4.16723622269519));
#52999=CARTESIAN_POINT('Origin',(-50.,0.,0.));
#53000=CARTESIAN_POINT('',(-50.,-15.4595584521058,-5.39839582338345));
#53001=CARTESIAN_POINT('Ctrl Pts',(-50.,-13.4308617934315,-4.1672362226952));
#53002=CARTESIAN_POINT('Ctrl Pts',(-50.,-13.4500704898848,-4.17256031098595));
#53003=CARTESIAN_POINT('Ctrl Pts',(-50.,-13.4884591342042,-4.1833208134517));
#53004=CARTESIAN_POINT('Ctrl Pts',(-50.,-13.5459558574286,-4.19979853847996));
#53005=CARTESIAN_POINT('Ctrl Pts',(-50.,-13.6224454176364,-4.22244373176092));
#53006=CARTESIAN_POINT('Ctrl Pts',(-50.,-13.717752718985,-4.25191737627554));
#53007=CARTESIAN_POINT('Ctrl Pts',(-50.,-13.8127069643429,-4.28267727534445));
#53008=CARTESIAN_POINT('Ctrl Pts',(-50.,-13.9072136271877,-4.31495340364481));
#53009=CARTESIAN_POINT('Ctrl Pts',(-50.,-14.0011148179182,-4.34912763794002));
#53010=CARTESIAN_POINT('Ctrl Pts',(-50.,-14.0941790754254,-4.38575705583354));
#53011=CARTESIAN_POINT('Ctrl Pts',(-50.,-14.1861499417075,-4.42544990152536));
#53012=CARTESIAN_POINT('Ctrl Pts',(-50.,-14.2767906338471,-4.4687510685349));
#53013=CARTESIAN_POINT('Ctrl Pts',(-50.,-14.3659275912213,-4.51603076153944));
#53014=CARTESIAN_POINT('Ctrl Pts',(-50.,-14.4535014438403,-4.56735341407851));
#53015=CARTESIAN_POINT('Ctrl Pts',(-50.,-14.5395956330118,-4.62240562435127));
#53016=CARTESIAN_POINT('Ctrl Pts',(-50.,-14.6243778356077,-4.68065407462106));
#53017=CARTESIAN_POINT('Ctrl Pts',(-50.,-14.7080540513971,-4.74147020990105));
#53018=CARTESIAN_POINT('Ctrl Pts',(-50.,-14.7908208532122,-4.80425948641264));
#53019=CARTESIAN_POINT('Ctrl Pts',(-50.,-14.8728122458042,-4.86860567563393));
#53020=CARTESIAN_POINT('Ctrl Pts',(-50.,-14.954068793312,-4.9343541825898));
#53021=CARTESIAN_POINT('Ctrl Pts',(-50.,-15.0345726196388,-5.00151514537911));
#53022=CARTESIAN_POINT('Ctrl Pts',(-50.,-15.1142708207137,-5.07019831600168));
#53023=CARTESIAN_POINT('Ctrl Pts',(-50.,-15.1931019676527,-5.14053953989829));
#53024=CARTESIAN_POINT('Ctrl Pts',(-50.,-15.2710244971014,-5.21262217319695));
#53025=CARTESIAN_POINT('Ctrl Pts',(-50.,-15.3399014939787,-5.27863372902275));
#53026=CARTESIAN_POINT('Ctrl Pts',(-50.,-15.3928371880222,-5.33087539803783));
#53027=CARTESIAN_POINT('Ctrl Pts',(-50.,-15.430260613301,-5.36854392084221));
#53028=CARTESIAN_POINT('Ctrl Pts',(-50.,-15.4524524103566,-5.39113568494369));
#53029=CARTESIAN_POINT('Ctrl Pts',(-50.,-15.4595584521058,-5.39839582338345));
#53030=CARTESIAN_POINT('',(-50.,-14.9594853178907,-6.65991171291435));
#53031=CARTESIAN_POINT('Origin',(-50.,0.,0.));
#53032=CARTESIAN_POINT('',(-50.,-12.6433463826116,-6.1562731014228));
#53033=CARTESIAN_POINT('Ctrl Pts',(-50.,-14.9594853178907,-6.65991171291435));
#53034=CARTESIAN_POINT('Ctrl Pts',(-50.,-14.9590185719531,-6.65995356711246));
#53035=CARTESIAN_POINT('Ctrl Pts',(-50.,-14.9324171877326,-6.66232854470537));
#53036=CARTESIAN_POINT('Ctrl Pts',(-50.,-14.880446730922,-6.66578980817273));
#53037=CARTESIAN_POINT('Ctrl Pts',(-50.,-14.8049275843586,-6.66735551923628));
#53038=CARTESIAN_POINT('Ctrl Pts',(-50.,-14.7078951610787,-6.6634907630476));
#53039=CARTESIAN_POINT('Ctrl Pts',(-50.,-14.5893646306071,-6.65393139885702));
#53040=CARTESIAN_POINT('Ctrl Pts',(-50.,-14.4696861744433,-6.64444024204806));
#53041=CARTESIAN_POINT('Ctrl Pts',(-50.,-14.3475726821666,-6.63694296762358));
#53042=CARTESIAN_POINT('Ctrl Pts',(-50.,-14.2235033417215,-6.63087754928856));
#53043=CARTESIAN_POINT('Ctrl Pts',(-50.,-14.0988589764351,-6.62435775818486));
#53044=CARTESIAN_POINT('Ctrl Pts',(-50.,-13.9753080627051,-6.61499785909296));
#53045=CARTESIAN_POINT('Ctrl Pts',(-50.,-13.8539565214648,-6.60104137487127));
#53046=CARTESIAN_POINT('Ctrl Pts',(-50.,-13.7351593700424,-6.58166436202222));
#53047=CARTESIAN_POINT('Ctrl Pts',(-50.,-13.6188417913781,-6.55665495690443));
#53048=CARTESIAN_POINT('Ctrl Pts',(-50.,-13.5046637960973,-6.52627657330457));
#53049=CARTESIAN_POINT('Ctrl Pts',(-50.,-13.3922710176287,-6.49104836068956));
#53050=CARTESIAN_POINT('Ctrl Pts',(-50.,-13.281428281035,-6.45159976453225));
#53051=CARTESIAN_POINT('Ctrl Pts',(-50.,-13.1719732880642,-6.40859684907992));
#53052=CARTESIAN_POINT('Ctrl Pts',(-50.,-13.0638062493037,-6.3626601011734));
#53053=CARTESIAN_POINT('Ctrl Pts',(-50.,-12.9568646849259,-6.31427939831312));
#53054=CARTESIAN_POINT('Ctrl Pts',(-50.,-12.851107036246,-6.26374871229064));
#53055=CARTESIAN_POINT('Ctrl Pts',(-50.,-12.7674287029928,-6.22172782249946));
#53056=CARTESIAN_POINT('Ctrl Pts',(-50.,-12.7051868090144,-6.18933938815496));
#53057=CARTESIAN_POINT('Ctrl Pts',(-50.,-12.6639216231176,-6.16735975564195));
#53058=CARTESIAN_POINT('Ctrl Pts',(-50.,-12.6433463826116,-6.1562731014228));
#53059=CARTESIAN_POINT('',(-50.,-11.9725570665522,-7.37643433768308));
#53060=CARTESIAN_POINT('Origin',(-50.,0.,0.));
#53061=CARTESIAN_POINT('',(-50.,-13.631341547005,-9.07343113870902));
#53062=CARTESIAN_POINT('Ctrl Pts',(-50.,-11.9725570665522,-7.37643433768309));
#53063=CARTESIAN_POINT('Ctrl Pts',(-50.,-11.9898382395678,-7.38636816850343));
#53064=CARTESIAN_POINT('Ctrl Pts',(-50.,-12.0243448058902,-7.40633747762124));
#53065=CARTESIAN_POINT('Ctrl Pts',(-50.,-12.0759373202474,-7.43659637822836));
#53066=CARTESIAN_POINT('Ctrl Pts',(-50.,-12.144392189705,-7.47755231121817));
#53067=CARTESIAN_POINT('Ctrl Pts',(-50.,-12.2293754395952,-7.5298019490105));
#53068=CARTESIAN_POINT('Ctrl Pts',(-50.,-12.3136968468978,-7.58320962985052));
#53069=CARTESIAN_POINT('Ctrl Pts',(-50.,-12.3972076624386,-7.63797459554787));
#53070=CARTESIAN_POINT('Ctrl Pts',(-50.,-12.4796599881192,-7.69442745995809));
#53071=CARTESIAN_POINT('Ctrl Pts',(-50.,-12.5606910950408,-7.75305023703025));
#53072=CARTESIAN_POINT('Ctrl Pts',(-50.,-12.6399013181197,-7.81436828334278));
#53073=CARTESIAN_POINT('Ctrl Pts',(-50.,-12.7169258039014,-7.87885048806616));
#53074=CARTESIAN_POINT('Ctrl Pts',(-50.,-12.7915043783298,-7.9468122624453));
#53075=CARTESIAN_POINT('Ctrl Pts',(-50.,-12.8635635126628,-8.01830125100551));
#53076=CARTESIAN_POINT('Ctrl Pts',(-50.,-12.9332619666045,-8.09303464904925));
#53077=CARTESIAN_POINT('Ctrl Pts',(-50.,-13.0008947798771,-8.17053759353955));
#53078=CARTESIAN_POINT('Ctrl Pts',(-50.,-13.0668177956572,-8.25025250675973));
#53079=CARTESIAN_POINT('Ctrl Pts',(-50.,-13.1313692681049,-8.3316524092927));
#53080=CARTESIAN_POINT('Ctrl Pts',(-50.,-13.1947825037901,-8.41436747482742));
#53081=CARTESIAN_POINT('Ctrl Pts',(-50.,-13.2571352386615,-8.49825805316535));
#53082=CARTESIAN_POINT('Ctrl Pts',(-50.,-13.3184076369901,-8.58332951829382));
#53083=CARTESIAN_POINT('Ctrl Pts',(-50.,-13.3785211625712,-8.66967501744431));
#53084=CARTESIAN_POINT('Ctrl Pts',(-50.,-13.4373825330349,-8.7574108514811));
#53085=CARTESIAN_POINT('Ctrl Pts',(-50.,-13.4949307609898,-8.84660742136017));
#53086=CARTESIAN_POINT('Ctrl Pts',(-50.,-13.5452274539844,-8.92767411535463));
#53087=CARTESIAN_POINT('Ctrl Pts',(-50.,-13.5835081010849,-8.99143908805054));
#53088=CARTESIAN_POINT('Ctrl Pts',(-50.,-13.6103880199559,-9.03723101235338));
#53089=CARTESIAN_POINT('Ctrl Pts',(-50.,-13.6262642776339,-9.06463189014802));
#53090=CARTESIAN_POINT('Ctrl Pts',(-50.,-13.631341547005,-9.07343113870902));
#53091=CARTESIAN_POINT('',(-50.,-12.8332528856473,-10.1709510554827));
#53092=CARTESIAN_POINT('Origin',(-50.,0.,0.));
#53093=CARTESIAN_POINT('',(-50.,-10.7151295435653,-9.10713484662511));
#53094=CARTESIAN_POINT('Ctrl Pts',(-50.,-12.8332528856473,-10.1709510554827));
#53095=CARTESIAN_POINT('Ctrl Pts',(-50.,-12.8327903946759,-10.1708755197597));
#53096=CARTESIAN_POINT('Ctrl Pts',(-50.,-12.8064341089476,-10.166560387824));
#53097=CARTESIAN_POINT('Ctrl Pts',(-50.,-12.7552356183835,-10.1569883822946));
#53098=CARTESIAN_POINT('Ctrl Pts',(-50.,-12.6816996681717,-10.1397240556283));
#53099=CARTESIAN_POINT('Ctrl Pts',(-50.,-12.5886768226797,-10.1118497354652));
#53100=CARTESIAN_POINT('Ctrl Pts',(-50.,-12.4762474639872,-10.0731133520306));
#53101=CARTESIAN_POINT('Ctrl Pts',(-50.,-12.362689281313,-10.0341575556064));
#53102=CARTESIAN_POINT('Ctrl Pts',(-50.,-12.2462767052779,-9.99652743122885));
#53103=CARTESIAN_POINT('Ctrl Pts',(-50.,-12.1276136395118,-9.95979777888845));
#53104=CARTESIAN_POINT('Ctrl Pts',(-50.,-12.0085066122796,-9.9224850258725));
#53105=CARTESIAN_POINT('Ctrl Pts',(-50.,-11.8911649899478,-9.88269332242761));
#53106=CARTESIAN_POINT('Ctrl Pts',(-50.,-11.7770967670118,-9.83899640572359));
#53107=CARTESIAN_POINT('Ctrl Pts',(-50.,-11.6668507136929,-9.79068450718227));
#53108=CARTESIAN_POINT('Ctrl Pts',(-50.,-11.5604070517922,-9.73753381300202));
#53109=CARTESIAN_POINT('Ctrl Pts',(-50.,-11.4573709649815,-9.6797149094218));
#53110=CARTESIAN_POINT('Ctrl Pts',(-50.,-11.3572701125446,-9.61764250849074));
#53111=CARTESIAN_POINT('Ctrl Pts',(-50.,-11.2597201712738,-9.55186779486609));
#53112=CARTESIAN_POINT('Ctrl Pts',(-50.,-11.1643982983724,-9.48299554522798));
#53113=CARTESIAN_POINT('Ctrl Pts',(-50.,-11.0710535306934,-9.4116019360644));
#53114=CARTESIAN_POINT('Ctrl Pts',(-50.,-10.9795035237476,-9.33814591637203));
#53115=CARTESIAN_POINT('Ctrl Pts',(-50.,-10.889634916681,-9.26290188705335));
#53116=CARTESIAN_POINT('Ctrl Pts',(-50.,-10.8190356624814,-9.20139120553108));
#53117=CARTESIAN_POINT('Ctrl Pts',(-50.,-10.7668038881397,-9.15454138381928));
#53118=CARTESIAN_POINT('Ctrl Pts',(-50.,-10.7323012362688,-9.12299004745485));
#53119=CARTESIAN_POINT('Ctrl Pts',(-50.,-10.7151295435653,-9.10713484662511));
#53120=CARTESIAN_POINT('',(-50.,-9.76197254719673,-10.1221439546065));
#53121=CARTESIAN_POINT('Origin',(-50.,0.,0.));
#53122=CARTESIAN_POINT('',(-50.,-10.9466173199385,-12.178349405844));
#53123=CARTESIAN_POINT('Ctrl Pts',(-50.,-9.76197254719672,-10.1221439546065));
#53124=CARTESIAN_POINT('Ctrl Pts',(-50.,-9.77624035711837,-10.1360633488319));
#53125=CARTESIAN_POINT('Ctrl Pts',(-50.,-9.80469667097528,-10.163986719468));
#53126=CARTESIAN_POINT('Ctrl Pts',(-50.,-9.84714322904426,-10.2061255176443));
#53127=CARTESIAN_POINT('Ctrl Pts',(-50.,-9.90326213654415,-10.2628187784479));
#53128=CARTESIAN_POINT('Ctrl Pts',(-50.,-9.97258152483879,-10.3345613726147));
#53129=CARTESIAN_POINT('Ctrl Pts',(-50.,-10.0409718699529,-10.4072610342189));
#53130=CARTESIAN_POINT('Ctrl Pts',(-50.,-10.108239546518,-10.4810737531071));
#53131=CARTESIAN_POINT('Ctrl Pts',(-50.,-10.1740622242879,-10.5562581065423));
#53132=CARTESIAN_POINT('Ctrl Pts',(-50.,-10.2379686981643,-10.6331907581101));
#53133=CARTESIAN_POINT('Ctrl Pts',(-50.,-10.2994412084092,-10.7122811666816));
#53134=CARTESIAN_POINT('Ctrl Pts',(-50.,-10.3580097561152,-10.7938927550471));
#53135=CARTESIAN_POINT('Ctrl Pts',(-50.,-10.4133439014856,-10.8782663225706));
#53136=CARTESIAN_POINT('Ctrl Pts',(-50.,-10.4653605771075,-10.9654297310826));
#53137=CARTESIAN_POINT('Ctrl Pts',(-50.,-10.5142838856252,-11.055148542648));
#53138=CARTESIAN_POINT('Ctrl Pts',(-50.,-10.5605176911805,-11.1470361863206));
#53139=CARTESIAN_POINT('Ctrl Pts',(-50.,-10.6045453214218,-11.2406410963124));
#53140=CARTESIAN_POINT('Ctrl Pts',(-50.,-10.6468254580846,-11.3355369696227));
#53141=CARTESIAN_POINT('Ctrl Pts',(-50.,-10.6876760500473,-11.4314236196986));
#53142=CARTESIAN_POINT('Ctrl Pts',(-50.,-10.727207120633,-11.5281851158537));
#53143=CARTESIAN_POINT('Ctrl Pts',(-50.,-10.7653981208323,-11.6258217302963));
#53144=CARTESIAN_POINT('Ctrl Pts',(-50.,-10.8021498170253,-11.7244041527066));
#53145=CARTESIAN_POINT('Ctrl Pts',(-50.,-10.8373429346305,-11.8240218317612));
#53146=CARTESIAN_POINT('Ctrl Pts',(-50.,-10.8709008942817,-11.9247277896931));
#53147=CARTESIAN_POINT('Ctrl Pts',(-50.,-10.8994569571944,-12.0157559033301));
#53148=CARTESIAN_POINT('Ctrl Pts',(-50.,-10.9206772435082,-12.0870375919612));
#53149=CARTESIAN_POINT('Ctrl Pts',(-50.,-10.9353246918112,-12.1380756427477));
#53150=CARTESIAN_POINT('Ctrl Pts',(-50.,-10.9438878464529,-12.1685639363102));
#53151=CARTESIAN_POINT('Ctrl Pts',(-50.,-10.9466173199385,-12.178349405844));
#53152=CARTESIAN_POINT('',(-50.,-9.90065997719615,-13.0429121370937));
#53153=CARTESIAN_POINT('Origin',(-50.,0.,0.));
#53154=CARTESIAN_POINT('',(-50.,-8.11364170780698,-11.4857618157149));
#53155=CARTESIAN_POINT('Ctrl Pts',(-50.,-9.90065997719615,-13.0429121370937));
#53156=CARTESIAN_POINT('Ctrl Pts',(-50.,-9.90023080119949,-13.0427239576368));
#53157=CARTESIAN_POINT('Ctrl Pts',(-50.,-9.87577567632734,-13.031989851782));
#53158=CARTESIAN_POINT('Ctrl Pts',(-50.,-9.82856614146686,-13.0099860215666));
#53159=CARTESIAN_POINT('Ctrl Pts',(-50.,-9.76163392180467,-12.9749764383087));
#53160=CARTESIAN_POINT('Ctrl Pts',(-50.,-9.67846562159703,-12.9248440002217));
#53161=CARTESIAN_POINT('Ctrl Pts',(-50.,-9.57920178477654,-12.8593645469766));
#53162=CARTESIAN_POINT('Ctrl Pts',(-50.,-9.47889915384706,-12.7933918468958));
#53163=CARTESIAN_POINT('Ctrl Pts',(-50.,-9.37550212434126,-12.7279933116739));
#53164=CARTESIAN_POINT('Ctrl Pts',(-50.,-9.26970137008846,-12.6629072844668));
#53165=CARTESIAN_POINT('Ctrl Pts',(-50.,-9.16361561347667,-12.5971460670373));
#53166=CARTESIAN_POINT('Ctrl Pts',(-50.,-9.05985628822634,-12.5294228183105));
#53167=CARTESIAN_POINT('Ctrl Pts',(-50.,-8.96023870955522,-12.4587311071067));
#53168=CARTESIAN_POINT('Ctrl Pts',(-50.,-8.86547091932666,-12.3845199371372));
#53169=CARTESIAN_POINT('Ctrl Pts',(-50.,-8.77558942093922,-12.3065676074844));
#53170=CARTESIAN_POINT('Ctrl Pts',(-50.,-8.69016937887314,-12.2249411582788));
#53171=CARTESIAN_POINT('Ctrl Pts',(-50.,-8.60865015717173,-12.1399248062686));
#53172=CARTESIAN_POINT('Ctrl Pts',(-50.,-8.53052243279731,-12.0519568423361));
#53173=CARTESIAN_POINT('Ctrl Pts',(-50.,-8.45532310380908,-11.9615427552514));
#53174=CARTESIAN_POINT('Ctrl Pts',(-50.,-8.3826658022629,-11.8691782078618));
#53175=CARTESIAN_POINT('Ctrl Pts',(-50.,-8.3122597763829,-11.775262383207));
#53176=CARTESIAN_POINT('Ctrl Pts',(-50.,-8.24392698602517,-11.6800328696824));
#53177=CARTESIAN_POINT('Ctrl Pts',(-50.,-8.19084282166638,-11.6028973387695));
#53178=CARTESIAN_POINT('Ctrl Pts',(-50.,-8.15190308143842,-11.5445298762901));
#53179=CARTESIAN_POINT('Ctrl Pts',(-50.,-8.12633089210227,-11.5053893225758));
#53180=CARTESIAN_POINT('Ctrl Pts',(-50.,-8.11364170780698,-11.4857618157149));
#53181=CARTESIAN_POINT('',(-50.,-6.93800739067722,-12.2318420402206));
#53182=CARTESIAN_POINT('Origin',(-50.,0.,0.));
#53183=CARTESIAN_POINT('',(-50.,-7.57407686781798,-14.5180571909737));
#53184=CARTESIAN_POINT('Ctrl Pts',(-50.,-6.93800739067721,-12.2318420402206));
#53185=CARTESIAN_POINT('Ctrl Pts',(-50.,-6.94836533853418,-12.24887239112));
#53186=CARTESIAN_POINT('Ctrl Pts',(-50.,-6.96898338507103,-12.2829952952022));
#53187=CARTESIAN_POINT('Ctrl Pts',(-50.,-6.99961691350077,-12.3343662552827));
#53188=CARTESIAN_POINT('Ctrl Pts',(-50.,-7.03987370169386,-12.4032345978205));
#53189=CARTESIAN_POINT('Ctrl Pts',(-50.,-7.08917363628753,-12.4899622973194));
#53190=CARTESIAN_POINT('Ctrl Pts',(-50.,-7.13733570230759,-12.5773859525787));
#53191=CARTESIAN_POINT('Ctrl Pts',(-50.,-7.18413356438513,-12.6656085000656));
#53192=CARTESIAN_POINT('Ctrl Pts',(-50.,-7.22919071332107,-12.7548002330908));
#53193=CARTESIAN_POINT('Ctrl Pts',(-50.,-7.27195707536722,-12.8452087977179));
#53194=CARTESIAN_POINT('Ctrl Pts',(-50.,-7.31182932887926,-12.9371020273035));
#53195=CARTESIAN_POINT('Ctrl Pts',(-50.,-7.34826186125705,-13.0307150430677));
#53196=CARTESIAN_POINT('Ctrl Pts',(-50.,-7.38087472971119,-13.1261989021839));
#53197=CARTESIAN_POINT('Ctrl Pts',(-50.,-7.40958054758866,-13.2235599331263));
#53198=CARTESIAN_POINT('Ctrl Pts',(-50.,-7.43465467928082,-13.32262679532));
#53199=CARTESIAN_POINT('Ctrl Pts',(-50.,-7.45658443707985,-13.4231254995838));
#53200=CARTESIAN_POINT('Ctrl Pts',(-50.,-7.47595026385202,-13.5247388655977));
#53201=CARTESIAN_POINT('Ctrl Pts',(-50.,-7.49330244824787,-13.6271680529626));
#53202=CARTESIAN_POINT('Ctrl Pts',(-50.,-7.50902360355704,-13.730201376709));
#53203=CARTESIAN_POINT('Ctrl Pts',(-50.,-7.52324912730704,-13.8337539100138));
#53204=CARTESIAN_POINT('Ctrl Pts',(-50.,-7.53595904837785,-13.9378208062029));
#53205=CARTESIAN_POINT('Ctrl Pts',(-50.,-7.54703967094767,-14.0424458557121));
#53206=CARTESIAN_POINT('Ctrl Pts',(-50.,-7.556353222684,-14.1476860346413));
#53207=CARTESIAN_POINT('Ctrl Pts',(-50.,-7.56381234400904,-14.2535736549186));
#53208=CARTESIAN_POINT('Ctrl Pts',(-50.,-7.56883349438523,-14.3488435570404));
#53209=CARTESIAN_POINT('Ctrl Pts',(-50.,-7.57166007128053,-14.4231630709543));
#53210=CARTESIAN_POINT('Ctrl Pts',(-50.,-7.57315469596912,-14.4762403397886));
#53211=CARTESIAN_POINT('Ctrl Pts',(-50.,-7.57386669307527,-14.5079003575064));
#53212=CARTESIAN_POINT('Ctrl Pts',(-50.,-7.57407686781798,-14.5180571909737));
#53213=CARTESIAN_POINT('',(-50.,-6.34597219029741,-15.0953390806557));
#53214=CARTESIAN_POINT('Origin',(-50.,0.,0.));
#53215=CARTESIAN_POINT('',(-50.,-5.00234392366024,-13.1426961282463));
#53216=CARTESIAN_POINT('Ctrl Pts',(-50.,-6.34597219029741,-15.0953390806557));
#53217=CARTESIAN_POINT('Ctrl Pts',(-50.,-6.34560329598179,-15.0950500814723));
#53218=CARTESIAN_POINT('Ctrl Pts',(-50.,-6.32458593740117,-15.0785714650465));
#53219=CARTESIAN_POINT('Ctrl Pts',(-50.,-6.28433170694406,-15.045518391722));
#53220=CARTESIAN_POINT('Ctrl Pts',(-50.,-6.22820881535241,-14.9949633327447));
#53221=CARTESIAN_POINT('Ctrl Pts',(-50.,-6.16012083060275,-14.925722782193));
#53222=CARTESIAN_POINT('Ctrl Pts',(-50.,-6.08025962758854,-14.8376145740015));
#53223=CARTESIAN_POINT('Ctrl Pts',(-50.,-5.99951493159239,-14.7487702776409));
#53224=CARTESIAN_POINT('Ctrl Pts',(-50.,-5.91563026424745,-14.6597125620614));
#53225=CARTESIAN_POINT('Ctrl Pts',(-50.,-5.8293396720056,-14.5703597544468));
#53226=CARTESIAN_POINT('Ctrl Pts',(-50.,-5.7429409442582,-14.4802820917477));
#53227=CARTESIAN_POINT('Ctrl Pts',(-50.,-5.65928349609497,-14.3888825985252));
#53228=CARTESIAN_POINT('Ctrl Pts',(-50.,-5.58037590052447,-14.2956379130225));
#53229=CARTESIAN_POINT('Ctrl Pts',(-50.,-5.50704098217782,-14.2001904323636));
#53230=CARTESIAN_POINT('Ctrl Pts',(-50.,-5.43936923240832,-14.102334498799));
#53231=CARTESIAN_POINT('Ctrl Pts',(-50.,-5.37693249048282,-14.0020293939727));
#53232=CARTESIAN_POINT('Ctrl Pts',(-50.,-5.31911705202313,-13.8994109809482));
#53233=CARTESIAN_POINT('Ctrl Pts',(-50.,-5.26532059680125,-13.7947771174053));
#53234=CARTESIAN_POINT('Ctrl Pts',(-50.,-5.21496886213029,-13.6885022424853));
#53235=CARTESIAN_POINT('Ctrl Pts',(-50.,-5.16756435218796,-13.5809703610753));
#53236=CARTESIAN_POINT('Ctrl Pts',(-50.,-5.12272617691501,-13.4724958081193));
#53237=CARTESIAN_POINT('Ctrl Pts',(-50.,-5.08022280379478,-13.3632644309532));
#53238=CARTESIAN_POINT('Ctrl Pts',(-50.,-5.04798920255339,-13.2753507597416));
#53239=CARTESIAN_POINT('Ctrl Pts',(-50.,-5.02478822352796,-13.2091330988228));
#53240=CARTESIAN_POINT('Ctrl Pts',(-50.,-5.00975329143057,-13.1648626726972));
#53241=CARTESIAN_POINT('Ctrl Pts',(-50.,-5.00234392366024,-13.1426961282463));
#53242=CARTESIAN_POINT('',(-50.,-3.67810171359515,-13.5729685048794));
#53243=CARTESIAN_POINT('Origin',(-50.,0.,0.));
#53244=CARTESIAN_POINT('',(-50.,-3.7256293105862,-15.9455420491152));
#53245=CARTESIAN_POINT('Ctrl Pts',(-50.,-3.67810171359514,-13.5729685048794));
#53246=CARTESIAN_POINT('Ctrl Pts',(-50.,-3.68389897142971,-13.5920397328724));
#53247=CARTESIAN_POINT('Ctrl Pts',(-50.,-3.69538324295473,-13.6302181028421));
#53248=CARTESIAN_POINT('Ctrl Pts',(-50.,-3.71227892449176,-13.6875933984758));
#53249=CARTESIAN_POINT('Ctrl Pts',(-50.,-3.73414411132176,-13.764309571506));
#53250=CARTESIAN_POINT('Ctrl Pts',(-50.,-3.76032689601146,-13.8605729560155));
#53251=CARTESIAN_POINT('Ctrl Pts',(-50.,-3.7852344832017,-13.9572274551481));
#53252=CARTESIAN_POINT('Ctrl Pts',(-50.,-3.8086220490069,-14.0543164841154));
#53253=CARTESIAN_POINT('Ctrl Pts',(-50.,-3.83008256273264,-14.1519113521203));
#53254=CARTESIAN_POINT('Ctrl Pts',(-50.,-3.84902164513744,-14.2501151271916));
#53255=CARTESIAN_POINT('Ctrl Pts',(-50.,-3.86478832158859,-14.3490371882169));
#53256=CARTESIAN_POINT('Ctrl Pts',(-50.,-3.87679564863944,-14.4487695813147));
#53257=CARTESIAN_POINT('Ctrl Pts',(-50.,-3.88463805371054,-14.5493641299902));
#53258=CARTESIAN_POINT('Ctrl Pts',(-50.,-3.88822932173376,-14.6508052317201));
#53259=CARTESIAN_POINT('Ctrl Pts',(-50.,-3.88787877668998,-14.7529954092481));
#53260=CARTESIAN_POINT('Ctrl Pts',(-50.,-3.88412655939816,-14.8557904709058));
#53261=CARTESIAN_POINT('Ctrl Pts',(-50.,-3.87761375658259,-14.9590275514473));
#53262=CARTESIAN_POINT('Ctrl Pts',(-50.,-3.86894768714904,-15.0625540503165));
#53263=CARTESIAN_POINT('Ctrl Pts',(-50.,-3.85855158779829,-15.1662600850723));
#53264=CARTESIAN_POINT('Ctrl Pts',(-50.,-3.84657772273756,-15.2700970690198));
#53265=CARTESIAN_POINT('Ctrl Pts',(-50.,-3.83300795359517,-15.3740553411364));
#53266=CARTESIAN_POINT('Ctrl Pts',(-50.,-3.81772126627406,-15.4781490410999));
#53267=CARTESIAN_POINT('Ctrl Pts',(-50.,-3.80057004743305,-15.5823990924153));
#53268=CARTESIAN_POINT('Ctrl Pts',(-50.,-3.78146164640637,-15.6868150664286));
#53269=CARTESIAN_POINT('Ctrl Pts',(-50.,-3.76263238690138,-15.7803405987066));
#53270=CARTESIAN_POINT('Ctrl Pts',(-50.,-3.74688765015641,-15.853028169516));
#53271=CARTESIAN_POINT('Ctrl Pts',(-50.,-3.73513553846456,-15.9048096163928));
#53272=CARTESIAN_POINT('Ctrl Pts',(-50.,-3.72795164063846,-15.9356520429153));
#53273=CARTESIAN_POINT('Ctrl Pts',(-50.,-3.7256293105862,-15.9455420491152));
#53274=CARTESIAN_POINT('',(-50.,-2.39254363182917,-16.1992703530064));
#53275=CARTESIAN_POINT('Origin',(-50.,0.,0.));
#53276=CARTESIAN_POINT('',(-50.,-1.57673047345591,-13.9738265075847));
#53277=CARTESIAN_POINT('Ctrl Pts',(-50.,-2.39254363182917,-16.1992703530064));
#53278=CARTESIAN_POINT('Ctrl Pts',(-50.,-2.39225819818113,-16.1988986929781));
#53279=CARTESIAN_POINT('Ctrl Pts',(-50.,-2.37599920382811,-16.1777109780555));
#53280=CARTESIAN_POINT('Ctrl Pts',(-50.,-2.34522959911868,-16.1356855077795));
#53281=CARTESIAN_POINT('Ctrl Pts',(-50.,-2.30344244328183,-16.0727615333669));
#53282=CARTESIAN_POINT('Ctrl Pts',(-50.,-2.25471299248206,-15.9887635087906));
#53283=CARTESIAN_POINT('Ctrl Pts',(-50.,-2.19927239636847,-15.8835627084126));
#53284=CARTESIAN_POINT('Ctrl Pts',(-50.,-2.14315912151332,-15.777429229659));
#53285=CARTESIAN_POINT('Ctrl Pts',(-50.,-2.08405759848474,-15.6703081575233));
#53286=CARTESIAN_POINT('Ctrl Pts',(-50.,-2.02269912351901,-15.5623029350202));
#53287=CARTESIAN_POINT('Ctrl Pts',(-50.,-1.96141617445265,-15.4535687378813));
#53288=CARTESIAN_POINT('Ctrl Pts',(-50.,-1.90311710851519,-15.3442359664661));
#53289=CARTESIAN_POINT('Ctrl Pts',(-50.,-1.84987755047685,-15.2342972131845));
#53290=CARTESIAN_POINT('Ctrl Pts',(-50.,-1.80258340663877,-15.1236107380773));
#53291=CARTESIAN_POINT('Ctrl Pts',(-50.,-1.76137347040452,-15.0119998487957));
#53292=CARTESIAN_POINT('Ctrl Pts',(-50.,-1.72584315874106,-14.8993186269813));
#53293=CARTESIAN_POINT('Ctrl Pts',(-50.,-1.69536426015181,-14.7855460452371));
#53294=CARTESIAN_POINT('Ctrl Pts',(-50.,-1.6692793032136,-14.6708208125467));
#53295=CARTESIAN_POINT('Ctrl Pts',(-50.,-1.64693894753001,-14.5553627910342));
#53296=CARTESIAN_POINT('Ctrl Pts',(-50.,-1.6277658288928,-14.4394201991873));
#53297=CARTESIAN_POINT('Ctrl Pts',(-50.,-1.61131285168258,-14.3232027730338));
#53298=CARTESIAN_POINT('Ctrl Pts',(-50.,-1.59730953904946,-14.2068329413785));
#53299=CARTESIAN_POINT('Ctrl Pts',(-50.,-1.58795185663835,-14.1136650691543));
#53300=CARTESIAN_POINT('Ctrl Pts',(-50.,-1.58194744165485,-14.0437579089631));
#53301=CARTESIAN_POINT('Ctrl Pts',(-50.,-1.57839446687451,-13.997139284115));
#53302=CARTESIAN_POINT('Ctrl Pts',(-50.,-1.57673047345591,-13.9738265075847));
#53303=CARTESIAN_POINT('',(-50.,-0.187087378736044,-14.0612554404903));
#53304=CARTESIAN_POINT('Origin',(-50.,0.,0.));
#53305=CARTESIAN_POINT('',(-50.,0.356913238135828,-16.3711098567093));
#53306=CARTESIAN_POINT('Ctrl Pts',(-50.,-0.187087378736032,-14.0612554404903));
#53307=CARTESIAN_POINT('Ctrl Pts',(-50.,-0.187959683517641,-14.0811692301831));
#53308=CARTESIAN_POINT('Ctrl Pts',(-50.,-0.189588581014708,-14.1210041786448));
#53309=CARTESIAN_POINT('Ctrl Pts',(-50.,-0.191684797850075,-14.1807787089954));
#53310=CARTESIAN_POINT('Ctrl Pts',(-50.,-0.193784513213942,-14.2605223532243));
#53311=CARTESIAN_POINT('Ctrl Pts',(-50.,-0.195204987344071,-14.3602728402636));
#53312=CARTESIAN_POINT('Ctrl Pts',(-50.,-0.195293060397626,-14.4600850256186));
#53313=CARTESIAN_POINT('Ctrl Pts',(-50.,-0.19380080315749,-14.5599400753078));
#53314=CARTESIAN_POINT('Ctrl Pts',(-50.,-0.190316238669402,-14.6598058338069));
#53315=CARTESIAN_POINT('Ctrl Pts',(-50.,-0.184238029232279,-14.7596343149665));
#53316=CARTESIAN_POINT('Ctrl Pts',(-50.,-0.174908450355344,-14.8593695705273));
#53317=CARTESIAN_POINT('Ctrl Pts',(-50.,-0.161736107560775,-14.9589547879103));
#53318=CARTESIAN_POINT('Ctrl Pts',(-50.,-0.144315282095873,-15.058339300691));
#53319=CARTESIAN_POINT('Ctrl Pts',(-50.,-0.122566347687195,-15.1574865557124));
#53320=CARTESIAN_POINT('Ctrl Pts',(-50.,-0.0968131519417803,-15.2563790638913));
#53321=CARTESIAN_POINT('Ctrl Pts',(-50.,-0.0676147251712506,-15.3550114911653));
#53322=CARTESIAN_POINT('Ctrl Pts',(-50.,-0.0356325161212601,-15.4533855207845));
#53323=CARTESIAN_POINT('Ctrl Pts',(-50.,-0.00149271387238248,-15.5515043804903));
#53324=CARTESIAN_POINT('Ctrl Pts',(-50.,0.0343674149818962,-15.6493668946876));
#53325=CARTESIAN_POINT('Ctrl Pts',(-50.,0.0717883068748032,-15.7469638696907));
#53326=CARTESIAN_POINT('Ctrl Pts',(-50.,0.110785127729046,-15.844281437166));
#53327=CARTESIAN_POINT('Ctrl Pts',(-50.,0.151478606156202,-15.9413031975852));
#53328=CARTESIAN_POINT('Ctrl Pts',(-50.,0.194016921417006,-16.0380127071578));
#53329=CARTESIAN_POINT('Ctrl Pts',(-50.,0.238492193683111,-16.1343961952447));
#53330=CARTESIAN_POINT('Ctrl Pts',(-50.,0.279988751445404,-16.220300804523));
#53331=CARTESIAN_POINT('Ctrl Pts',(-50.,0.313315502115871,-16.2867892048278));
#53332=CARTESIAN_POINT('Ctrl Pts',(-50.,0.337575921789304,-16.3340212110009));
#53333=CARTESIAN_POINT('Ctrl Pts',(-50.,0.352204323826718,-16.3621081032393));
#53334=CARTESIAN_POINT('Ctrl Pts',(-50.,0.356913238135828,-16.3711098567093));
#53335=CARTESIAN_POINT('',(-50.,1.71121724218688,-16.2853418923289));
#53336=CARTESIAN_POINT('Origin',(-50.,0.,0.));
#53337=CARTESIAN_POINT('',(-50.,1.94795475120472,-13.9269299753125));
#53338=CARTESIAN_POINT('Ctrl Pts',(-50.,1.71121724218688,-16.2853418923289));
#53339=CARTESIAN_POINT('Ctrl Pts',(-50.,1.71140128032148,-16.284910924222));
#53340=CARTESIAN_POINT('Ctrl Pts',(-50.,1.72188029803531,-16.2603454128541));
#53341=CARTESIAN_POINT('Ctrl Pts',(-50.,1.74123190957046,-16.211988160483));
#53342=CARTESIAN_POINT('Ctrl Pts',(-50.,1.76605768896888,-16.1406490153657));
#53343=CARTESIAN_POINT('Ctrl Pts',(-50.,1.79236675521062,-16.047171421572));
#53344=CARTESIAN_POINT('Ctrl Pts',(-50.,1.81990320787353,-15.9314881821968));
#53345=CARTESIAN_POINT('Ctrl Pts',(-50.,1.84785925815835,-15.8147342778518));
#53346=CARTESIAN_POINT('Ctrl Pts',(-50.,1.87846407081847,-15.6962806600859));
#53347=CARTESIAN_POINT('Ctrl Pts',(-50.,1.91103504986532,-15.5764093880396));
#53348=CARTESIAN_POINT('Ctrl Pts',(-50.,1.94335158717786,-15.4558508259636));
#53349=CARTESIAN_POINT('Ctrl Pts',(-50.,1.97262912616775,-15.3354545564815));
#53350=CARTESIAN_POINT('Ctrl Pts',(-50.,1.99685540944097,-15.2157295916163));
#53351=CARTESIAN_POINT('Ctrl Pts',(-50.,2.01513711377743,-15.096758960368));
#53352=CARTESIAN_POINT('Ctrl Pts',(-50.,2.02729586462329,-14.9784060380191));
#53353=CARTESIAN_POINT('Ctrl Pts',(-50.,2.03368724587156,-14.8604288747958));
#53354=CARTESIAN_POINT('Ctrl Pts',(-50.,2.03491450329845,-14.7426508740692));
#53355=CARTESIAN_POINT('Ctrl Pts',(-50.,2.03164894817481,-14.625042880531));
#53356=CARTESIAN_POINT('Ctrl Pts',(-50.,2.02457419816135,-14.5076563645426));
#53357=CARTESIAN_POINT('Ctrl Pts',(-50.,2.01431120793567,-14.3905881617116));
#53358=CARTESIAN_POINT('Ctrl Pts',(-50.,2.00134518601523,-14.2739302306637));
#53359=CARTESIAN_POINT('Ctrl Pts',(-50.,1.98596855852791,-14.1577338890203));
#53360=CARTESIAN_POINT('Ctrl Pts',(-50.,1.9718623445077,-14.0651658958429));
#53361=CARTESIAN_POINT('Ctrl Pts',(-50.,1.96029291597316,-13.9959617603545));
#53362=CARTESIAN_POINT('Ctrl Pts',(-50.,1.95214068696407,-13.9499241564345));
#53363=CARTESIAN_POINT('Ctrl Pts',(-50.,1.94795475120472,-13.9269299753125));
#53364=CARTESIAN_POINT('',(-50.,3.31568234418831,-13.6660219830951));
#53365=CARTESIAN_POINT('Origin',(-50.,0.,0.));
#53366=CARTESIAN_POINT('',(-50.,4.41702961547073,-15.7680206232759));
#53367=CARTESIAN_POINT('Ctrl Pts',(-50.,3.31568234418832,-13.6660219830951));
#53368=CARTESIAN_POINT('Ctrl Pts',(-50.,3.31978980257722,-13.6855270778435));
#53369=CARTESIAN_POINT('Ctrl Pts',(-50.,3.3281186287285,-13.7245156284827));
#53370=CARTESIAN_POINT('Ctrl Pts',(-50.,3.34095358960791,-13.7829335399729));
#53371=CARTESIAN_POINT('Ctrl Pts',(-50.,3.35875127854871,-13.860694068957));
#53372=CARTESIAN_POINT('Ctrl Pts',(-50.,3.38218236859189,-13.9576639685687));
#53373=CARTESIAN_POINT('Ctrl Pts',(-50.,3.40691934362888,-14.0543622734568));
#53374=CARTESIAN_POINT('Ctrl Pts',(-50.,3.43319765990381,-14.1507090838548));
#53375=CARTESIAN_POINT('Ctrl Pts',(-50.,3.46140835460361,-14.246570799961));
#53376=CARTESIAN_POINT('Ctrl Pts',(-50.,3.49212193962963,-14.3417513965941));
#53377=CARTESIAN_POINT('Ctrl Pts',(-50.,3.52596156208203,-14.436033113783));
#53378=CARTESIAN_POINT('Ctrl Pts',(-50.,3.56348590797974,-14.5292138499942));
#53379=CARTESIAN_POINT('Ctrl Pts',(-50.,3.60507534944737,-14.6211436324314));
#53380=CARTESIAN_POINT('Ctrl Pts',(-50.,3.65079792075207,-14.7117672540732));
#53381=CARTESIAN_POINT('Ctrl Pts',(-50.,3.7003355991968,-14.801148312913));
#53382=CARTESIAN_POINT('Ctrl Pts',(-50.,3.75314559090774,-14.8894206676529));
#53383=CARTESIAN_POINT('Ctrl Pts',(-50.,3.80858764637521,-14.9767504442745));
#53384=CARTESIAN_POINT('Ctrl Pts',(-50.,3.8660560521067,-15.0632964960055));
#53385=CARTESIAN_POINT('Ctrl Pts',(-50.,3.92512698668427,-15.1491664279643));
#53386=CARTESIAN_POINT('Ctrl Pts',(-50.,3.98564361314731,-15.2343910171469));
#53387=CARTESIAN_POINT('Ctrl Pts',(-50.,4.04761717203886,-15.3189530593075));
#53388=CARTESIAN_POINT('Ctrl Pts',(-50.,4.11116052066234,-15.4028066461541));
#53389=CARTESIAN_POINT('Ctrl Pts',(-50.,4.17641309355012,-15.4858989998248));
#53390=CARTESIAN_POINT('Ctrl Pts',(-50.,4.24346069213056,-15.5681938729551));
#53391=CARTESIAN_POINT('Ctrl Pts',(-50.,4.30501716681229,-15.6410798566978));
#53392=CARTESIAN_POINT('Ctrl Pts',(-50.,4.35383188909641,-15.6971913757796));
#53393=CARTESIAN_POINT('Ctrl Pts',(-50.,4.38907624535977,-15.736906180594));
#53394=CARTESIAN_POINT('Ctrl Pts',(-50.,4.41022999530898,-15.7604727358124));
#53395=CARTESIAN_POINT('Ctrl Pts',(-50.,4.41702961547073,-15.7680206232759));
#53396=CARTESIAN_POINT('',(-50.,5.70745604345954,-15.3481455072584));
#53397=CARTESIAN_POINT('Origin',(-50.,0.,0.));
#53398=CARTESIAN_POINT('',(-50.,5.35024281477071,-13.004953213026));
#53399=CARTESIAN_POINT('Ctrl Pts',(-50.,5.70745604345954,-15.3481455072584));
#53400=CARTESIAN_POINT('Ctrl Pts',(-50.,5.70752712228785,-15.3476823103842));
#53401=CARTESIAN_POINT('Ctrl Pts',(-50.,5.7115677281404,-15.3212825439959));
#53402=CARTESIAN_POINT('Ctrl Pts',(-50.,5.71828541357827,-15.2696319735416));
#53403=CARTESIAN_POINT('Ctrl Pts',(-50.,5.72458992151582,-15.1943601585744));
#53404=CARTESIAN_POINT('Ctrl Pts',(-50.,5.72682550780959,-15.0972765365679));
#53405=CARTESIAN_POINT('Ctrl Pts',(-50.,5.72472760042901,-14.9783796615786));
#53406=CARTESIAN_POINT('Ctrl Pts',(-50.,5.72276984468895,-14.8583414088431));
#53407=CARTESIAN_POINT('Ctrl Pts',(-50.,5.72295493404455,-14.7359981218931));
#53408=CARTESIAN_POINT('Ctrl Pts',(-50.,5.72469186277131,-14.611792753182));
#53409=CARTESIAN_POINT('Ctrl Pts',(-50.,5.72601142143879,-14.4869849640075));
#53410=CARTESIAN_POINT('Ctrl Pts',(-50.,5.7244278180311,-14.3630901368566));
#53411=CARTESIAN_POINT('Ctrl Pts',(-50.,5.71811860006313,-14.2411017202677));
#53412=CARTESIAN_POINT('Ctrl Pts',(-50.,5.7062391581791,-14.1213222951832));
#53413=CARTESIAN_POINT('Ctrl Pts',(-50.,5.68858274460417,-14.0036638891498));
#53414=CARTESIAN_POINT('Ctrl Pts',(-50.,5.66543360144756,-13.8878037235725));
#53415=CARTESIAN_POINT('Ctrl Pts',(-50.,5.63733210461441,-13.7734207288063));
#53416=CARTESIAN_POINT('Ctrl Pts',(-50.,5.60492122426722,-13.6603197171863));
#53417=CARTESIAN_POINT('Ctrl Pts',(-50.,5.56887590111916,-13.548380533239));
#53418=CARTESIAN_POINT('Ctrl Pts',(-50.,5.52982166345111,-13.4375425451545));
#53419=CARTESIAN_POINT('Ctrl Pts',(-50.,5.48825134524296,-13.3277741560577));
#53420=CARTESIAN_POINT('Ctrl Pts',(-50.,5.44446094769152,-13.2190523479119));
#53421=CARTESIAN_POINT('Ctrl Pts',(-50.,5.40777718254589,-13.1329006212338));
#53422=CARTESIAN_POINT('Ctrl Pts',(-50.,5.37936086023753,-13.0687478607962));
#53423=CARTESIAN_POINT('Ctrl Pts',(-50.,5.36001566196946,-13.026183989773));
#53424=CARTESIAN_POINT('Ctrl Pts',(-50.,5.35024281477071,-13.004953213026));
#53425=CARTESIAN_POINT('',(-50.,6.61011555120063,-12.4121021043889));
#53426=CARTESIAN_POINT('Origin',(-50.,0.,0.));
#53427=CARTESIAN_POINT('',(-50.,8.199607777367,-14.1741686633588));
#53428=CARTESIAN_POINT('Ctrl Pts',(-50.,6.61011555120064,-12.4121021043889));
#53429=CARTESIAN_POINT('Ctrl Pts',(-50.,6.6189446860433,-12.4299729273552));
#53430=CARTESIAN_POINT('Ctrl Pts',(-50.,6.63670790506457,-12.4656652861453));
#53431=CARTESIAN_POINT('Ctrl Pts',(-50.,6.66366757586302,-12.5190559665502));
#53432=CARTESIAN_POINT('Ctrl Pts',(-50.,6.70024437485702,-12.5899474002701));
#53433=CARTESIAN_POINT('Ctrl Pts',(-50.,6.74705476751256,-12.6780437370314));
#53434=CARTESIAN_POINT('Ctrl Pts',(-50.,6.79506247552229,-12.7655522513249));
#53435=CARTESIAN_POINT('Ctrl Pts',(-50.,6.84447568757558,-12.8523369979956));
#53436=CARTESIAN_POINT('Ctrl Pts',(-50.,6.89563993078743,-12.9381713275312));
#53437=CARTESIAN_POINT('Ctrl Pts',(-50.,6.94905904389849,-13.0227234927017));
#53438=CARTESIAN_POINT('Ctrl Pts',(-50.,7.00528244199424,-13.1056276044837));
#53439=CARTESIAN_POINT('Ctrl Pts',(-50.,7.06480099833745,-13.1865489711723));
#53440=CARTESIAN_POINT('Ctrl Pts',(-50.,7.12794583824513,-13.2652477369413));
#53441=CARTESIAN_POINT('Ctrl Pts',(-50.,7.19476912913493,-13.3416535097654));
#53442=CARTESIAN_POINT('Ctrl Pts',(-50.,7.26497865575545,-13.4159069786186));
#53443=CARTESIAN_POINT('Ctrl Pts',(-50.,7.33808196640605,-13.4882727841331));
#53444=CARTESIAN_POINT('Ctrl Pts',(-50.,7.41350024004436,-13.5590710567155));
#53445=CARTESIAN_POINT('Ctrl Pts',(-50.,7.49068629797234,-13.6286062937474));
#53446=CARTESIAN_POINT('Ctrl Pts',(-50.,7.56925639420599,-13.6970881198352));
#53447=CARTESIAN_POINT('Ctrl Pts',(-50.,7.6490662730339,-13.7645853488249));
#53448=CARTESIAN_POINT('Ctrl Pts',(-50.,7.7301225433348,-13.8310785215643));
#53449=CARTESIAN_POINT('Ctrl Pts',(-50.,7.81252309986449,-13.8964951055849));
#53450=CARTESIAN_POINT('Ctrl Pts',(-50.,7.89638987124254,-13.9607493051802));
#53451=CARTESIAN_POINT('Ctrl Pts',(-50.,7.98179694893469,-14.0237846738158));
#53452=CARTESIAN_POINT('Ctrl Pts',(-50.,8.05954552084273,-14.0790723376084));
#53453=CARTESIAN_POINT('Ctrl Pts',(-50.,8.1207810062114,-14.1212812823596));
#53454=CARTESIAN_POINT('Ctrl Pts',(-50.,8.16479476654098,-14.150983458568));
#53455=CARTESIAN_POINT('Ctrl Pts',(-50.,8.19114469649464,-14.1685489034304));
#53456=CARTESIAN_POINT('Ctrl Pts',(-50.,8.199607777367,-14.1741686633588));
#53457=CARTESIAN_POINT('',(-50.,9.34507439096662,-13.4465686934362));
#53458=CARTESIAN_POINT('Origin',(-50.,0.,0.));
#53459=CARTESIAN_POINT('',(-50.,8.41635544546801,-11.2658274114927));
#53460=CARTESIAN_POINT('Ctrl Pts',(-50.,9.34507439096662,-13.4465686934362));
#53461=CARTESIAN_POINT('Ctrl Pts',(-50.,9.34502804434446,-13.4461023721578));
#53462=CARTESIAN_POINT('Ctrl Pts',(-50.,9.3423763522097,-13.4195271451628));
#53463=CARTESIAN_POINT('Ctrl Pts',(-50.,9.33603801466832,-13.3678286519246));
#53464=CARTESIAN_POINT('Ctrl Pts',(-50.,9.32342511572492,-13.293353772072));
#53465=CARTESIAN_POINT('Ctrl Pts',(-50.,9.30144675196197,-13.1987642428721));
#53466=CARTESIAN_POINT('Ctrl Pts',(-50.,9.26984630377419,-13.0841244601964));
#53467=CARTESIAN_POINT('Ctrl Pts',(-50.,9.23809775500251,-12.9683443039596));
#53468=CARTESIAN_POINT('Ctrl Pts',(-50.,9.20785149120868,-12.8497986264917));
#53469=CARTESIAN_POINT('Ctrl Pts',(-50.,9.17864523199547,-12.7290634412273));
#53470=CARTESIAN_POINT('Ctrl Pts',(-50.,9.14888489929381,-12.6078485573591));
#53471=CARTESIAN_POINT('Ctrl Pts',(-50.,9.11653965711474,-12.4882399401825));
#53472=CARTESIAN_POINT('Ctrl Pts',(-50.,9.08009136927418,-12.3716530527263));
#53473=CARTESIAN_POINT('Ctrl Pts',(-50.,9.03879721019277,-12.2585910156016));
#53474=CARTESIAN_POINT('Ctrl Pts',(-50.,8.99243504959771,-12.149020036252));
#53475=CARTESIAN_POINT('Ctrl Pts',(-50.,8.94119992783734,-12.0425567886278));
#53476=CARTESIAN_POINT('Ctrl Pts',(-50.,8.88553539714026,-11.9387559040544));
#53477=CARTESIAN_POINT('Ctrl Pts',(-50.,8.8260156863806,-11.8372684268691));
#53478=CARTESIAN_POINT('Ctrl Pts',(-50.,8.76326465031677,-11.7378101255738));
#53479=CARTESIAN_POINT('Ctrl Pts',(-50.,8.69787308659046,-11.6401667106607));
#53480=CARTESIAN_POINT('Ctrl Pts',(-50.,8.63031048807256,-11.544185015102));
#53481=CARTESIAN_POINT('Ctrl Pts',(-50.,8.56085783218497,-11.4497691315105));
#53482=CARTESIAN_POINT('Ctrl Pts',(-50.,8.50390149179148,-11.3754469011628));
#53483=CARTESIAN_POINT('Ctrl Pts',(-50.,8.46042377774785,-11.3203764696515));
#53484=CARTESIAN_POINT('Ctrl Pts',(-50.,8.43110114017464,-11.2839607760805));
#53485=CARTESIAN_POINT('Ctrl Pts',(-50.,8.41635544546801,-11.2658274114927));
#53486=CARTESIAN_POINT('',(-50.,9.48921088782657,-10.3782842019456));
#53487=CARTESIAN_POINT('Origin',(-50.,0.,0.));
#53488=CARTESIAN_POINT('',(-50.,11.4669744265634,-11.689701557377));
#53489=CARTESIAN_POINT('Ctrl Pts',(-50.,9.48921088782658,-10.3782842019456));
#53490=CARTESIAN_POINT('Ctrl Pts',(-50.,9.50220693210954,-10.3933978635985));
#53491=CARTESIAN_POINT('Ctrl Pts',(-50.,9.52828841562115,-10.4235513483695));
#53492=CARTESIAN_POINT('Ctrl Pts',(-50.,9.56767882107163,-10.4685600648819));
#53493=CARTESIAN_POINT('Ctrl Pts',(-50.,9.62073647531797,-10.5281280338367));
#53494=CARTESIAN_POINT('Ctrl Pts',(-50.,9.68798490145875,-10.6018153909131));
#53495=CARTESIAN_POINT('Ctrl Pts',(-50.,9.75624684158698,-10.6746356328252));
#53496=CARTESIAN_POINT('Ctrl Pts',(-50.,9.82569013557624,-10.7464053109633));
#53497=CARTESIAN_POINT('Ctrl Pts',(-50.,9.89659308973021,-10.816818967327));
#53498=CARTESIAN_POINT('Ctrl Pts',(-50.,9.9693612115878,-10.885429977536));
#53499=CARTESIAN_POINT('Ctrl Pts',(-50.,10.0444356624493,-10.951747313668));
#53500=CARTESIAN_POINT('Ctrl Pts',(-50.,10.1222086594491,-11.0153247237569));
#53501=CARTESIAN_POINT('Ctrl Pts',(-50.,10.2029412752749,-11.0758475399707));
#53502=CARTESIAN_POINT('Ctrl Pts',(-50.,10.2866665326243,-11.1332346082697));
#53503=CARTESIAN_POINT('Ctrl Pts',(-50.,10.3731363846505,-11.1876948686032));
#53504=CARTESIAN_POINT('Ctrl Pts',(-50.,10.4619396643774,-11.2396071151889));
#53505=CARTESIAN_POINT('Ctrl Pts',(-50.,10.5525953486849,-11.289425367888));
#53506=CARTESIAN_POINT('Ctrl Pts',(-50.,10.6446491749193,-11.3375806355454));
#53507=CARTESIAN_POINT('Ctrl Pts',(-50.,10.737781584702,-11.3843713907704));
#53508=CARTESIAN_POINT('Ctrl Pts',(-50.,10.8318699676878,-11.4299001604323));
#53509=CARTESIAN_POINT('Ctrl Pts',(-50.,10.926915885831,-11.4741464531626));
#53510=CARTESIAN_POINT('Ctrl Pts',(-50.,11.0229961202521,-11.5170156697979));
#53511=CARTESIAN_POINT('Ctrl Pts',(-50.,11.1202074324343,-11.5583943876468));
#53512=CARTESIAN_POINT('Ctrl Pts',(-50.,11.2186075484415,-11.5982095077484));
#53513=CARTESIAN_POINT('Ctrl Pts',(-50.,11.3076629888636,-11.632424924341));
#53514=CARTESIAN_POINT('Ctrl Pts',(-50.,11.3774715865628,-11.6580791515292));
#53515=CARTESIAN_POINT('Ctrl Pts',(-50.,11.4274892045258,-11.6759024021635));
#53516=CARTESIAN_POINT('Ctrl Pts',(-50.,11.4573796514766,-11.6863630351679));
#53517=CARTESIAN_POINT('Ctrl Pts',(-50.,11.4669744265634,-11.689701557377));
#53518=CARTESIAN_POINT('',(-50.,12.3955073457098,-10.7000945155851));
#53519=CARTESIAN_POINT('Origin',(-50.,0.,0.));
#53520=CARTESIAN_POINT('',(-50.,10.9536375103364,-8.81882824088046));
#53521=CARTESIAN_POINT('Ctrl Pts',(-50.,12.3955073457098,-10.7000945155851));
#53522=CARTESIAN_POINT('Ctrl Pts',(-50.,12.3953464857659,-10.6996543705834));
#53523=CARTESIAN_POINT('Ctrl Pts',(-50.,12.3861691112129,-10.6745735022306));
#53524=CARTESIAN_POINT('Ctrl Pts',(-50.,12.3671730117507,-10.6260754926723));
#53525=CARTESIAN_POINT('Ctrl Pts',(-50.,12.336435220754,-10.5570770785351));
#53526=CARTESIAN_POINT('Ctrl Pts',(-50.,12.2916238883603,-10.4709250501372));
#53527=CARTESIAN_POINT('Ctrl Pts',(-50.,12.2325064717433,-10.3677455989363));
#53528=CARTESIAN_POINT('Ctrl Pts',(-50.,12.1729620080223,-10.2634984322242));
#53529=CARTESIAN_POINT('Ctrl Pts',(-50.,12.1141848750712,-10.1561990251342));
#53530=CARTESIAN_POINT('Ctrl Pts',(-50.,12.0558705645975,-10.0465202590396));
#53531=CARTESIAN_POINT('Ctrl Pts',(-50.,11.9969002916812,-9.93651465742827));
#53532=CARTESIAN_POINT('Ctrl Pts',(-50.,11.9358257812543,-9.82870769953299));
#53533=CARTESIAN_POINT('Ctrl Pts',(-50.,11.8715286035136,-9.724847924125));
#53534=CARTESIAN_POINT('Ctrl Pts',(-50.,11.8034143911192,-9.62560737856555));
#53535=CARTESIAN_POINT('Ctrl Pts',(-50.,11.7312595885623,-9.53100857350628));
#53536=CARTESIAN_POINT('Ctrl Pts',(-50.,11.655157779328,-9.44063172122792));
#53537=CARTESIAN_POINT('Ctrl Pts',(-50.,11.5754278219505,-9.35393513817802));
#53538=CARTESIAN_POINT('Ctrl Pts',(-50.,11.4925391231036,-9.27043802686381));
#53539=CARTESIAN_POINT('Ctrl Pts',(-50.,11.407025252502,-9.18970993907287));
#53540=CARTESIAN_POINT('Ctrl Pts',(-50.,11.3194051551598,-9.11139639219764));
#53541=CARTESIAN_POINT('Ctrl Pts',(-50.,11.2300954828748,-9.03523227310488));
#53542=CARTESIAN_POINT('Ctrl Pts',(-50.,11.1393445344495,-8.96105481127105));
#53543=CARTESIAN_POINT('Ctrl Pts',(-50.,11.0656943951459,-8.90323201632451));
#53544=CARTESIAN_POINT('Ctrl Pts',(-50.,11.0098871540402,-8.86070419148627));
#53545=CARTESIAN_POINT('Ctrl Pts',(-50.,10.9724295263217,-8.83272480732197));
#53546=CARTESIAN_POINT('Ctrl Pts',(-50.,10.9536375103364,-8.81882824088046));
#53547=CARTESIAN_POINT('',(-50.,11.7720642054939,-7.6923605344347));
#53548=CARTESIAN_POINT('Origin',(-50.,0.,0.));
#53549=CARTESIAN_POINT('',(-50.,14.0138288999568,-8.47072751083015));
#53550=CARTESIAN_POINT('Ctrl Pts',(-50.,11.7720642054939,-7.69236053443469));
#53551=CARTESIAN_POINT('Ctrl Pts',(-50.,11.7884105699588,-7.70376738782835));
#53552=CARTESIAN_POINT('Ctrl Pts',(-50.,11.8211715224307,-7.72648734423527));
#53553=CARTESIAN_POINT('Ctrl Pts',(-50.,11.870517618491,-7.7602860336664));
#53554=CARTESIAN_POINT('Ctrl Pts',(-50.,11.936722320441,-7.80478766329085));
#53555=CARTESIAN_POINT('Ctrl Pts',(-50.,12.0201833141302,-7.85943599303422));
#53556=CARTESIAN_POINT('Ctrl Pts',(-50.,12.1044103376288,-7.91299239895144));
#53557=CARTESIAN_POINT('Ctrl Pts',(-50.,12.1895203359981,-7.96523745572904));
#53558=CARTESIAN_POINT('Ctrl Pts',(-50.,12.2757069077219,-8.01580608992824));
#53559=CARTESIAN_POINT('Ctrl Pts',(-50.,12.3632517496072,-8.06416486307078));
#53560=CARTESIAN_POINT('Ctrl Pts',(-50.,12.4524600493824,-8.10972846142537));
#53561=CARTESIAN_POINT('Ctrl Pts',(-50.,12.5436007236081,-8.15196711241727));
#53562=CARTESIAN_POINT('Ctrl Pts',(-50.,12.636848388186,-8.19051110794578));
#53563=CARTESIAN_POINT('Ctrl Pts',(-50.,12.7322148461558,-8.22527363116368));
#53564=CARTESIAN_POINT('Ctrl Pts',(-50.,12.829511804771,-8.25651874452987));
#53565=CARTESIAN_POINT('Ctrl Pts',(-50.,12.9284352169133,-8.284715594814));
#53566=CARTESIAN_POINT('Ctrl Pts',(-50.,13.0286320818366,-8.31042356359388));
#53567=CARTESIAN_POINT('Ctrl Pts',(-50.,13.1297695959248,-8.33417308930716));
#53568=CARTESIAN_POINT('Ctrl Pts',(-50.,13.231612467433,-8.35633273843435));
#53569=CARTESIAN_POINT('Ctrl Pts',(-50.,13.3340674354409,-8.37703230872753));
#53570=CARTESIAN_POINT('Ctrl Pts',(-50.,13.4371309168349,-8.39625156414993));
#53571=CARTESIAN_POINT('Ctrl Pts',(-50.,13.5408537546603,-8.41387978285669));
#53572=CARTESIAN_POINT('Ctrl Pts',(-50.,13.6453014633841,-8.42978304193647));
#53573=CARTESIAN_POINT('Ctrl Pts',(-50.,13.7505117765273,-8.44387618307839));
#53574=CARTESIAN_POINT('Ctrl Pts',(-50.,13.8452784046188,-8.45486947201102));
#53575=CARTESIAN_POINT('Ctrl Pts',(-50.,13.9192737837169,-8.4623570321923));
#53576=CARTESIAN_POINT('Ctrl Pts',(-50.,13.9721524684248,-8.46718145686578));
#53577=CARTESIAN_POINT('Ctrl Pts',(-50.,14.0037053056615,-8.4698799979691));
#53578=CARTESIAN_POINT('Ctrl Pts',(-50.,14.0138288999568,-8.47072751083015));
#53579=CARTESIAN_POINT('',(-50.,14.6670849864349,-7.28129404712485));
#53580=CARTESIAN_POINT('Origin',(-50.,0.,0.));
#53581=CARTESIAN_POINT('',(-50.,12.8026622457696,-5.81770965851216));
#53582=CARTESIAN_POINT('Ctrl Pts',(-50.,14.6670849864349,-7.28129404712485));
#53583=CARTESIAN_POINT('Ctrl Pts',(-50.,14.6668197205911,-7.28090773432903));
#53584=CARTESIAN_POINT('Ctrl Pts',(-50.,14.6516933118151,-7.2588971478181));
#53585=CARTESIAN_POINT('Ctrl Pts',(-50.,14.6212330452241,-7.21664693024351));
#53586=CARTESIAN_POINT('Ctrl Pts',(-50.,14.5743017306281,-7.15746040594034));
#53587=CARTESIAN_POINT('Ctrl Pts',(-50.,14.5094730904225,-7.08515912713373));
#53588=CARTESIAN_POINT('Ctrl Pts',(-50.,14.426553270081,-6.99992315179396));
#53589=CARTESIAN_POINT('Ctrl Pts',(-50.,14.3429542890555,-6.9137592074853));
#53590=CARTESIAN_POINT('Ctrl Pts',(-50.,14.2593394703776,-6.8244480871404));
#53591=CARTESIAN_POINT('Ctrl Pts',(-50.,14.1755812112355,-6.73271726045961));
#53592=CARTESIAN_POINT('Ctrl Pts',(-50.,14.0911063172293,-6.64083299762664));
#53593=CARTESIAN_POINT('Ctrl Pts',(-50.,14.0051400746611,-6.55160160666348));
#53594=CARTESIAN_POINT('Ctrl Pts',(-50.,13.9170340351662,-6.46699483496205));
#53595=CARTESIAN_POINT('Ctrl Pts',(-50.,13.8263796359301,-6.38781142942664));
#53596=CARTESIAN_POINT('Ctrl Pts',(-50.,13.7329659430228,-6.31412878948963));
#53597=CARTESIAN_POINT('Ctrl Pts',(-50.,13.6367792028716,-6.24551704256852));
#53598=CARTESIAN_POINT('Ctrl Pts',(-50.,13.537993545262,-6.18137222620287));
#53599=CARTESIAN_POINT('Ctrl Pts',(-50.,13.4369440601197,-6.12111191134452));
#53600=CARTESIAN_POINT('Ctrl Pts',(-50.,13.3340405059683,-6.06418647971103));
#53601=CARTESIAN_POINT('Ctrl Pts',(-50.,13.2296973679703,-6.01012352904084));
#53602=CARTESIAN_POINT('Ctrl Pts',(-50.,13.124252277086,-5.95856265812867));
#53603=CARTESIAN_POINT('Ctrl Pts',(-50.,13.0179052519711,-5.90928446078516));
#53604=CARTESIAN_POINT('Ctrl Pts',(-50.,12.932189022876,-5.87159432010365));
#53605=CARTESIAN_POINT('Ctrl Pts',(-50.,12.8675588289116,-5.84428128157946));
#53606=CARTESIAN_POINT('Ctrl Pts',(-50.,12.8243198115569,-5.82649625442995));
#53607=CARTESIAN_POINT('Ctrl Pts',(-50.,12.8026622457696,-5.81770965851216));
#53608=CARTESIAN_POINT('',(-50.,13.3152354345065,-4.52309756402218));
#53609=CARTESIAN_POINT('Origin',(-50.,0.,0.));
#53610=CARTESIAN_POINT('',(-50.,15.6801429643085,-4.71950650162129));
#53611=CARTESIAN_POINT('Ctrl Pts',(-50.,13.3152354345065,-4.52309756402217));
#53612=CARTESIAN_POINT('Ctrl Pts',(-50.,13.3339050169562,-4.53008087460641));
#53613=CARTESIAN_POINT('Ctrl Pts',(-50.,13.3712869472582,-4.54393972423008));
#53614=CARTESIAN_POINT('Ctrl Pts',(-50.,13.4274881372306,-4.56440469062003));
#53615=CARTESIAN_POINT('Ctrl Pts',(-50.,13.5026800019769,-4.59104377985933));
#53616=CARTESIAN_POINT('Ctrl Pts',(-50.,13.5971094020329,-4.62321932672933));
#53617=CARTESIAN_POINT('Ctrl Pts',(-50.,13.6920092152502,-4.65414675070122));
#53618=CARTESIAN_POINT('Ctrl Pts',(-50.,13.7874381437893,-4.68358443705714));
#53619=CARTESIAN_POINT('Ctrl Pts',(-50.,13.8834929138094,-4.71113063582666));
#53620=CARTESIAN_POINT('Ctrl Pts',(-50.,13.9803137113395,-4.73619861233502));
#53621=CARTESIAN_POINT('Ctrl Pts',(-50.,14.0780505744683,-4.75814554445644));
#53622=CARTESIAN_POINT('Ctrl Pts',(-50.,14.1768322221664,-4.77639142656668));
#53623=CARTESIAN_POINT('Ctrl Pts',(-50.,14.27673584179,-4.79053474041595));
#53624=CARTESIAN_POINT('Ctrl Pts',(-50.,14.3777512750926,-4.80048846137132));
#53625=CARTESIAN_POINT('Ctrl Pts',(-50.,14.4797618145538,-4.80655518238588));
#53626=CARTESIAN_POINT('Ctrl Pts',(-50.,14.5825896373118,-4.80926492456431));
#53627=CARTESIAN_POINT('Ctrl Pts',(-50.,14.6860319453295,-4.80924728319928));
#53628=CARTESIAN_POINT('Ctrl Pts',(-50.,14.7898983053036,-4.80709879692323));
#53629=CARTESIAN_POINT('Ctrl Pts',(-50.,14.8940524763685,-4.80323496770043));
#53630=CARTESIAN_POINT('Ctrl Pts',(-50.,14.9984364069554,-4.79780470849564));
#53631=CARTESIAN_POINT('Ctrl Pts',(-50.,15.1030415940234,-4.79078931010852));
#53632=CARTESIAN_POINT('Ctrl Pts',(-50.,15.2078897478867,-4.78206888507335));
#53633=CARTESIAN_POINT('Ctrl Pts',(-50.,15.3130110194811,-4.77149742512795));
#53634=CARTESIAN_POINT('Ctrl Pts',(-50.,15.418420778849,-4.75898306342126));
#53635=CARTESIAN_POINT('Ctrl Pts',(-50.,15.5129440588396,-4.74606347591976));
#53636=CARTESIAN_POINT('Ctrl Pts',(-50.,15.586476817532,-4.73491389815065));
#53637=CARTESIAN_POINT('Ctrl Pts',(-50.,15.6388940067504,-4.72643636051809));
#53638=CARTESIAN_POINT('Ctrl Pts',(-50.,15.6701266534662,-4.72120325045824));
#53639=CARTESIAN_POINT('Ctrl Pts',(-50.,15.6801429643085,-4.71950650162129));
#53640=CARTESIAN_POINT('',(-50.,16.017075735697,-3.40498309495743));
#53641=CARTESIAN_POINT('Origin',(-50.,0.,0.));
#53642=CARTESIAN_POINT('',(-50.,13.847248627403,-2.45104298226008));
#53643=CARTESIAN_POINT('Ctrl Pts',(-50.,16.017075735697,-3.40498309495743));
#53644=CARTESIAN_POINT('Ctrl Pts',(-50.,16.0167227315819,-3.40467488782123));
#53645=CARTESIAN_POINT('Ctrl Pts',(-50.,15.9965977364772,-3.38711758925191));
#53646=CARTESIAN_POINT('Ctrl Pts',(-50.,15.9565872333324,-3.35376990021665));
#53647=CARTESIAN_POINT('Ctrl Pts',(-50.,15.8964112622344,-3.30811417274226));
#53648=CARTESIAN_POINT('Ctrl Pts',(-50.,15.8156387361042,-3.25420659877988));
#53649=CARTESIAN_POINT('Ctrl Pts',(-50.,15.7141266693079,-3.19226978910788));
#53650=CARTESIAN_POINT('Ctrl Pts',(-50.,15.6117260024113,-3.1296030647124));
#53651=CARTESIAN_POINT('Ctrl Pts',(-50.,15.5085273245779,-3.06389197726713));
#53652=CARTESIAN_POINT('Ctrl Pts',(-50.,15.4045879562307,-2.99587287520288));
#53653=CARTESIAN_POINT('Ctrl Pts',(-50.,15.299916309402,-2.9278833773088));
#53654=CARTESIAN_POINT('Ctrl Pts',(-50.,15.1944599098748,-2.86283428974206));
#53655=CARTESIAN_POINT('Ctrl Pts',(-50.,15.0880810351184,-2.80279667637514));
#53656=CARTESIAN_POINT('Ctrl Pts',(-50.,14.9805825983482,-2.74864579544975));
#53657=CARTESIAN_POINT('Ctrl Pts',(-50.,14.8717795409674,-2.70050907188802));
#53658=CARTESIAN_POINT('Ctrl Pts',(-50.,14.7615516365331,-2.65797355871958));
#53659=CARTESIAN_POINT('Ctrl Pts',(-50.,14.6499173448672,-2.62041096375855));
#53660=CARTESIAN_POINT('Ctrl Pts',(-50.,14.537056384215,-2.58717382256056));
#53661=CARTESIAN_POINT('Ctrl Pts',(-50.,14.423228955274,-2.55762788131115));
#53662=CARTESIAN_POINT('Ctrl Pts',(-50.,14.3087190397278,-2.53121250086624));
#53663=CARTESIAN_POINT('Ctrl Pts',(-50.,14.1937640331043,-2.50749463728168));
#53664=CARTESIAN_POINT('Ctrl Pts',(-50.,14.0785031060049,-2.48621203480011));
#53665=CARTESIAN_POINT('Ctrl Pts',(-50.,13.9861066530346,-2.47102275853729));
#53666=CARTESIAN_POINT('Ctrl Pts',(-50.,13.9167144589915,-2.46064068498796));
#53667=CARTESIAN_POINT('Ctrl Pts',(-50.,13.8704109184829,-2.45416751351779));
#53668=CARTESIAN_POINT('Ctrl Pts',(-50.,13.847248627403,-2.45104298226008));
#53669=CARTESIAN_POINT('Origin',(-50.,0.,0.));
#53670=CARTESIAN_POINT('Origin',(-50.,0.,0.));
#53671=CARTESIAN_POINT('',(-50.,5.93712762672243,-8.04677050399782));
#53672=CARTESIAN_POINT('Origin',(-50.,0.,0.));
#53673=CARTESIAN_POINT('',(-50.,3.75038736519794,-6.13145585166881));
#53674=CARTESIAN_POINT('Ctrl Pts',(-50.,3.75038736519793,-6.13145585166881));
#53675=CARTESIAN_POINT('Ctrl Pts',(-50.,3.7614973065729,-6.1481985134482));
#53676=CARTESIAN_POINT('Ctrl Pts',(-50.,3.78357651403939,-6.1817683663582));
#53677=CARTESIAN_POINT('Ctrl Pts',(-50.,3.81627329006595,-6.23237673886416));
#53678=CARTESIAN_POINT('Ctrl Pts',(-50.,3.859023878729,-6.30036238594766));
#53679=CARTESIAN_POINT('Ctrl Pts',(-50.,3.91110213900011,-6.38616193008433));
#53680=CARTESIAN_POINT('Ctrl Pts',(-50.,3.96197913233089,-6.47268455970493));
#53681=CARTESIAN_POINT('Ctrl Pts',(-50.,4.01197889710939,-6.55973735411151));
#53682=CARTESIAN_POINT('Ctrl Pts',(-50.,4.06165666819706,-6.64698999124062));
#53683=CARTESIAN_POINT('Ctrl Pts',(-50.,4.11183783259628,-6.73395053478792));
#53684=CARTESIAN_POINT('Ctrl Pts',(-50.,4.16348379256721,-6.82003644526658));
#53685=CARTESIAN_POINT('Ctrl Pts',(-50.,4.21757413484032,-6.90463617300865));
#53686=CARTESIAN_POINT('Ctrl Pts',(-50.,4.27498923356982,-6.98717136730191));
#53687=CARTESIAN_POINT('Ctrl Pts',(-50.,4.33637651734857,-7.06716577496009));
#53688=CARTESIAN_POINT('Ctrl Pts',(-50.,4.40207217433237,-7.14429034032177));
#53689=CARTESIAN_POINT('Ctrl Pts',(-50.,4.47217290162416,-7.21834255288981));
#53690=CARTESIAN_POINT('Ctrl Pts',(-50.,4.54657777868016,-7.28923990788708));
#53691=CARTESIAN_POINT('Ctrl Pts',(-50.,4.62503998887083,-7.35700721943171));
#53692=CARTESIAN_POINT('Ctrl Pts',(-50.,4.70721371156899,-7.42177134000892));
#53693=CARTESIAN_POINT('Ctrl Pts',(-50.,4.79269894740031,-7.48374039375355));
#53694=CARTESIAN_POINT('Ctrl Pts',(-50.,4.88107836846757,-7.54316218647348));
#53695=CARTESIAN_POINT('Ctrl Pts',(-50.,4.9719575030537,-7.60028648840776));
#53696=CARTESIAN_POINT('Ctrl Pts',(-50.,5.06499955030093,-7.65532943098672));
#53697=CARTESIAN_POINT('Ctrl Pts',(-50.,5.15997145275563,-7.70842918324715));
#53698=CARTESIAN_POINT('Ctrl Pts',(-50.,5.25675269887972,-7.75963419345371));
#53699=CARTESIAN_POINT('Ctrl Pts',(-50.,5.35529468870783,-7.80893560674388));
#53700=CARTESIAN_POINT('Ctrl Pts',(-50.,5.45559153104423,-7.85628931405591));
#53701=CARTESIAN_POINT('Ctrl Pts',(-50.,5.5576484178972,-7.90164067817667));
#53702=CARTESIAN_POINT('Ctrl Pts',(-50.,5.66144582368073,-7.94495188520329));
#53703=CARTESIAN_POINT('Ctrl Pts',(-50.,5.75805784341865,-7.98274785508065));
#53704=CARTESIAN_POINT('Ctrl Pts',(-50.,5.83459703193086,-8.01098733792827));
#53705=CARTESIAN_POINT('Ctrl Pts',(-50.,5.89025885371265,-8.03066876757453));
#53706=CARTESIAN_POINT('Ctrl Pts',(-50.,5.92452703906404,-8.04247213408069));
#53707=CARTESIAN_POINT('Ctrl Pts',(-50.,5.93712762672279,-8.04677050399795));
#53708=CARTESIAN_POINT('',(-50.,2.45543694297674,-6.75507110762463));
#53709=CARTESIAN_POINT('Origin',(-50.,0.,0.));
#53710=CARTESIAN_POINT('',(-50.,2.55037217513312,-9.66931237308562));
#53711=CARTESIAN_POINT('Ctrl Pts',(-50.,2.55037217513312,-9.66931237308562));
#53712=CARTESIAN_POINT('Ctrl Pts',(-50.,2.55611128043686,-9.64665974290731));
#53713=CARTESIAN_POINT('Ctrl Pts',(-50.,2.57093577554682,-9.59816055611738));
#53714=CARTESIAN_POINT('Ctrl Pts',(-50.,2.60118245057803,-9.51956163099604));
#53715=CARTESIAN_POINT('Ctrl Pts',(-50.,2.6506378639391,-9.4077851093183));
#53716=CARTESIAN_POINT('Ctrl Pts',(-50.,2.71205611361093,-9.26593773005304));
#53717=CARTESIAN_POINT('Ctrl Pts',(-50.,2.76185693608665,-9.12774569066013));
#53718=CARTESIAN_POINT('Ctrl Pts',(-50.,2.79564609540172,-8.99695638729624));
#53719=CARTESIAN_POINT('Ctrl Pts',(-50.,2.81593951016314,-8.87218721998315));
#53720=CARTESIAN_POINT('Ctrl Pts',(-50.,2.8281804649272,-8.7503085875302));
#53721=CARTESIAN_POINT('Ctrl Pts',(-50.,2.838231660712,-8.62789111098118));
#53722=CARTESIAN_POINT('Ctrl Pts',(-50.,2.84893087833482,-8.50318672326558));
#53723=CARTESIAN_POINT('Ctrl Pts',(-50.,2.85932311928695,-8.37659160589212));
#53724=CARTESIAN_POINT('Ctrl Pts',(-50.,2.8666442371861,-8.24955186700095));
#53725=CARTESIAN_POINT('Ctrl Pts',(-50.,2.86748815125169,-8.12392974416385));
#53726=CARTESIAN_POINT('Ctrl Pts',(-50.,2.85947913898695,-8.00108902987832));
#53727=CARTESIAN_POINT('Ctrl Pts',(-50.,2.84216119689693,-7.88140953422486));
#53728=CARTESIAN_POINT('Ctrl Pts',(-50.,2.81629364412744,-7.76466852264525));
#53729=CARTESIAN_POINT('Ctrl Pts',(-50.,2.78345892001629,-7.65025207826714));
#53730=CARTESIAN_POINT('Ctrl Pts',(-50.,2.74553095355499,-7.53744508591865));
#53731=CARTESIAN_POINT('Ctrl Pts',(-50.,2.70427297026251,-7.42564364342468));
#53732=CARTESIAN_POINT('Ctrl Pts',(-50.,2.66128382072048,-7.31434056822034));
#53733=CARTESIAN_POINT('Ctrl Pts',(-50.,2.61790620462629,-7.20313763732345));
#53734=CARTESIAN_POINT('Ctrl Pts',(-50.,2.57514309471485,-7.09174914908801));
#53735=CARTESIAN_POINT('Ctrl Pts',(-50.,2.53358368474749,-6.98000697278327));
#53736=CARTESIAN_POINT('Ctrl Pts',(-50.,2.50153193679118,-6.89026394714059));
#53737=CARTESIAN_POINT('Ctrl Pts',(-50.,2.47820711493347,-6.82274841734025));
#53738=CARTESIAN_POINT('Ctrl Pts',(-50.,2.46297417772978,-6.77764561818537));
#53739=CARTESIAN_POINT('Ctrl Pts',(-50.,2.45543694297674,-6.75507110762463));
#53740=CARTESIAN_POINT('',(-50.,1.85780428234483,-9.82591284555798));
#53741=CARTESIAN_POINT('Origin',(-50.,0.,0.));
#53742=CARTESIAN_POINT('',(-50.,0.718643267461627,-7.15148293042304));
#53743=CARTESIAN_POINT('Ctrl Pts',(-50.,0.718643267461621,-7.15148293042304));
#53744=CARTESIAN_POINT('Ctrl Pts',(-50.,0.721388610069064,-7.17138797035723));
#53745=CARTESIAN_POINT('Ctrl Pts',(-50.,0.72671587532212,-7.21121317182152));
#53746=CARTESIAN_POINT('Ctrl Pts',(-50.,0.734216502709278,-7.2709963393441));
#53747=CARTESIAN_POINT('Ctrl Pts',(-50.,0.743235585416283,-7.35079807608913));
#53748=CARTESIAN_POINT('Ctrl Pts',(-50.,0.752929449590465,-7.45069670452966));
#53749=CARTESIAN_POINT('Ctrl Pts',(-50.,0.761227274615911,-7.55072560028829));
#53750=CARTESIAN_POINT('Ctrl Pts',(-50.,0.768504714146026,-7.65085154280962));
#53751=CARTESIAN_POINT('Ctrl Pts',(-50.,0.775405338877349,-7.75101782957587));
#53752=CARTESIAN_POINT('Ctrl Pts',(-50.,0.782886239966143,-7.85113936329068));
#53753=CARTESIAN_POINT('Ctrl Pts',(-50.,0.792066365329068,-7.95110843081948));
#53754=CARTESIAN_POINT('Ctrl Pts',(-50.,0.804093633570272,-8.05079907170372));
#53755=CARTESIAN_POINT('Ctrl Pts',(-50.,0.820012171364339,-8.15007218998677));
#53756=CARTESIAN_POINT('Ctrl Pts',(-50.,0.840611930230857,-8.24877960511329));
#53757=CARTESIAN_POINT('Ctrl Pts',(-50.,0.866338577132719,-8.34677071475058));
#53758=CARTESIAN_POINT('Ctrl Pts',(-50.,0.897367099160984,-8.4439050185459));
#53759=CARTESIAN_POINT('Ctrl Pts',(-50.,0.933642367528787,-8.5400643944807));
#53760=CARTESIAN_POINT('Ctrl Pts',(-50.,0.974931241694465,-8.63516410958082));
#53761=CARTESIAN_POINT('Ctrl Pts',(-50.,1.02086710880845,-8.72916840803945));
#53762=CARTESIAN_POINT('Ctrl Pts',(-50.,1.07099928020948,-8.82209124999857));
#53763=CARTESIAN_POINT('Ctrl Pts',(-50.,1.12484423754393,-8.91397482898789));
#53764=CARTESIAN_POINT('Ctrl Pts',(-50.,1.18193820283021,-9.00487302535333));
#53765=CARTESIAN_POINT('Ctrl Pts',(-50.,1.24188395306769,-9.09483443436949));
#53766=CARTESIAN_POINT('Ctrl Pts',(-50.,1.30441156144786,-9.18388242219763));
#53767=CARTESIAN_POINT('Ctrl Pts',(-50.,1.3693914299125,-9.27200835121914));
#53768=CARTESIAN_POINT('Ctrl Pts',(-50.,1.43678361338666,-9.35918315674388));
#53769=CARTESIAN_POINT('Ctrl Pts',(-50.,1.50660194229105,-9.44536454178638));
#53770=CARTESIAN_POINT('Ctrl Pts',(-50.,1.57887480066182,-9.53050553264656));
#53771=CARTESIAN_POINT('Ctrl Pts',(-50.,1.65360100339141,-9.61456358834088));
#53772=CARTESIAN_POINT('Ctrl Pts',(-50.,1.72424636870643,-9.69053496490009));
#53773=CARTESIAN_POINT('Ctrl Pts',(-50.,1.78095314232172,-9.7491869690921));
#53774=CARTESIAN_POINT('Ctrl Pts',(-50.,1.82256325859169,-9.79107008383992));
#53775=CARTESIAN_POINT('Ctrl Pts',(-50.,1.84831653795888,-9.81657295799139));
#53776=CARTESIAN_POINT('Ctrl Pts',(-50.,1.85780428234483,-9.82591284555798));
#53777=CARTESIAN_POINT('',(-50.,-0.718643267461624,-7.15148293042304));
#53778=CARTESIAN_POINT('Origin',(-50.,0.,0.));
#53779=CARTESIAN_POINT('',(-50.,-1.89755147577054,-9.81831443766195));
#53780=CARTESIAN_POINT('Ctrl Pts',(-50.,-1.89755147577054,-9.81831443766195));
#53781=CARTESIAN_POINT('Ctrl Pts',(-50.,-1.88255211267964,-9.80039522756355));
#53782=CARTESIAN_POINT('Ctrl Pts',(-50.,-1.84815269559462,-9.76313107751608));
#53783=CARTESIAN_POINT('Ctrl Pts',(-50.,-1.78679858751167,-9.70543943338958));
#53784=CARTESIAN_POINT('Ctrl Pts',(-50.,-1.69374278455301,-9.62619016686422));
#53785=CARTESIAN_POINT('Ctrl Pts',(-50.,-1.576861582378,-9.52503847397034));
#53786=CARTESIAN_POINT('Ctrl Pts',(-50.,-1.47203331296336,-9.42213951575228));
#53787=CARTESIAN_POINT('Ctrl Pts',(-50.,-1.38484298036779,-9.31896299195203));
#53788=CARTESIAN_POINT('Ctrl Pts',(-50.,-1.31242393260393,-9.21535483920498));
#53789=CARTESIAN_POINT('Ctrl Pts',(-50.,-1.24851405668088,-9.11085713692575));
#53790=CARTESIAN_POINT('Ctrl Pts',(-50.,-1.18634328973517,-9.00492385207762));
#53791=CARTESIAN_POINT('Ctrl Pts',(-50.,-1.12259642171968,-8.89721129760285));
#53792=CARTESIAN_POINT('Ctrl Pts',(-50.,-1.05830577327405,-8.78766206238304));
#53793=CARTESIAN_POINT('Ctrl Pts',(-50.,-0.996589197042053,-8.67637972666424));
#53794=CARTESIAN_POINT('Ctrl Pts',(-50.,-0.941323460369318,-8.56356426545847));
#53795=CARTESIAN_POINT('Ctrl Pts',(-50.,-0.895240742652424,-8.44941362598824));
#53796=CARTESIAN_POINT('Ctrl Pts',(-50.,-0.858916682261846,-8.33407215281038));
#53797=CARTESIAN_POINT('Ctrl Pts',(-50.,-0.831570515383447,-8.21766862525226));
#53798=CARTESIAN_POINT('Ctrl Pts',(-50.,-0.811510144890449,-8.10033651802127));
#53799=CARTESIAN_POINT('Ctrl Pts',(-50.,-0.796736942256156,-7.98224460192821));
#53800=CARTESIAN_POINT('Ctrl Pts',(-50.,-0.785400272847099,-7.86361381479518));
#53801=CARTESIAN_POINT('Ctrl Pts',(-50.,-0.775839563797133,-7.74468091618948));
#53802=CARTESIAN_POINT('Ctrl Pts',(-50.,-0.766672302003446,-7.62566969516693));
#53803=CARTESIAN_POINT('Ctrl Pts',(-50.,-0.756870878958097,-7.5067579169994));
#53804=CARTESIAN_POINT('Ctrl Pts',(-50.,-0.745831500234844,-7.38804974272502));
#53805=CARTESIAN_POINT('Ctrl Pts',(-50.,-0.735771087779772,-7.29328733826105));
#53806=CARTESIAN_POINT('Ctrl Pts',(-50.,-0.72749213560466,-7.22233768688913));
#53807=CARTESIAN_POINT('Ctrl Pts',(-50.,-0.721647166649912,-7.17509214524366));
#53808=CARTESIAN_POINT('Ctrl Pts',(-50.,-0.718643267461624,-7.15148293042304));
#53809=CARTESIAN_POINT('',(-50.,-2.58947998462545,-9.65891264114259));
#53810=CARTESIAN_POINT('Origin',(-50.,0.,0.));
#53811=CARTESIAN_POINT('',(-50.,-2.45543694297674,-6.75507110762463));
#53812=CARTESIAN_POINT('Ctrl Pts',(-50.,-2.45543694297675,-6.75507110762463));
#53813=CARTESIAN_POINT('Ctrl Pts',(-50.,-2.46159994790965,-6.77419608843536));
#53814=CARTESIAN_POINT('Ctrl Pts',(-50.,-2.47407975508802,-6.8123887688799));
#53815=CARTESIAN_POINT('Ctrl Pts',(-50.,-2.49326086758344,-6.8695059418988));
#53816=CARTESIAN_POINT('Ctrl Pts',(-50.,-2.5197596307744,-6.94531805563895));
#53817=CARTESIAN_POINT('Ctrl Pts',(-50.,-2.55437015138428,-7.03952961984441));
#53818=CARTESIAN_POINT('Ctrl Pts',(-50.,-2.59029498067661,-7.13325283216217));
#53819=CARTESIAN_POINT('Ctrl Pts',(-50.,-2.62718125254576,-7.22662075191781));
#53820=CARTESIAN_POINT('Ctrl Pts',(-50.,-2.66442452752942,-7.31986152676826));
#53821=CARTESIAN_POINT('Ctrl Pts',(-50.,-2.70112557395893,-7.41331375298832));
#53822=CARTESIAN_POINT('Ctrl Pts',(-50.,-2.73622951961898,-7.50736587770304));
#53823=CARTESIAN_POINT('Ctrl Pts',(-50.,-2.76864747338962,-7.60240247767684));
#53824=CARTESIAN_POINT('Ctrl Pts',(-50.,-2.79737835816915,-7.69875126136884));
#53825=CARTESIAN_POINT('Ctrl Pts',(-50.,-2.82164615909785,-7.79662146983088));
#53826=CARTESIAN_POINT('Ctrl Pts',(-50.,-2.84098400021346,-7.89607078269802));
#53827=CARTESIAN_POINT('Ctrl Pts',(-50.,-2.85517326277626,-7.9970485375799));
#53828=CARTESIAN_POINT('Ctrl Pts',(-50.,-2.86421236488387,-8.099424390731));
#53829=CARTESIAN_POINT('Ctrl Pts',(-50.,-2.8682745946465,-8.20302084448955));
#53830=CARTESIAN_POINT('Ctrl Pts',(-50.,-2.86767474496505,-8.30764661663281));
#53831=CARTESIAN_POINT('Ctrl Pts',(-50.,-2.86282492937103,-8.41311873833255));
#53832=CARTESIAN_POINT('Ctrl Pts',(-50.,-2.85417908993455,-8.51926543389428));
#53833=CARTESIAN_POINT('Ctrl Pts',(-50.,-2.84217845398458,-8.62593402210748));
#53834=CARTESIAN_POINT('Ctrl Pts',(-50.,-2.82720199177778,-8.73299593720093));
#53835=CARTESIAN_POINT('Ctrl Pts',(-50.,-2.80950303716262,-8.84035511450549));
#53836=CARTESIAN_POINT('Ctrl Pts',(-50.,-2.78919460623265,-8.94794754130566));
#53837=CARTESIAN_POINT('Ctrl Pts',(-50.,-2.76630007756038,-9.05572969970196));
#53838=CARTESIAN_POINT('Ctrl Pts',(-50.,-2.74078863839312,-9.16366948222194));
#53839=CARTESIAN_POINT('Ctrl Pts',(-50.,-2.71261433447333,-9.27173688239595));
#53840=CARTESIAN_POINT('Ctrl Pts',(-50.,-2.68175977570501,-9.37989305792331));
#53841=CARTESIAN_POINT('Ctrl Pts',(-50.,-2.65107324582197,-9.47899277830914));
#53842=CARTESIAN_POINT('Ctrl Pts',(-50.,-2.62543035908095,-9.55644055509579));
#53843=CARTESIAN_POINT('Ctrl Pts',(-50.,-2.60611334216455,-9.61222989040676));
#53844=CARTESIAN_POINT('Ctrl Pts',(-50.,-2.59397572160338,-9.64638111520572));
#53845=CARTESIAN_POINT('Ctrl Pts',(-50.,-2.58947998462532,-9.65891264114296));
#53846=CARTESIAN_POINT('',(-50.,-3.75038736519793,-6.13145585166881));
#53847=CARTESIAN_POINT('Origin',(-50.,0.,0.));
#53848=CARTESIAN_POINT('',(-50.,-5.96964178495622,-8.0226789141349));
#53849=CARTESIAN_POINT('Ctrl Pts',(-50.,-5.96964178495622,-8.0226789141349));
#53850=CARTESIAN_POINT('Ctrl Pts',(-50.,-5.94835297189343,-8.0130422434411));
#53851=CARTESIAN_POINT('Ctrl Pts',(-50.,-5.9011918592682,-7.9943937520678));
#53852=CARTESIAN_POINT('Ctrl Pts',(-50.,-5.8208822516981,-7.96903592659697));
#53853=CARTESIAN_POINT('Ctrl Pts',(-50.,-5.70265690217233,-7.93801020438781));
#53854=CARTESIAN_POINT('Ctrl Pts',(-50.,-5.55346250303877,-7.89758853118704));
#53855=CARTESIAN_POINT('Ctrl Pts',(-50.,-5.41436931107715,-7.85036305479183));
#53856=CARTESIAN_POINT('Ctrl Pts',(-50.,-5.29104691989087,-7.79523468647088));
#53857=CARTESIAN_POINT('Ctrl Pts',(-50.,-5.18084571969554,-7.73330841361203));
#53858=CARTESIAN_POINT('Ctrl Pts',(-50.,-5.07792505734327,-7.66688869302314));
#53859=CARTESIAN_POINT('Ctrl Pts',(-50.,-4.97594840210465,-7.59842098612654));
#53860=CARTESIAN_POINT('Ctrl Pts',(-50.,-4.87177973271099,-7.52903405731413));
#53861=CARTESIAN_POINT('Ctrl Pts',(-50.,-4.76632422816958,-7.45822827381644));
#53862=CARTESIAN_POINT('Ctrl Pts',(-50.,-4.66243591843162,-7.38474417264741));
#53863=CARTESIAN_POINT('Ctrl Pts',(-50.,-4.56369441608956,-7.30707985875561));
#53864=CARTESIAN_POINT('Ctrl Pts',(-50.,-4.4726472158023,-7.22422822821349));
#53865=CARTESIAN_POINT('Ctrl Pts',(-50.,-4.38987557857684,-7.13606957084443));
#53866=CARTESIAN_POINT('Ctrl Pts',(-50.,-4.31473193577955,-7.04305867353628));
#53867=CARTESIAN_POINT('Ctrl Pts',(-50.,-4.24574967308285,-6.94604996627335));
#53868=CARTESIAN_POINT('Ctrl Pts',(-50.,-4.18120131531612,-6.84606267872027));
#53869=CARTESIAN_POINT('Ctrl Pts',(-50.,-4.11951535961712,-6.74409882925098));
#53870=CARTESIAN_POINT('Ctrl Pts',(-50.,-4.0592984076569,-6.64109222642907));
#53871=CARTESIAN_POINT('Ctrl Pts',(-50.,-3.99940195660266,-6.53784434718121));
#53872=CARTESIAN_POINT('Ctrl Pts',(-50.,-3.93897729264122,-6.43496121510494));
#53873=CARTESIAN_POINT('Ctrl Pts',(-50.,-3.87752560957259,-6.33279865263617));
#53874=CARTESIAN_POINT('Ctrl Pts',(-50.,-3.82734562477572,-6.25178572573963));
#53875=CARTESIAN_POINT('Ctrl Pts',(-50.,-3.78910264658076,-6.19145440139071));
#53876=CARTESIAN_POINT('Ctrl Pts',(-50.,-3.7633374392529,-6.15142367620606));
#53877=CARTESIAN_POINT('Ctrl Pts',(-50.,-3.75038736519793,-6.13145585166881));
#53878=CARTESIAN_POINT('',(-50.,-6.52388598275276,-7.57884632935924));
#53879=CARTESIAN_POINT('Origin',(-50.,0.,0.));
#53880=CARTESIAN_POINT('',(-50.,-5.14318775290069,-5.02073460645077));
#53881=CARTESIAN_POINT('Ctrl Pts',(-50.,-5.14318775290069,-5.02073460645076));
#53882=CARTESIAN_POINT('Ctrl Pts',(-50.,-5.15703844666268,-5.03529159113598));
#53883=CARTESIAN_POINT('Ctrl Pts',(-50.,-5.18485354740602,-5.06428722179623));
#53884=CARTESIAN_POINT('Ctrl Pts',(-50.,-5.22691734521339,-5.10742564369891));
#53885=CARTESIAN_POINT('Ctrl Pts',(-50.,-5.28368554926634,-5.16423261553338));
#53886=CARTESIAN_POINT('Ctrl Pts',(-50.,-5.35574541658332,-5.23409735978387));
#53887=CARTESIAN_POINT('Ctrl Pts',(-50.,-5.42877754716296,-5.30295185702147));
#53888=CARTESIAN_POINT('Ctrl Pts',(-50.,-5.50252175190725,-5.37106909242141));
#53889=CARTESIAN_POINT('Ctrl Pts',(-50.,-5.57653243923659,-5.43891687637388));
#53890=CARTESIAN_POINT('Ctrl Pts',(-50.,-5.65014634083023,-5.50719043557996));
#53891=CARTESIAN_POINT('Ctrl Pts',(-50.,-5.72258159055366,-5.57669744070723));
#53892=CARTESIAN_POINT('Ctrl Pts',(-50.,-5.79302399301176,-5.64825683559838));
#53893=CARTESIAN_POINT('Ctrl Pts',(-50.,-5.86071379627312,-5.72259822644884));
#53894=CARTESIAN_POINT('Ctrl Pts',(-50.,-5.92504262139805,-5.80024683316115));
#53895=CARTESIAN_POINT('Ctrl Pts',(-50.,-5.98561485393513,-5.88145719317904));
#53896=CARTESIAN_POINT('Ctrl Pts',(-50.,-6.04221154361855,-5.96627851638222));
#53897=CARTESIAN_POINT('Ctrl Pts',(-50.,-6.09477471117184,-6.05459405347559));
#53898=CARTESIAN_POINT('Ctrl Pts',(-50.,-6.14338347043832,-6.14616869769857));
#53899=CARTESIAN_POINT('Ctrl Pts',(-50.,-6.18823844577549,-6.2406935262026));
#53900=CARTESIAN_POINT('Ctrl Pts',(-50.,-6.22963155144596,-6.33782488040964));
#53901=CARTESIAN_POINT('Ctrl Pts',(-50.,-6.2678972444421,-6.43721103768399));
#53902=CARTESIAN_POINT('Ctrl Pts',(-50.,-6.30336681095649,-6.53852299564495));
#53903=CARTESIAN_POINT('Ctrl Pts',(-50.,-6.33632590879467,-6.64148049150319));
#53904=CARTESIAN_POINT('Ctrl Pts',(-50.,-6.36696110296949,-6.74588705654512));
#53905=CARTESIAN_POINT('Ctrl Pts',(-50.,-6.39534644338642,-6.85163598146165));
#53906=CARTESIAN_POINT('Ctrl Pts',(-50.,-6.42148411170256,-6.9586779143977));
#53907=CARTESIAN_POINT('Ctrl Pts',(-50.,-6.44533241567678,-7.06699729667253));
#53908=CARTESIAN_POINT('Ctrl Pts',(-50.,-6.46683693263443,-7.17658703219621));
#53909=CARTESIAN_POINT('Ctrl Pts',(-50.,-6.48596514159778,-7.28741967054497));
#53910=CARTESIAN_POINT('Ctrl Pts',(-50.,-6.5013152907357,-7.39001981975656));
#53911=CARTESIAN_POINT('Ctrl Pts',(-50.,-6.51181517907742,-7.47092388711047));
#53912=CARTESIAN_POINT('Ctrl Pts',(-50.,-6.5186172336226,-7.52956968091483));
#53913=CARTESIAN_POINT('Ctrl Pts',(-50.,-6.52249927647778,-7.56560518745242));
#53914=CARTESIAN_POINT('Ctrl Pts',(-50.,-6.52388598275276,-7.57884632935924));
#53915=CARTESIAN_POINT('',(-50.,-6.03932124977421,-3.89701874412038));
#53916=CARTESIAN_POINT('Origin',(-50.,0.,0.));
#53917=CARTESIAN_POINT('',(-50.,-8.85937132577942,-4.63805343996351));
#53918=CARTESIAN_POINT('Ctrl Pts',(-50.,-8.85937132577942,-4.63805343996351));
#53919=CARTESIAN_POINT('Ctrl Pts',(-50.,-8.83600957326199,-4.63860796949123));
#53920=CARTESIAN_POINT('Ctrl Pts',(-50.,-8.78542760184506,-4.64226869921731));
#53921=CARTESIAN_POINT('Ctrl Pts',(-50.,-8.70206879749976,-4.65426712072998));
#53922=CARTESIAN_POINT('Ctrl Pts',(-50.,-8.58208988181923,-4.67760996762605));
#53923=CARTESIAN_POINT('Ctrl Pts',(-50.,-8.43013206622476,-4.7059243222351));
#53924=CARTESIAN_POINT('Ctrl Pts',(-50.,-8.2843230642502,-4.72372591244526));
#53925=CARTESIAN_POINT('Ctrl Pts',(-50.,-8.14929412649754,-4.72756454905465));
#53926=CARTESIAN_POINT('Ctrl Pts',(-50.,-8.02313747309844,-4.71958541389958));
#53927=CARTESIAN_POINT('Ctrl Pts',(-50.,-7.9015907237349,-4.70439891524807));
#53928=CARTESIAN_POINT('Ctrl Pts',(-50.,-7.78000590743498,-4.68695765535521));
#53929=CARTESIAN_POINT('Ctrl Pts',(-50.,-7.65604731918147,-4.66963928443128));
#53930=CARTESIAN_POINT('Ctrl Pts',(-50.,-7.53031371454558,-4.65160090645338));
#53931=CARTESIAN_POINT('Ctrl Pts',(-50.,-7.40483002515176,-4.63046946729401));
#53932=CARTESIAN_POINT('Ctrl Pts',(-50.,-7.28216972266428,-4.60333867057275));
#53933=CARTESIAN_POINT('Ctrl Pts',(-50.,-7.16419105444418,-4.56819583049617));
#53934=CARTESIAN_POINT('Ctrl Pts',(-50.,-7.05136577826386,-4.52468089222283));
#53935=CARTESIAN_POINT('Ctrl Pts',(-50.,-6.94330777957998,-4.47348457408032));
#53936=CARTESIAN_POINT('Ctrl Pts',(-50.,-6.83906640781858,-4.4160130309926));
#53937=CARTESIAN_POINT('Ctrl Pts',(-50.,-6.73752748880879,-4.35393408054299));
#53938=CARTESIAN_POINT('Ctrl Pts',(-50.,-6.63770990687462,-4.2888323596294));
#53939=CARTESIAN_POINT('Ctrl Pts',(-50.,-6.53876341785232,-4.22215377357323));
#53940=CARTESIAN_POINT('Ctrl Pts',(-50.,-6.44000100425059,-4.15511874483724));
#53941=CARTESIAN_POINT('Ctrl Pts',(-50.,-6.34092094513049,-4.08864152493875));
#53942=CARTESIAN_POINT('Ctrl Pts',(-50.,-6.24122821720367,-4.02325912271413));
#53943=CARTESIAN_POINT('Ctrl Pts',(-50.,-6.16086742147115,-3.97204127711522));
#53944=CARTESIAN_POINT('Ctrl Pts',(-50.,-6.10023490810719,-3.93427763849175));
#53945=CARTESIAN_POINT('Ctrl Pts',(-50.,-6.05965257770704,-3.90939030583537));
#53946=CARTESIAN_POINT('Ctrl Pts',(-50.,-6.03932124977421,-3.89701874412038));
#53947=CARTESIAN_POINT('',(-50.,-9.16615635178499,-3.9976965535958));
#53948=CARTESIAN_POINT('Origin',(-50.,0.,0.));
#53949=CARTESIAN_POINT('',(-50.,-6.8122671513043,-2.29198004120026));
#53950=CARTESIAN_POINT('Ctrl Pts',(-50.,-6.8122671513043,-2.29198004120026));
#53951=CARTESIAN_POINT('Ctrl Pts',(-50.,-6.8310622341282,-2.29908584041335));
#53952=CARTESIAN_POINT('Ctrl Pts',(-50.,-6.86870350660446,-2.31314148102898));
#53953=CARTESIAN_POINT('Ctrl Pts',(-50.,-6.92531873868941,-2.33375705829959));
#53954=CARTESIAN_POINT('Ctrl Pts',(-50.,-7.00111274457534,-2.36030757076476));
#53955=CARTESIAN_POINT('Ctrl Pts',(-50.,-7.09634961812101,-2.39198792562662));
#53956=CARTESIAN_POINT('Ctrl Pts',(-50.,-7.19202414084635,-2.42233623016115));
#53957=CARTESIAN_POINT('Ctrl Pts',(-50.,-7.28802033430286,-2.45171132733138));
#53958=CARTESIAN_POINT('Ctrl Pts',(-50.,-7.3841397096708,-2.4807280346756));
#53959=CARTESIAN_POINT('Ctrl Pts',(-50.,-7.4800863304027,-2.5103005111467));
#53960=CARTESIAN_POINT('Ctrl Pts',(-50.,-7.57550619462173,-2.54149568187359));
#53961=CARTESIAN_POINT('Ctrl Pts',(-50.,-7.67002106404108,-2.5754046559055));
#53962=CARTESIAN_POINT('Ctrl Pts',(-50.,-7.76326299008741,-2.61301442971916));
#53963=CARTESIAN_POINT('Ctrl Pts',(-50.,-7.85491172665132,-2.65506217582471));
#53964=CARTESIAN_POINT('Ctrl Pts',(-50.,-7.94472127708621,-2.70194887521209));
#53965=CARTESIAN_POINT('Ctrl Pts',(-50.,-8.03251572538561,-2.75381386341092));
#53966=CARTESIAN_POINT('Ctrl Pts',(-50.,-8.11819217840571,-2.81057710920625));
#53967=CARTESIAN_POINT('Ctrl Pts',(-50.,-8.201719906256,-2.87199246251599));
#53968=CARTESIAN_POINT('Ctrl Pts',(-50.,-8.28314562863609,-2.93769454582461));
#53969=CARTESIAN_POINT('Ctrl Pts',(-50.,-8.36258324333989,-3.00724707660037));
#53970=CARTESIAN_POINT('Ctrl Pts',(-50.,-8.44018147897284,-3.08018804824792));
#53971=CARTESIAN_POINT('Ctrl Pts',(-50.,-8.51609606529771,-3.15607730017284));
#53972=CARTESIAN_POINT('Ctrl Pts',(-50.,-8.59046276963722,-3.23453838205034));
#53973=CARTESIAN_POINT('Ctrl Pts',(-50.,-8.66336443667969,-3.31531333416059));
#53974=CARTESIAN_POINT('Ctrl Pts',(-50.,-8.7348214836506,-3.3982738856883));
#53975=CARTESIAN_POINT('Ctrl Pts',(-50.,-8.80481446318767,-3.48337462556297));
#53976=CARTESIAN_POINT('Ctrl Pts',(-50.,-8.87329906122102,-3.57061962548306));
#53977=CARTESIAN_POINT('Ctrl Pts',(-50.,-8.94022316573707,-3.66002610520606));
#53978=CARTESIAN_POINT('Ctrl Pts',(-50.,-9.0055455660548,-3.75158344307814));
#53979=CARTESIAN_POINT('Ctrl Pts',(-50.,-9.06389210891971,-3.83736280325601));
#53980=CARTESIAN_POINT('Ctrl Pts',(-50.,-9.10845514068543,-3.90569911841461));
#53981=CARTESIAN_POINT('Ctrl Pts',(-50.,-9.14002903636781,-3.95558585200608));
#53982=CARTESIAN_POINT('Ctrl Pts',(-50.,-9.15916185644175,-3.9863683662662));
#53983=CARTESIAN_POINT('Ctrl Pts',(-50.,-9.16615635178519,-3.99769655359614));
#53984=CARTESIAN_POINT('',(-50.,-7.13209349341826,-0.89072928050049));
#53985=CARTESIAN_POINT('Origin',(-50.,0.,0.));
#53986=CARTESIAN_POINT('',(-50.,-9.99439372247306,-0.334804600014791));
#53987=CARTESIAN_POINT('Ctrl Pts',(-50.,-9.99439372247306,-0.334804600014791));
#53988=CARTESIAN_POINT('Ctrl Pts',(-50.,-9.97358611210015,-0.345440498390201));
#53989=CARTESIAN_POINT('Ctrl Pts',(-50.,-9.92960166167783,-0.370685396797522));
#53990=CARTESIAN_POINT('Ctrl Pts',(-50.,-9.85970389408656,-0.417663630762108));
#53991=CARTESIAN_POINT('Ctrl Pts',(-50.,-9.76173470794663,-0.490751709654423));
#53992=CARTESIAN_POINT('Ctrl Pts',(-50.,-9.63711058491003,-0.582194086890198));
#53993=CARTESIAN_POINT('Ctrl Pts',(-50.,-9.51346503399365,-0.66149692044243));
#53994=CARTESIAN_POINT('Ctrl Pts',(-50.,-9.39347368681776,-0.723542272923874));
#53995=CARTESIAN_POINT('Ctrl Pts',(-50.,-9.27634845263042,-0.771090641047726));
#53996=CARTESIAN_POINT('Ctrl Pts',(-50.,-9.1602494406401,-0.810145236641717));
#53997=CARTESIAN_POINT('Ctrl Pts',(-50.,-9.04313782728701,-0.847184879177381));
#53998=CARTESIAN_POINT('Ctrl Pts',(-50.,-8.92394083882956,-0.885365181899303));
#53999=CARTESIAN_POINT('Ctrl Pts',(-50.,-8.80283221651881,-0.923666931425906));
#54000=CARTESIAN_POINT('Ctrl Pts',(-50.,-8.68060673111004,-0.959073494961789));
#54001=CARTESIAN_POINT('Ctrl Pts',(-50.,-8.55832200571467,-0.98784980243911));
#54002=CARTESIAN_POINT('Ctrl Pts',(-50.,-8.43677899171613,-1.00737622330388));
#54003=CARTESIAN_POINT('Ctrl Pts',(-50.,-8.31624650623966,-1.017123671327));
#54004=CARTESIAN_POINT('Ctrl Pts',(-50.,-8.19667636355292,-1.01788199103989));
#54005=CARTESIAN_POINT('Ctrl Pts',(-50.,-8.0778221648407,-1.01133055607812));
#54006=CARTESIAN_POINT('Ctrl Pts',(-50.,-7.95940371279084,-0.999455440216892));
#54007=CARTESIAN_POINT('Ctrl Pts',(-50.,-7.84122460090589,-0.984110042106142));
#54008=CARTESIAN_POINT('Ctrl Pts',(-50.,-7.72314614047142,-0.966965984543332));
#54009=CARTESIAN_POINT('Ctrl Pts',(-50.,-7.60507887157754,-0.949420915891056));
#54010=CARTESIAN_POINT('Ctrl Pts',(-50.,-7.4869674381447,-0.932516236860826));
#54011=CARTESIAN_POINT('Ctrl Pts',(-50.,-7.36877903277666,-0.916863781503486));
#54012=CARTESIAN_POINT('Ctrl Pts',(-50.,-7.27415386726379,-0.90558533966873));
#54013=CARTESIAN_POINT('Ctrl Pts',(-50.,-7.20314083161155,-0.89786893854071));
#54014=CARTESIAN_POINT('Ctrl Pts',(-50.,-7.15577920638447,-0.893054239868308));
#54015=CARTESIAN_POINT('Ctrl Pts',(-50.,-7.13209349341826,-0.89072928050049));
#54016=CARTESIAN_POINT('',(-50.,-9.99295703981581,0.375246053138014));
#54017=CARTESIAN_POINT('Origin',(-50.,0.,0.));
#54018=CARTESIAN_POINT('',(-50.,-7.13209349341826,0.890729280500487));
#54019=CARTESIAN_POINT('Ctrl Pts',(-50.,-7.13209349341826,0.890729280500492));
#54020=CARTESIAN_POINT('Ctrl Pts',(-50.,-7.15211036864424,0.892482057440589));
#54021=CARTESIAN_POINT('Ctrl Pts',(-50.,-7.19212249719958,0.89615029887462));
#54022=CARTESIAN_POINT('Ctrl Pts',(-50.,-7.25207582250743,0.902140734147994));
#54023=CARTESIAN_POINT('Ctrl Pts',(-50.,-7.33188369780814,0.911105335666499));
#54024=CARTESIAN_POINT('Ctrl Pts',(-50.,-7.43143474677318,0.923884053007731));
#54025=CARTESIAN_POINT('Ctrl Pts',(-50.,-7.53080214904746,0.938052795086852));
#54026=CARTESIAN_POINT('Ctrl Pts',(-50.,-7.63003710778607,0.953237934402831));
#54027=CARTESIAN_POINT('Ctrl Pts',(-50.,-7.7292275500742,0.968799418422935));
#54028=CARTESIAN_POINT('Ctrl Pts',(-50.,-7.82850348500033,0.983785216334555));
#54029=CARTESIAN_POINT('Ctrl Pts',(-50.,-7.92800888935854,0.997080466154163));
#54030=CARTESIAN_POINT('Ctrl Pts',(-50.,-8.02787639670185,1.00753800115478));
#54031=CARTESIAN_POINT('Ctrl Pts',(-50.,-8.12820273854249,1.01410892133532));
#54032=CARTESIAN_POINT('Ctrl Pts',(-50.,-8.2290192302709,1.01599010763451));
#54033=CARTESIAN_POINT('Ctrl Pts',(-50.,-8.33027821569813,1.01271355471894));
#54034=CARTESIAN_POINT('Ctrl Pts',(-50.,-8.43188165539955,1.00407739851957));
#54035=CARTESIAN_POINT('Ctrl Pts',(-50.,-8.53370212161309,0.990109101007577));
#54036=CARTESIAN_POINT('Ctrl Pts',(-50.,-8.63560512714608,0.971017102543951));
#54037=CARTESIAN_POINT('Ctrl Pts',(-50.,-8.73747423363077,0.947150867813171));
#54038=CARTESIAN_POINT('Ctrl Pts',(-50.,-8.83922276353739,0.918952892194649));
#54039=CARTESIAN_POINT('Ctrl Pts',(-50.,-8.94078425956014,0.886903960171005));
#54040=CARTESIAN_POINT('Ctrl Pts',(-50.,-9.04210805084257,0.851468211346448));
#54041=CARTESIAN_POINT('Ctrl Pts',(-50.,-9.14315312384119,0.813043722977555));
#54042=CARTESIAN_POINT('Ctrl Pts',(-50.,-9.24388219451328,0.771898853704203));
#54043=CARTESIAN_POINT('Ctrl Pts',(-50.,-9.34425800352241,0.728158030239756));
#54044=CARTESIAN_POINT('Ctrl Pts',(-50.,-9.44424332627553,0.68185372865074));
#54045=CARTESIAN_POINT('Ctrl Pts',(-50.,-9.54380000381903,0.632963053309265));
#54046=CARTESIAN_POINT('Ctrl Pts',(-50.,-9.64288855622378,0.581447879194613));
#54047=CARTESIAN_POINT('Ctrl Pts',(-50.,-9.74146724538631,0.527299895441832));
#54048=CARTESIAN_POINT('Ctrl Pts',(-50.,-9.83125393359035,0.475330978595834));
#54049=CARTESIAN_POINT('Ctrl Pts',(-50.,-9.90105385380907,0.433097260939727));
#54050=CARTESIAN_POINT('Ctrl Pts',(-50.,-9.95114599336025,0.401850266969692));
#54051=CARTESIAN_POINT('Ctrl Pts',(-50.,-9.98174010098861,0.382417599459157));
#54052=CARTESIAN_POINT('Ctrl Pts',(-50.,-9.99295703981581,0.375246053138014));
#54053=CARTESIAN_POINT('',(-50.,-6.8122671513043,2.29198004120026));
#54054=CARTESIAN_POINT('Origin',(-50.,0.,0.));
#54055=CARTESIAN_POINT('',(-50.,-9.14990386923577,4.03475639707581));
#54056=CARTESIAN_POINT('Ctrl Pts',(-50.,-9.14990386923577,4.03475639707581));
#54057=CARTESIAN_POINT('Ctrl Pts',(-50.,-9.13577160343033,4.01614569996669));
#54058=CARTESIAN_POINT('Ctrl Pts',(-50.,-9.10709633384263,3.97431669461607));
#54059=CARTESIAN_POINT('Ctrl Pts',(-50.,-9.06450371311672,3.90166326358647));
#54060=CARTESIAN_POINT('Ctrl Pts',(-50.,-9.00794825534563,3.79330594308901));
#54061=CARTESIAN_POINT('Ctrl Pts',(-50.,-8.93534116084886,3.65684682750522));
#54062=CARTESIAN_POINT('Ctrl Pts',(-50.,-8.85834857876282,3.53174964938136));
#54063=CARTESIAN_POINT('Ctrl Pts',(-50.,-8.77716058006919,3.42378642402312));
#54064=CARTESIAN_POINT('Ctrl Pts',(-50.,-8.69226485417113,3.33012809006974));
#54065=CARTESIAN_POINT('Ctrl Pts',(-50.,-8.60460841273967,3.24456764186082));
#54066=CARTESIAN_POINT('Ctrl Pts',(-50.,-8.51516539363766,3.16038325236223));
#54067=CARTESIAN_POINT('Ctrl Pts',(-50.,-8.4243384303954,3.07426635319921));
#54068=CARTESIAN_POINT('Ctrl Pts',(-50.,-8.33184183835821,2.98721060740198));
#54069=CARTESIAN_POINT('Ctrl Pts',(-50.,-8.2370828133169,2.90227874531213));
#54070=CARTESIAN_POINT('Ctrl Pts',(-50.,-8.13939365460193,2.82329483425037));
#54071=CARTESIAN_POINT('Ctrl Pts',(-50.,-8.03835937937461,2.75296659957235));
#54072=CARTESIAN_POINT('Ctrl Pts',(-50.,-7.93399262158453,2.69188736687836));
#54073=CARTESIAN_POINT('Ctrl Pts',(-50.,-7.82659266808561,2.63932460382938));
#54074=CARTESIAN_POINT('Ctrl Pts',(-50.,-7.71666617412861,2.59365833862295));
#54075=CARTESIAN_POINT('Ctrl Pts',(-50.,-7.60482241577417,2.55297760756074));
#54076=CARTESIAN_POINT('Ctrl Pts',(-50.,-7.49168859641893,2.51552733857386));
#54077=CARTESIAN_POINT('Ctrl Pts',(-50.,-7.37786505179862,2.47974127678492));
#54078=CARTESIAN_POINT('Ctrl Pts',(-50.,-7.26387759821705,2.44432136933076));
#54079=CARTESIAN_POINT('Ctrl Pts',(-50.,-7.15012820840451,2.4083053284885));
#54080=CARTESIAN_POINT('Ctrl Pts',(-50.,-7.03685278876406,2.37112767623027));
#54081=CARTESIAN_POINT('Ctrl Pts',(-50.,-6.94670492800217,2.34023288057449));
#54082=CARTESIAN_POINT('Ctrl Pts',(-50.,-6.8793763726903,2.31637371632821));
#54083=CARTESIAN_POINT('Ctrl Pts',(-50.,-6.83461600336474,2.30016217089616));
#54084=CARTESIAN_POINT('Ctrl Pts',(-50.,-6.8122671513043,2.29198004120026));
#54085=CARTESIAN_POINT('',(-50.,-8.84053003053573,4.67386657695701));
#54086=CARTESIAN_POINT('Origin',(-50.,0.,0.));
#54087=CARTESIAN_POINT('',(-50.,-6.03932124977422,3.89701874412038));
#54088=CARTESIAN_POINT('Ctrl Pts',(-50.,-6.03932124977421,3.89701874412039));
#54089=CARTESIAN_POINT('Ctrl Pts',(-50.,-6.0565953297729,3.90728293824429));
#54090=CARTESIAN_POINT('Ctrl Pts',(-50.,-6.09105342163039,3.92794852152394));
#54091=CARTESIAN_POINT('Ctrl Pts',(-50.,-6.14247034880463,3.95935849016754));
#54092=CARTESIAN_POINT('Ctrl Pts',(-50.,-6.21048516503746,4.00206265639536));
#54093=CARTESIAN_POINT('Ctrl Pts',(-50.,-6.29463308326085,4.05676946424956));
#54094=CARTESIAN_POINT('Ctrl Pts',(-50.,-6.37801243240243,4.11264895980536));
#54095=CARTESIAN_POINT('Ctrl Pts',(-50.,-6.46083145580807,4.1693867325325));
#54096=CARTESIAN_POINT('Ctrl Pts',(-50.,-6.54344708143028,4.22644426515767));
#54097=CARTESIAN_POINT('Ctrl Pts',(-50.,-6.62638951409907,4.28302021638686));
#54098=CARTESIAN_POINT('Ctrl Pts',(-50.,-6.71027219290964,4.33817259947066));
#54099=CARTESIAN_POINT('Ctrl Pts',(-50.,-6.79571235355295,4.39092540044367));
#54100=CARTESIAN_POINT('Ctrl Pts',(-50.,-6.88325224876452,4.44037556328962));
#54101=CARTESIAN_POINT('Ctrl Pts',(-50.,-6.9732685530375,4.48581308997575));
#54102=CARTESIAN_POINT('Ctrl Pts',(-50.,-7.06592138953324,4.5267956450212));
#54103=CARTESIAN_POINT('Ctrl Pts',(-50.,-7.16121001331941,4.56309881747208));
#54104=CARTESIAN_POINT('Ctrl Pts',(-50.,-7.25900770064673,4.59469206087561));
#54105=CARTESIAN_POINT('Ctrl Pts',(-50.,-7.35910284385827,4.62170482170181));
#54106=CARTESIAN_POINT('Ctrl Pts',(-50.,-7.46123890856565,4.64440143603747));
#54107=CARTESIAN_POINT('Ctrl Pts',(-50.,-7.56514580946327,4.66314297047291));
#54108=CARTESIAN_POINT('Ctrl Pts',(-50.,-7.67055506601851,4.67833376211481));
#54109=CARTESIAN_POINT('Ctrl Pts',(-50.,-7.77721964274024,4.69037000103626));
#54110=CARTESIAN_POINT('Ctrl Pts',(-50.,-7.8849298684541,4.69959254734285));
#54111=CARTESIAN_POINT('Ctrl Pts',(-50.,-7.99353571494822,4.70622700687469));
#54112=CARTESIAN_POINT('Ctrl Pts',(-50.,-8.1029496259928,4.71036931800664));
#54113=CARTESIAN_POINT('Ctrl Pts',(-50.,-8.21312397255121,4.71203258951797));
#54114=CARTESIAN_POINT('Ctrl Pts',(-50.,-8.32403430863484,4.71117963661127));
#54115=CARTESIAN_POINT('Ctrl Pts',(-50.,-8.4356616058832,4.70775898013052));
#54116=CARTESIAN_POINT('Ctrl Pts',(-50.,-8.5479718655136,4.70174502276072));
#54117=CARTESIAN_POINT('Ctrl Pts',(-50.,-8.65141534429661,4.69387963058481));
#54118=CARTESIAN_POINT('Ctrl Pts',(-50.,-8.73262742272929,4.68611341617548));
#54119=CARTESIAN_POINT('Ctrl Pts',(-50.,-8.79131644357152,4.6796950122018));
#54120=CARTESIAN_POINT('Ctrl Pts',(-50.,-8.8273123005265,4.67546106956725));
#54121=CARTESIAN_POINT('Ctrl Pts',(-50.,-8.84053003053612,4.67386657695697));
#54122=CARTESIAN_POINT('',(-50.,-5.14318775290069,5.02073460645076));
#54123=CARTESIAN_POINT('Origin',(-50.,0.,0.));
#54124=CARTESIAN_POINT('',(-50.,-6.49316333848958,7.60518440668567));
#54125=CARTESIAN_POINT('Ctrl Pts',(-50.,-6.49316333848958,7.60518440668567));
#54126=CARTESIAN_POINT('Ctrl Pts',(-50.,-6.48850548581524,7.58228498765052));
#54127=CARTESIAN_POINT('Ctrl Pts',(-50.,-6.48081888588311,7.53215662286537));
#54128=CARTESIAN_POINT('Ctrl Pts',(-50.,-6.47396740292153,7.44821789782204));
#54129=CARTESIAN_POINT('Ctrl Pts',(-50.,-6.47002717553801,7.32605283195927));
#54130=CARTESIAN_POINT('Ctrl Pts',(-50.,-6.46381783511374,7.17160437943005));
#54131=CARTESIAN_POINT('Ctrl Pts',(-50.,-6.44872754699223,7.02548988707821));
#54132=CARTESIAN_POINT('Ctrl Pts',(-50.,-6.42242317562759,6.89299222970744));
#54133=CARTESIAN_POINT('Ctrl Pts',(-50.,-6.38657159771068,6.77177411160809));
#54134=CARTESIAN_POINT('Ctrl Pts',(-50.,-6.34471916009928,6.65665410688205));
#54135=CARTESIAN_POINT('Ctrl Pts',(-50.,-6.30066002212815,6.5419987212145));
#54136=CARTESIAN_POINT('Ctrl Pts',(-50.,-6.25619247809081,6.42500173364409));
#54137=CARTESIAN_POINT('Ctrl Pts',(-50.,-6.2106280007764,6.30643444970003));
#54138=CARTESIAN_POINT('Ctrl Pts',(-50.,-6.16210362315516,6.18879908596403));
#54139=CARTESIAN_POINT('Ctrl Pts',(-50.,-6.108358567083,6.07525130357771));
#54140=CARTESIAN_POINT('Ctrl Pts',(-50.,-6.04784410793973,5.96805062448362));
#54141=CARTESIAN_POINT('Ctrl Pts',(-50.,-5.98031419419066,5.86773709824143));
#54142=CARTESIAN_POINT('Ctrl Pts',(-50.,-5.906356307844,5.77378059171821));
#54143=CARTESIAN_POINT('Ctrl Pts',(-50.,-5.82712980893039,5.68494139022769));
#54144=CARTESIAN_POINT('Ctrl Pts',(-50.,-5.74401277228714,5.59976212994534));
#54145=CARTESIAN_POINT('Ctrl Pts',(-50.,-5.65833178588016,5.51693367893109));
#54146=CARTESIAN_POINT('Ctrl Pts',(-50.,-5.57130730604024,5.43530536621495));
#54147=CARTESIAN_POINT('Ctrl Pts',(-50.,-5.48397628091718,5.35393582972231));
#54148=CARTESIAN_POINT('Ctrl Pts',(-50.,-5.39711839642203,5.27213248760413));
#54149=CARTESIAN_POINT('Ctrl Pts',(-50.,-5.31119154860082,5.18948821771405));
#54150=CARTESIAN_POINT('Ctrl Pts',(-50.,-5.24337588200476,5.12253927774717));
#54151=CARTESIAN_POINT('Ctrl Pts',(-50.,-5.19306705314332,5.071830148219));
#54152=CARTESIAN_POINT('Ctrl Pts',(-50.,-5.1597732798141,5.03780325407688));
#54153=CARTESIAN_POINT('Ctrl Pts',(-50.,-5.14318775290069,5.02073460645076));
#54154=CARTESIAN_POINT('',(-50.,-5.93712762672243,8.04677050399782));
#54155=CARTESIAN_POINT('Origin',(-50.,0.,0.));
#54156=CARTESIAN_POINT('',(-50.,-3.75038736519794,6.13145585166881));
#54157=CARTESIAN_POINT('Ctrl Pts',(-50.,-3.75038736519793,6.13145585166881));
#54158=CARTESIAN_POINT('Ctrl Pts',(-50.,-3.7614973065729,6.1481985134482));
#54159=CARTESIAN_POINT('Ctrl Pts',(-50.,-3.78357651403939,6.1817683663582));
#54160=CARTESIAN_POINT('Ctrl Pts',(-50.,-3.81627329006595,6.23237673886416));
#54161=CARTESIAN_POINT('Ctrl Pts',(-50.,-3.859023878729,6.30036238594766));
#54162=CARTESIAN_POINT('Ctrl Pts',(-50.,-3.91110213900011,6.38616193008433));
#54163=CARTESIAN_POINT('Ctrl Pts',(-50.,-3.96197913233089,6.47268455970493));
#54164=CARTESIAN_POINT('Ctrl Pts',(-50.,-4.01197889710939,6.55973735411151));
#54165=CARTESIAN_POINT('Ctrl Pts',(-50.,-4.06165666819706,6.64698999124062));
#54166=CARTESIAN_POINT('Ctrl Pts',(-50.,-4.11183783259628,6.73395053478792));
#54167=CARTESIAN_POINT('Ctrl Pts',(-50.,-4.16348379256721,6.82003644526658));
#54168=CARTESIAN_POINT('Ctrl Pts',(-50.,-4.21757413484033,6.90463617300865));
#54169=CARTESIAN_POINT('Ctrl Pts',(-50.,-4.27498923356982,6.98717136730191));
#54170=CARTESIAN_POINT('Ctrl Pts',(-50.,-4.33637651734857,7.06716577496009));
#54171=CARTESIAN_POINT('Ctrl Pts',(-50.,-4.40207217433237,7.14429034032177));
#54172=CARTESIAN_POINT('Ctrl Pts',(-50.,-4.47217290162416,7.21834255288981));
#54173=CARTESIAN_POINT('Ctrl Pts',(-50.,-4.54657777868016,7.28923990788708));
#54174=CARTESIAN_POINT('Ctrl Pts',(-50.,-4.62503998887083,7.35700721943171));
#54175=CARTESIAN_POINT('Ctrl Pts',(-50.,-4.70721371156899,7.42177134000892));
#54176=CARTESIAN_POINT('Ctrl Pts',(-50.,-4.79269894740031,7.48374039375355));
#54177=CARTESIAN_POINT('Ctrl Pts',(-50.,-4.88107836846757,7.54316218647348));
#54178=CARTESIAN_POINT('Ctrl Pts',(-50.,-4.9719575030537,7.60028648840776));
#54179=CARTESIAN_POINT('Ctrl Pts',(-50.,-5.06499955030094,7.65532943098672));
#54180=CARTESIAN_POINT('Ctrl Pts',(-50.,-5.15997145275563,7.70842918324715));
#54181=CARTESIAN_POINT('Ctrl Pts',(-50.,-5.25675269887972,7.75963419345371));
#54182=CARTESIAN_POINT('Ctrl Pts',(-50.,-5.35529468870783,7.80893560674388));
#54183=CARTESIAN_POINT('Ctrl Pts',(-50.,-5.45559153104423,7.85628931405591));
#54184=CARTESIAN_POINT('Ctrl Pts',(-50.,-5.5576484178972,7.90164067817667));
#54185=CARTESIAN_POINT('Ctrl Pts',(-50.,-5.66144582368073,7.94495188520329));
#54186=CARTESIAN_POINT('Ctrl Pts',(-50.,-5.75805784341858,7.98274785508062));
#54187=CARTESIAN_POINT('Ctrl Pts',(-50.,-5.83459703193072,8.01098733792821));
#54188=CARTESIAN_POINT('Ctrl Pts',(-50.,-5.89025885371243,8.03066876757445));
#54189=CARTESIAN_POINT('Ctrl Pts',(-50.,-5.92452703906375,8.04247213408059));
#54190=CARTESIAN_POINT('Ctrl Pts',(-50.,-5.93712762672243,8.04677050399782));
#54191=CARTESIAN_POINT('',(-50.,-2.45543694297674,6.75507110762463));
#54192=CARTESIAN_POINT('Origin',(-50.,0.,0.));
#54193=CARTESIAN_POINT('',(-50.,-2.55037217513312,9.66931237308562));
#54194=CARTESIAN_POINT('Ctrl Pts',(-50.,-2.55037217513312,9.66931237308562));
#54195=CARTESIAN_POINT('Ctrl Pts',(-50.,-2.55611128043686,9.64665974290731));
#54196=CARTESIAN_POINT('Ctrl Pts',(-50.,-2.57093577554682,9.59816055611737));
#54197=CARTESIAN_POINT('Ctrl Pts',(-50.,-2.60118245057803,9.51956163099604));
#54198=CARTESIAN_POINT('Ctrl Pts',(-50.,-2.6506378639391,9.4077851093183));
#54199=CARTESIAN_POINT('Ctrl Pts',(-50.,-2.71205611361093,9.26593773005304));
#54200=CARTESIAN_POINT('Ctrl Pts',(-50.,-2.76185693608665,9.12774569066013));
#54201=CARTESIAN_POINT('Ctrl Pts',(-50.,-2.79564609540172,8.99695638729624));
#54202=CARTESIAN_POINT('Ctrl Pts',(-50.,-2.81593951016314,8.87218721998315));
#54203=CARTESIAN_POINT('Ctrl Pts',(-50.,-2.8281804649272,8.7503085875302));
#54204=CARTESIAN_POINT('Ctrl Pts',(-50.,-2.838231660712,8.62789111098118));
#54205=CARTESIAN_POINT('Ctrl Pts',(-50.,-2.84893087833482,8.50318672326558));
#54206=CARTESIAN_POINT('Ctrl Pts',(-50.,-2.85932311928695,8.37659160589212));
#54207=CARTESIAN_POINT('Ctrl Pts',(-50.,-2.8666442371861,8.24955186700095));
#54208=CARTESIAN_POINT('Ctrl Pts',(-50.,-2.86748815125169,8.12392974416385));
#54209=CARTESIAN_POINT('Ctrl Pts',(-50.,-2.85947913898695,8.00108902987832));
#54210=CARTESIAN_POINT('Ctrl Pts',(-50.,-2.84216119689693,7.88140953422486));
#54211=CARTESIAN_POINT('Ctrl Pts',(-50.,-2.81629364412744,7.76466852264525));
#54212=CARTESIAN_POINT('Ctrl Pts',(-50.,-2.78345892001629,7.65025207826714));
#54213=CARTESIAN_POINT('Ctrl Pts',(-50.,-2.74553095355499,7.53744508591865));
#54214=CARTESIAN_POINT('Ctrl Pts',(-50.,-2.70427297026251,7.42564364342468));
#54215=CARTESIAN_POINT('Ctrl Pts',(-50.,-2.66128382072048,7.31434056822034));
#54216=CARTESIAN_POINT('Ctrl Pts',(-50.,-2.61790620462629,7.20313763732345));
#54217=CARTESIAN_POINT('Ctrl Pts',(-50.,-2.57514309471485,7.09174914908801));
#54218=CARTESIAN_POINT('Ctrl Pts',(-50.,-2.53358368474749,6.98000697278327));
#54219=CARTESIAN_POINT('Ctrl Pts',(-50.,-2.50153193679118,6.89026394714059));
#54220=CARTESIAN_POINT('Ctrl Pts',(-50.,-2.47820711493347,6.82274841734025));
#54221=CARTESIAN_POINT('Ctrl Pts',(-50.,-2.46297417772978,6.77764561818537));
#54222=CARTESIAN_POINT('Ctrl Pts',(-50.,-2.45543694297674,6.75507110762463));
#54223=CARTESIAN_POINT('',(-50.,-1.85780428234483,9.82591284555797));
#54224=CARTESIAN_POINT('Origin',(-50.,0.,0.));
#54225=CARTESIAN_POINT('',(-50.,-0.718643267461628,7.15148293042304));
#54226=CARTESIAN_POINT('Ctrl Pts',(-50.,-0.718643267461623,7.15148293042304));
#54227=CARTESIAN_POINT('Ctrl Pts',(-50.,-0.721388610069065,7.17138797035723));
#54228=CARTESIAN_POINT('Ctrl Pts',(-50.,-0.726715875322121,7.21121317182152));
#54229=CARTESIAN_POINT('Ctrl Pts',(-50.,-0.734216502709279,7.2709963393441));
#54230=CARTESIAN_POINT('Ctrl Pts',(-50.,-0.743235585416284,7.35079807608913));
#54231=CARTESIAN_POINT('Ctrl Pts',(-50.,-0.752929449590466,7.45069670452966));
#54232=CARTESIAN_POINT('Ctrl Pts',(-50.,-0.761227274615912,7.55072560028829));
#54233=CARTESIAN_POINT('Ctrl Pts',(-50.,-0.768504714146027,7.65085154280962));
#54234=CARTESIAN_POINT('Ctrl Pts',(-50.,-0.775405338877351,7.75101782957587));
#54235=CARTESIAN_POINT('Ctrl Pts',(-50.,-0.782886239966145,7.85113936329068));
#54236=CARTESIAN_POINT('Ctrl Pts',(-50.,-0.792066365329069,7.95110843081948));
#54237=CARTESIAN_POINT('Ctrl Pts',(-50.,-0.804093633570273,8.05079907170372));
#54238=CARTESIAN_POINT('Ctrl Pts',(-50.,-0.82001217136434,8.15007218998677));
#54239=CARTESIAN_POINT('Ctrl Pts',(-50.,-0.840611930230858,8.24877960511329));
#54240=CARTESIAN_POINT('Ctrl Pts',(-50.,-0.86633857713272,8.34677071475058));
#54241=CARTESIAN_POINT('Ctrl Pts',(-50.,-0.897367099160985,8.4439050185459));
#54242=CARTESIAN_POINT('Ctrl Pts',(-50.,-0.933642367528788,8.5400643944807));
#54243=CARTESIAN_POINT('Ctrl Pts',(-50.,-0.974931241694467,8.63516410958082));
#54244=CARTESIAN_POINT('Ctrl Pts',(-50.,-1.02086710880846,8.72916840803945));
#54245=CARTESIAN_POINT('Ctrl Pts',(-50.,-1.07099928020948,8.82209124999857));
#54246=CARTESIAN_POINT('Ctrl Pts',(-50.,-1.12484423754393,8.91397482898789));
#54247=CARTESIAN_POINT('Ctrl Pts',(-50.,-1.18193820283021,9.00487302535333));
#54248=CARTESIAN_POINT('Ctrl Pts',(-50.,-1.24188395306769,9.09483443436949));
#54249=CARTESIAN_POINT('Ctrl Pts',(-50.,-1.30441156144786,9.18388242219763));
#54250=CARTESIAN_POINT('Ctrl Pts',(-50.,-1.3693914299125,9.27200835121914));
#54251=CARTESIAN_POINT('Ctrl Pts',(-50.,-1.43678361338666,9.35918315674388));
#54252=CARTESIAN_POINT('Ctrl Pts',(-50.,-1.50660194229105,9.44536454178638));
#54253=CARTESIAN_POINT('Ctrl Pts',(-50.,-1.57887480066182,9.53050553264656));
#54254=CARTESIAN_POINT('Ctrl Pts',(-50.,-1.65360100339141,9.61456358834088));
#54255=CARTESIAN_POINT('Ctrl Pts',(-50.,-1.72424636870649,9.69053496490015));
#54256=CARTESIAN_POINT('Ctrl Pts',(-50.,-1.78095314232183,9.74918696909221));
#54257=CARTESIAN_POINT('Ctrl Pts',(-50.,-1.82256325859186,9.79107008384009));
#54258=CARTESIAN_POINT('Ctrl Pts',(-50.,-1.8483165379591,9.81657295799161));
#54259=CARTESIAN_POINT('Ctrl Pts',(-50.,-1.85780428234511,9.82591284555825));
#54260=CARTESIAN_POINT('',(-50.,0.718643267461623,7.15148293042304));
#54261=CARTESIAN_POINT('Origin',(-50.,0.,0.));
#54262=CARTESIAN_POINT('',(-50.,1.89755147577054,9.81831443766195));
#54263=CARTESIAN_POINT('Ctrl Pts',(-50.,1.89755147577054,9.81831443766194));
#54264=CARTESIAN_POINT('Ctrl Pts',(-50.,1.88255211267964,9.80039522756355));
#54265=CARTESIAN_POINT('Ctrl Pts',(-50.,1.84815269559462,9.76313107751608));
#54266=CARTESIAN_POINT('Ctrl Pts',(-50.,1.78679858751167,9.70543943338958));
#54267=CARTESIAN_POINT('Ctrl Pts',(-50.,1.69374278455301,9.62619016686422));
#54268=CARTESIAN_POINT('Ctrl Pts',(-50.,1.576861582378,9.52503847397034));
#54269=CARTESIAN_POINT('Ctrl Pts',(-50.,1.47203331296336,9.42213951575228));
#54270=CARTESIAN_POINT('Ctrl Pts',(-50.,1.38484298036779,9.31896299195203));
#54271=CARTESIAN_POINT('Ctrl Pts',(-50.,1.31242393260393,9.21535483920498));
#54272=CARTESIAN_POINT('Ctrl Pts',(-50.,1.24851405668088,9.11085713692575));
#54273=CARTESIAN_POINT('Ctrl Pts',(-50.,1.18634328973517,9.00492385207762));
#54274=CARTESIAN_POINT('Ctrl Pts',(-50.,1.12259642171968,8.89721129760285));
#54275=CARTESIAN_POINT('Ctrl Pts',(-50.,1.05830577327405,8.78766206238304));
#54276=CARTESIAN_POINT('Ctrl Pts',(-50.,0.996589197042052,8.67637972666424));
#54277=CARTESIAN_POINT('Ctrl Pts',(-50.,0.941323460369316,8.56356426545847));
#54278=CARTESIAN_POINT('Ctrl Pts',(-50.,0.895240742652423,8.44941362598824));
#54279=CARTESIAN_POINT('Ctrl Pts',(-50.,0.858916682261844,8.33407215281038));
#54280=CARTESIAN_POINT('Ctrl Pts',(-50.,0.831570515383446,8.21766862525226));
#54281=CARTESIAN_POINT('Ctrl Pts',(-50.,0.811510144890448,8.10033651802127));
#54282=CARTESIAN_POINT('Ctrl Pts',(-50.,0.796736942256154,7.98224460192821));
#54283=CARTESIAN_POINT('Ctrl Pts',(-50.,0.785400272847098,7.86361381479518));
#54284=CARTESIAN_POINT('Ctrl Pts',(-50.,0.775839563797132,7.74468091618948));
#54285=CARTESIAN_POINT('Ctrl Pts',(-50.,0.766672302003445,7.62566969516693));
#54286=CARTESIAN_POINT('Ctrl Pts',(-50.,0.756870878958096,7.5067579169994));
#54287=CARTESIAN_POINT('Ctrl Pts',(-50.,0.745831500234843,7.38804974272502));
#54288=CARTESIAN_POINT('Ctrl Pts',(-50.,0.735771087779772,7.29328733826105));
#54289=CARTESIAN_POINT('Ctrl Pts',(-50.,0.72749213560466,7.22233768688913));
#54290=CARTESIAN_POINT('Ctrl Pts',(-50.,0.721647166649911,7.17509214524366));
#54291=CARTESIAN_POINT('Ctrl Pts',(-50.,0.718643267461623,7.15148293042304));
#54292=CARTESIAN_POINT('',(-50.,2.58947998462545,9.65891264114259));
#54293=CARTESIAN_POINT('Origin',(-50.,0.,0.));
#54294=CARTESIAN_POINT('',(-50.,2.45543694297674,6.75507110762463));
#54295=CARTESIAN_POINT('Ctrl Pts',(-50.,2.45543694297675,6.75507110762463));
#54296=CARTESIAN_POINT('Ctrl Pts',(-50.,2.46159994790965,6.77419608843537));
#54297=CARTESIAN_POINT('Ctrl Pts',(-50.,2.47407975508802,6.8123887688799));
#54298=CARTESIAN_POINT('Ctrl Pts',(-50.,2.49326086758344,6.8695059418988));
#54299=CARTESIAN_POINT('Ctrl Pts',(-50.,2.5197596307744,6.94531805563895));
#54300=CARTESIAN_POINT('Ctrl Pts',(-50.,2.55437015138428,7.03952961984441));
#54301=CARTESIAN_POINT('Ctrl Pts',(-50.,2.59029498067661,7.13325283216217));
#54302=CARTESIAN_POINT('Ctrl Pts',(-50.,2.62718125254576,7.22662075191781));
#54303=CARTESIAN_POINT('Ctrl Pts',(-50.,2.66442452752942,7.31986152676826));
#54304=CARTESIAN_POINT('Ctrl Pts',(-50.,2.70112557395893,7.41331375298832));
#54305=CARTESIAN_POINT('Ctrl Pts',(-50.,2.73622951961898,7.50736587770304));
#54306=CARTESIAN_POINT('Ctrl Pts',(-50.,2.76864747338962,7.60240247767684));
#54307=CARTESIAN_POINT('Ctrl Pts',(-50.,2.79737835816915,7.69875126136884));
#54308=CARTESIAN_POINT('Ctrl Pts',(-50.,2.82164615909785,7.79662146983088));
#54309=CARTESIAN_POINT('Ctrl Pts',(-50.,2.84098400021345,7.89607078269802));
#54310=CARTESIAN_POINT('Ctrl Pts',(-50.,2.85517326277626,7.9970485375799));
#54311=CARTESIAN_POINT('Ctrl Pts',(-50.,2.86421236488386,8.099424390731));
#54312=CARTESIAN_POINT('Ctrl Pts',(-50.,2.8682745946465,8.20302084448955));
#54313=CARTESIAN_POINT('Ctrl Pts',(-50.,2.86767474496505,8.30764661663281));
#54314=CARTESIAN_POINT('Ctrl Pts',(-50.,2.86282492937103,8.41311873833255));
#54315=CARTESIAN_POINT('Ctrl Pts',(-50.,2.85417908993455,8.51926543389428));
#54316=CARTESIAN_POINT('Ctrl Pts',(-50.,2.84217845398458,8.62593402210748));
#54317=CARTESIAN_POINT('Ctrl Pts',(-50.,2.82720199177778,8.73299593720093));
#54318=CARTESIAN_POINT('Ctrl Pts',(-50.,2.80950303716262,8.84035511450549));
#54319=CARTESIAN_POINT('Ctrl Pts',(-50.,2.78919460623265,8.94794754130566));
#54320=CARTESIAN_POINT('Ctrl Pts',(-50.,2.76630007756038,9.05572969970197));
#54321=CARTESIAN_POINT('Ctrl Pts',(-50.,2.74078863839312,9.16366948222194));
#54322=CARTESIAN_POINT('Ctrl Pts',(-50.,2.71261433447332,9.27173688239595));
#54323=CARTESIAN_POINT('Ctrl Pts',(-50.,2.68175977570501,9.37989305792331));
#54324=CARTESIAN_POINT('Ctrl Pts',(-50.,2.65107324582199,9.47899277830907));
#54325=CARTESIAN_POINT('Ctrl Pts',(-50.,2.62543035908099,9.55644055509564));
#54326=CARTESIAN_POINT('Ctrl Pts',(-50.,2.60611334216463,9.61222989040654));
#54327=CARTESIAN_POINT('Ctrl Pts',(-50.,2.59397572160348,9.64638111520543));
#54328=CARTESIAN_POINT('Ctrl Pts',(-50.,2.58947998462545,9.65891264114259));
#54329=CARTESIAN_POINT('',(-50.,3.75038736519793,6.13145585166881));
#54330=CARTESIAN_POINT('Origin',(-50.,0.,0.));
#54331=CARTESIAN_POINT('',(-50.,5.96964178495622,8.0226789141349));
#54332=CARTESIAN_POINT('Ctrl Pts',(-50.,5.96964178495622,8.0226789141349));
#54333=CARTESIAN_POINT('Ctrl Pts',(-50.,5.94835297189343,8.0130422434411));
#54334=CARTESIAN_POINT('Ctrl Pts',(-50.,5.9011918592682,7.9943937520678));
#54335=CARTESIAN_POINT('Ctrl Pts',(-50.,5.82088225169809,7.96903592659697));
#54336=CARTESIAN_POINT('Ctrl Pts',(-50.,5.70265690217233,7.93801020438781));
#54337=CARTESIAN_POINT('Ctrl Pts',(-50.,5.55346250303877,7.89758853118705));
#54338=CARTESIAN_POINT('Ctrl Pts',(-50.,5.41436931107715,7.85036305479183));
#54339=CARTESIAN_POINT('Ctrl Pts',(-50.,5.29104691989087,7.79523468647088));
#54340=CARTESIAN_POINT('Ctrl Pts',(-50.,5.18084571969554,7.73330841361203));
#54341=CARTESIAN_POINT('Ctrl Pts',(-50.,5.07792505734327,7.66688869302314));
#54342=CARTESIAN_POINT('Ctrl Pts',(-50.,4.97594840210465,7.59842098612655));
#54343=CARTESIAN_POINT('Ctrl Pts',(-50.,4.87177973271099,7.52903405731413));
#54344=CARTESIAN_POINT('Ctrl Pts',(-50.,4.76632422816958,7.45822827381644));
#54345=CARTESIAN_POINT('Ctrl Pts',(-50.,4.66243591843161,7.38474417264741));
#54346=CARTESIAN_POINT('Ctrl Pts',(-50.,4.56369441608956,7.30707985875561));
#54347=CARTESIAN_POINT('Ctrl Pts',(-50.,4.4726472158023,7.22422822821349));
#54348=CARTESIAN_POINT('Ctrl Pts',(-50.,4.38987557857684,7.13606957084443));
#54349=CARTESIAN_POINT('Ctrl Pts',(-50.,4.31473193577955,7.04305867353628));
#54350=CARTESIAN_POINT('Ctrl Pts',(-50.,4.24574967308284,6.94604996627335));
#54351=CARTESIAN_POINT('Ctrl Pts',(-50.,4.18120131531612,6.84606267872027));
#54352=CARTESIAN_POINT('Ctrl Pts',(-50.,4.11951535961712,6.74409882925098));
#54353=CARTESIAN_POINT('Ctrl Pts',(-50.,4.05929840765689,6.64109222642907));
#54354=CARTESIAN_POINT('Ctrl Pts',(-50.,3.99940195660266,6.53784434718121));
#54355=CARTESIAN_POINT('Ctrl Pts',(-50.,3.93897729264122,6.43496121510494));
#54356=CARTESIAN_POINT('Ctrl Pts',(-50.,3.87752560957259,6.33279865263617));
#54357=CARTESIAN_POINT('Ctrl Pts',(-50.,3.82734562477572,6.25178572573963));
#54358=CARTESIAN_POINT('Ctrl Pts',(-50.,3.78910264658076,6.19145440139071));
#54359=CARTESIAN_POINT('Ctrl Pts',(-50.,3.7633374392529,6.15142367620606));
#54360=CARTESIAN_POINT('Ctrl Pts',(-50.,3.75038736519793,6.13145585166881));
#54361=CARTESIAN_POINT('',(-50.,6.52388598275276,7.57884632935924));
#54362=CARTESIAN_POINT('Origin',(-50.,0.,0.));
#54363=CARTESIAN_POINT('',(-50.,5.14318775290069,5.02073460645077));
#54364=CARTESIAN_POINT('Ctrl Pts',(-50.,5.14318775290069,5.02073460645076));
#54365=CARTESIAN_POINT('Ctrl Pts',(-50.,5.15703844666268,5.03529159113598));
#54366=CARTESIAN_POINT('Ctrl Pts',(-50.,5.18485354740602,5.06428722179623));
#54367=CARTESIAN_POINT('Ctrl Pts',(-50.,5.22691734521339,5.10742564369892));
#54368=CARTESIAN_POINT('Ctrl Pts',(-50.,5.28368554926634,5.16423261553338));
#54369=CARTESIAN_POINT('Ctrl Pts',(-50.,5.35574541658332,5.23409735978387));
#54370=CARTESIAN_POINT('Ctrl Pts',(-50.,5.42877754716296,5.30295185702147));
#54371=CARTESIAN_POINT('Ctrl Pts',(-50.,5.50252175190725,5.37106909242141));
#54372=CARTESIAN_POINT('Ctrl Pts',(-50.,5.57653243923659,5.43891687637388));
#54373=CARTESIAN_POINT('Ctrl Pts',(-50.,5.65014634083023,5.50719043557996));
#54374=CARTESIAN_POINT('Ctrl Pts',(-50.,5.72258159055366,5.57669744070723));
#54375=CARTESIAN_POINT('Ctrl Pts',(-50.,5.79302399301176,5.64825683559838));
#54376=CARTESIAN_POINT('Ctrl Pts',(-50.,5.86071379627312,5.72259822644884));
#54377=CARTESIAN_POINT('Ctrl Pts',(-50.,5.92504262139805,5.80024683316115));
#54378=CARTESIAN_POINT('Ctrl Pts',(-50.,5.98561485393513,5.88145719317904));
#54379=CARTESIAN_POINT('Ctrl Pts',(-50.,6.04221154361855,5.96627851638222));
#54380=CARTESIAN_POINT('Ctrl Pts',(-50.,6.09477471117184,6.05459405347559));
#54381=CARTESIAN_POINT('Ctrl Pts',(-50.,6.14338347043832,6.14616869769857));
#54382=CARTESIAN_POINT('Ctrl Pts',(-50.,6.18823844577549,6.2406935262026));
#54383=CARTESIAN_POINT('Ctrl Pts',(-50.,6.22963155144596,6.33782488040965));
#54384=CARTESIAN_POINT('Ctrl Pts',(-50.,6.2678972444421,6.43721103768399));
#54385=CARTESIAN_POINT('Ctrl Pts',(-50.,6.30336681095649,6.53852299564495));
#54386=CARTESIAN_POINT('Ctrl Pts',(-50.,6.33632590879467,6.64148049150319));
#54387=CARTESIAN_POINT('Ctrl Pts',(-50.,6.36696110296949,6.74588705654512));
#54388=CARTESIAN_POINT('Ctrl Pts',(-50.,6.39534644338642,6.85163598146165));
#54389=CARTESIAN_POINT('Ctrl Pts',(-50.,6.42148411170256,6.95867791439771));
#54390=CARTESIAN_POINT('Ctrl Pts',(-50.,6.44533241567678,7.06699729667253));
#54391=CARTESIAN_POINT('Ctrl Pts',(-50.,6.46683693263443,7.17658703219621));
#54392=CARTESIAN_POINT('Ctrl Pts',(-50.,6.48596514159778,7.28741967054497));
#54393=CARTESIAN_POINT('Ctrl Pts',(-50.,6.50131529073571,7.39001981975663));
#54394=CARTESIAN_POINT('Ctrl Pts',(-50.,6.51181517907743,7.47092388711063));
#54395=CARTESIAN_POINT('Ctrl Pts',(-50.,6.51861723362263,7.52956968091507));
#54396=CARTESIAN_POINT('Ctrl Pts',(-50.,6.52249927647781,7.56560518745274));
#54397=CARTESIAN_POINT('Ctrl Pts',(-50.,6.52388598275281,7.57884632935963));
#54398=CARTESIAN_POINT('',(-50.,6.03932124977421,3.89701874412038));
#54399=CARTESIAN_POINT('Origin',(-50.,0.,0.));
#54400=CARTESIAN_POINT('',(-50.,8.85937132577942,4.63805343996351));
#54401=CARTESIAN_POINT('Ctrl Pts',(-50.,8.85937132577942,4.63805343996351));
#54402=CARTESIAN_POINT('Ctrl Pts',(-50.,8.83600957326198,4.63860796949123));
#54403=CARTESIAN_POINT('Ctrl Pts',(-50.,8.78542760184506,4.64226869921732));
#54404=CARTESIAN_POINT('Ctrl Pts',(-50.,8.70206879749976,4.65426712072998));
#54405=CARTESIAN_POINT('Ctrl Pts',(-50.,8.58208988181924,4.67760996762605));
#54406=CARTESIAN_POINT('Ctrl Pts',(-50.,8.43013206622476,4.70592432223511));
#54407=CARTESIAN_POINT('Ctrl Pts',(-50.,8.2843230642502,4.72372591244527));
#54408=CARTESIAN_POINT('Ctrl Pts',(-50.,8.14929412649754,4.72756454905465));
#54409=CARTESIAN_POINT('Ctrl Pts',(-50.,8.02313747309844,4.71958541389958));
#54410=CARTESIAN_POINT('Ctrl Pts',(-50.,7.9015907237349,4.70439891524807));
#54411=CARTESIAN_POINT('Ctrl Pts',(-50.,7.78000590743498,4.68695765535521));
#54412=CARTESIAN_POINT('Ctrl Pts',(-50.,7.65604731918147,4.66963928443128));
#54413=CARTESIAN_POINT('Ctrl Pts',(-50.,7.53031371454558,4.65160090645339));
#54414=CARTESIAN_POINT('Ctrl Pts',(-50.,7.40483002515176,4.63046946729401));
#54415=CARTESIAN_POINT('Ctrl Pts',(-50.,7.28216972266428,4.60333867057275));
#54416=CARTESIAN_POINT('Ctrl Pts',(-50.,7.16419105444418,4.56819583049617));
#54417=CARTESIAN_POINT('Ctrl Pts',(-50.,7.05136577826386,4.52468089222283));
#54418=CARTESIAN_POINT('Ctrl Pts',(-50.,6.94330777957998,4.47348457408032));
#54419=CARTESIAN_POINT('Ctrl Pts',(-50.,6.83906640781858,4.4160130309926));
#54420=CARTESIAN_POINT('Ctrl Pts',(-50.,6.73752748880879,4.35393408054299));
#54421=CARTESIAN_POINT('Ctrl Pts',(-50.,6.63770990687462,4.2888323596294));
#54422=CARTESIAN_POINT('Ctrl Pts',(-50.,6.53876341785232,4.22215377357323));
#54423=CARTESIAN_POINT('Ctrl Pts',(-50.,6.44000100425059,4.15511874483725));
#54424=CARTESIAN_POINT('Ctrl Pts',(-50.,6.34092094513049,4.08864152493875));
#54425=CARTESIAN_POINT('Ctrl Pts',(-50.,6.24122821720367,4.02325912271413));
#54426=CARTESIAN_POINT('Ctrl Pts',(-50.,6.16086742147114,3.97204127711522));
#54427=CARTESIAN_POINT('Ctrl Pts',(-50.,6.10023490810719,3.93427763849175));
#54428=CARTESIAN_POINT('Ctrl Pts',(-50.,6.05965257770704,3.90939030583537));
#54429=CARTESIAN_POINT('Ctrl Pts',(-50.,6.03932124977421,3.89701874412038));
#54430=CARTESIAN_POINT('',(-50.,9.16615635178499,3.9976965535958));
#54431=CARTESIAN_POINT('Origin',(-50.,0.,0.));
#54432=CARTESIAN_POINT('',(-50.,6.8122671513043,2.29198004120026));
#54433=CARTESIAN_POINT('Ctrl Pts',(-50.,6.8122671513043,2.29198004120026));
#54434=CARTESIAN_POINT('Ctrl Pts',(-50.,6.8310622341282,2.29908584041335));
#54435=CARTESIAN_POINT('Ctrl Pts',(-50.,6.86870350660446,2.31314148102898));
#54436=CARTESIAN_POINT('Ctrl Pts',(-50.,6.92531873868941,2.33375705829959));
#54437=CARTESIAN_POINT('Ctrl Pts',(-50.,7.00111274457534,2.36030757076476));
#54438=CARTESIAN_POINT('Ctrl Pts',(-50.,7.09634961812101,2.39198792562662));
#54439=CARTESIAN_POINT('Ctrl Pts',(-50.,7.19202414084635,2.42233623016115));
#54440=CARTESIAN_POINT('Ctrl Pts',(-50.,7.28802033430286,2.45171132733138));
#54441=CARTESIAN_POINT('Ctrl Pts',(-50.,7.3841397096708,2.4807280346756));
#54442=CARTESIAN_POINT('Ctrl Pts',(-50.,7.4800863304027,2.5103005111467));
#54443=CARTESIAN_POINT('Ctrl Pts',(-50.,7.57550619462173,2.54149568187359));
#54444=CARTESIAN_POINT('Ctrl Pts',(-50.,7.67002106404108,2.5754046559055));
#54445=CARTESIAN_POINT('Ctrl Pts',(-50.,7.76326299008741,2.61301442971916));
#54446=CARTESIAN_POINT('Ctrl Pts',(-50.,7.85491172665132,2.65506217582471));
#54447=CARTESIAN_POINT('Ctrl Pts',(-50.,7.94472127708621,2.70194887521209));
#54448=CARTESIAN_POINT('Ctrl Pts',(-50.,8.03251572538561,2.75381386341092));
#54449=CARTESIAN_POINT('Ctrl Pts',(-50.,8.11819217840571,2.81057710920625));
#54450=CARTESIAN_POINT('Ctrl Pts',(-50.,8.201719906256,2.87199246251599));
#54451=CARTESIAN_POINT('Ctrl Pts',(-50.,8.28314562863609,2.93769454582461));
#54452=CARTESIAN_POINT('Ctrl Pts',(-50.,8.36258324333989,3.00724707660037));
#54453=CARTESIAN_POINT('Ctrl Pts',(-50.,8.44018147897284,3.08018804824792));
#54454=CARTESIAN_POINT('Ctrl Pts',(-50.,8.51609606529771,3.15607730017284));
#54455=CARTESIAN_POINT('Ctrl Pts',(-50.,8.59046276963722,3.23453838205034));
#54456=CARTESIAN_POINT('Ctrl Pts',(-50.,8.66336443667969,3.31531333416059));
#54457=CARTESIAN_POINT('Ctrl Pts',(-50.,8.7348214836506,3.3982738856883));
#54458=CARTESIAN_POINT('Ctrl Pts',(-50.,8.80481446318767,3.48337462556297));
#54459=CARTESIAN_POINT('Ctrl Pts',(-50.,8.87329906122102,3.57061962548306));
#54460=CARTESIAN_POINT('Ctrl Pts',(-50.,8.94022316573707,3.66002610520606));
#54461=CARTESIAN_POINT('Ctrl Pts',(-50.,9.0055455660548,3.75158344307814));
#54462=CARTESIAN_POINT('Ctrl Pts',(-50.,9.06389210891971,3.83736280325601));
#54463=CARTESIAN_POINT('Ctrl Pts',(-50.,9.10845514068543,3.90569911841461));
#54464=CARTESIAN_POINT('Ctrl Pts',(-50.,9.1400290363678,3.95558585200609));
#54465=CARTESIAN_POINT('Ctrl Pts',(-50.,9.15916185644175,3.9863683662662));
#54466=CARTESIAN_POINT('Ctrl Pts',(-50.,9.16615635178519,3.99769655359614));
#54467=CARTESIAN_POINT('',(-50.,7.13209349341826,0.890729280500491));
#54468=CARTESIAN_POINT('Origin',(-50.,0.,0.));
#54469=CARTESIAN_POINT('Ctrl Pts',(-50.,9.99439372247306,0.334804600014792));
#54470=CARTESIAN_POINT('Ctrl Pts',(-50.,9.97358611210015,0.345440498390202));
#54471=CARTESIAN_POINT('Ctrl Pts',(-50.,9.92960166167783,0.370685396797523));
#54472=CARTESIAN_POINT('Ctrl Pts',(-50.,9.85970389408656,0.417663630762109));
#54473=CARTESIAN_POINT('Ctrl Pts',(-50.,9.76173470794663,0.490751709654424));
#54474=CARTESIAN_POINT('Ctrl Pts',(-50.,9.63711058491003,0.582194086890199));
#54475=CARTESIAN_POINT('Ctrl Pts',(-50.,9.51346503399365,0.661496920442432));
#54476=CARTESIAN_POINT('Ctrl Pts',(-50.,9.39347368681776,0.723542272923875));
#54477=CARTESIAN_POINT('Ctrl Pts',(-50.,9.27634845263042,0.771090641047727));
#54478=CARTESIAN_POINT('Ctrl Pts',(-50.,9.1602494406401,0.810145236641718));
#54479=CARTESIAN_POINT('Ctrl Pts',(-50.,9.04313782728701,0.847184879177382));
#54480=CARTESIAN_POINT('Ctrl Pts',(-50.,8.92394083882956,0.885365181899305));
#54481=CARTESIAN_POINT('Ctrl Pts',(-50.,8.80283221651881,0.923666931425907));
#54482=CARTESIAN_POINT('Ctrl Pts',(-50.,8.68060673111004,0.95907349496179));
#54483=CARTESIAN_POINT('Ctrl Pts',(-50.,8.55832200571467,0.987849802439111));
#54484=CARTESIAN_POINT('Ctrl Pts',(-50.,8.43677899171613,1.00737622330388));
#54485=CARTESIAN_POINT('Ctrl Pts',(-50.,8.31624650623966,1.017123671327));
#54486=CARTESIAN_POINT('Ctrl Pts',(-50.,8.19667636355292,1.01788199103989));
#54487=CARTESIAN_POINT('Ctrl Pts',(-50.,8.0778221648407,1.01133055607812));
#54488=CARTESIAN_POINT('Ctrl Pts',(-50.,7.95940371279084,0.999455440216893));
#54489=CARTESIAN_POINT('Ctrl Pts',(-50.,7.84122460090589,0.984110042106143));
#54490=CARTESIAN_POINT('Ctrl Pts',(-50.,7.72314614047142,0.966965984543333));
#54491=CARTESIAN_POINT('Ctrl Pts',(-50.,7.60507887157754,0.949420915891057));
#54492=CARTESIAN_POINT('Ctrl Pts',(-50.,7.4869674381447,0.932516236860827));
#54493=CARTESIAN_POINT('Ctrl Pts',(-50.,7.36877903277666,0.916863781503487));
#54494=CARTESIAN_POINT('Ctrl Pts',(-50.,7.27415386726379,0.90558533966873));
#54495=CARTESIAN_POINT('Ctrl Pts',(-50.,7.20314083161155,0.897868938540711));
#54496=CARTESIAN_POINT('Ctrl Pts',(-50.,7.15577920638447,0.893054239868309));
#54497=CARTESIAN_POINT('Ctrl Pts',(-50.,7.13209349341826,0.890729280500491));
#54498=CARTESIAN_POINT('Origin',(-35.75,0.,0.));
#54499=CARTESIAN_POINT('',(-21.5,5.93712762672243,-8.04677050399782));
#54500=CARTESIAN_POINT('Origin',(-21.5,0.,0.));
#54501=CARTESIAN_POINT('Ctrl Pts',(-21.5,5.93712762672243,-8.04677050399782));
#54502=CARTESIAN_POINT('Ctrl Pts',(-26.3333333333333,5.93712762672243,-8.04677050399782));
#54503=CARTESIAN_POINT('Ctrl Pts',(-31.1666666666667,5.93712762672243,-8.04677050399782));
#54504=CARTESIAN_POINT('Ctrl Pts',(-40.6666666666667,5.93712762672243,-8.04677050399782));
#54505=CARTESIAN_POINT('Ctrl Pts',(-45.3333333333333,5.93712762672243,-8.04677050399782));
#54506=CARTESIAN_POINT('Ctrl Pts',(-50.,5.93712762672243,-8.04677050399782));
#54507=CARTESIAN_POINT('Origin',(-21.25,0.,0.));
#54508=CARTESIAN_POINT('Ctrl Pts',(-21.,5.38825861761966,-7.82410819644306));
#54509=CARTESIAN_POINT('Ctrl Pts',(-21.1171767610852,5.51032506808644,-7.88231976704313));
#54510=CARTESIAN_POINT('Ctrl Pts',(-21.2874825276342,5.69235044789971,-7.96327099664331));
#54511=CARTESIAN_POINT('Ctrl Pts',(-21.5,5.93712762672243,-8.04677050399782));
#54512=CARTESIAN_POINT('Ctrl Pts',(-50.,6.6617400018565,-8.24507247679879));
#54513=CARTESIAN_POINT('Ctrl Pts',(-21.,6.6617400018565,-8.24507247679879));
#54514=CARTESIAN_POINT('Ctrl Pts',(-50.,6.63837938775657,-8.24010262588658));
#54515=CARTESIAN_POINT('Ctrl Pts',(-21.,6.63837938775657,-8.24010262588658));
#54516=CARTESIAN_POINT('Ctrl Pts',(-50.,6.59177764993375,-8.2299772134607));
#54517=CARTESIAN_POINT('Ctrl Pts',(-21.,6.59177764993375,-8.2299772134607));
#54518=CARTESIAN_POINT('Ctrl Pts',(-50.,6.52223351516926,-8.21423196280605));
#54519=CARTESIAN_POINT('Ctrl Pts',(-21.,6.52223351516926,-8.21423196280605));
#54520=CARTESIAN_POINT('Ctrl Pts',(-50.,6.43022589217209,-8.1921225513));
#54521=CARTESIAN_POINT('Ctrl Pts',(-21.,6.43022589217209,-8.1921225513));
#54522=CARTESIAN_POINT('Ctrl Pts',(-50.,6.31642365942377,-8.16261538830187));
#54523=CARTESIAN_POINT('Ctrl Pts',(-21.,6.31642365942377,-8.16261538830187));
#54524=CARTESIAN_POINT('Ctrl Pts',(-50.,6.20385140809547,-8.1312203551374));
#54525=CARTESIAN_POINT('Ctrl Pts',(-21.,6.20385140809547,-8.1312203551374));
#54526=CARTESIAN_POINT('Ctrl Pts',(-50.,6.09254749437728,-8.0979137913074));
#54527=CARTESIAN_POINT('Ctrl Pts',(-21.,6.09254749437728,-8.0979137913074));
#54528=CARTESIAN_POINT('Ctrl Pts',(-50.,5.9825687506924,-8.06266677783295));
#54529=CARTESIAN_POINT('Ctrl Pts',(-21.,5.9825687506924,-8.06266677783295));
#54530=CARTESIAN_POINT('Ctrl Pts',(-50.,5.87399565540877,-8.02544535222689));
#54531=CARTESIAN_POINT('Ctrl Pts',(-21.,5.87399565540877,-8.02544535222689));
#54532=CARTESIAN_POINT('Ctrl Pts',(-50.,5.7669227832391,-7.98621594320599));
#54533=CARTESIAN_POINT('Ctrl Pts',(-21.,5.7669227832391,-7.98621594320599));
#54534=CARTESIAN_POINT('Ctrl Pts',(-50.,5.66144582368073,-7.94495188520329));
#54535=CARTESIAN_POINT('Ctrl Pts',(-21.,5.66144582368073,-7.94495188520329));
#54536=CARTESIAN_POINT('Ctrl Pts',(-50.,5.5576484178972,-7.90164067817667));
#54537=CARTESIAN_POINT('Ctrl Pts',(-21.,5.5576484178972,-7.90164067817667));
#54538=CARTESIAN_POINT('Ctrl Pts',(-50.,5.45559153104423,-7.85628931405591));
#54539=CARTESIAN_POINT('Ctrl Pts',(-21.,5.45559153104423,-7.85628931405591));
#54540=CARTESIAN_POINT('Ctrl Pts',(-50.,5.35529468870783,-7.80893560674388));
#54541=CARTESIAN_POINT('Ctrl Pts',(-21.,5.35529468870783,-7.80893560674388));
#54542=CARTESIAN_POINT('Ctrl Pts',(-50.,5.25675269887972,-7.75963419345371));
#54543=CARTESIAN_POINT('Ctrl Pts',(-21.,5.25675269887972,-7.75963419345371));
#54544=CARTESIAN_POINT('Ctrl Pts',(-50.,5.15997145275563,-7.70842918324715));
#54545=CARTESIAN_POINT('Ctrl Pts',(-21.,5.15997145275563,-7.70842918324715));
#54546=CARTESIAN_POINT('Ctrl Pts',(-50.,5.06499955030093,-7.65532943098672));
#54547=CARTESIAN_POINT('Ctrl Pts',(-21.,5.06499955030093,-7.65532943098672));
#54548=CARTESIAN_POINT('Ctrl Pts',(-50.,4.9719575030537,-7.60028648840776));
#54549=CARTESIAN_POINT('Ctrl Pts',(-21.,4.9719575030537,-7.60028648840776));
#54550=CARTESIAN_POINT('Ctrl Pts',(-50.,4.88107836846757,-7.54316218647348));
#54551=CARTESIAN_POINT('Ctrl Pts',(-21.,4.88107836846757,-7.54316218647348));
#54552=CARTESIAN_POINT('Ctrl Pts',(-50.,4.79269894740031,-7.48374039375355));
#54553=CARTESIAN_POINT('Ctrl Pts',(-21.,4.79269894740031,-7.48374039375355));
#54554=CARTESIAN_POINT('Ctrl Pts',(-50.,4.70721371156899,-7.42177134000892));
#54555=CARTESIAN_POINT('Ctrl Pts',(-21.,4.70721371156899,-7.42177134000892));
#54556=CARTESIAN_POINT('Ctrl Pts',(-50.,4.62503998887083,-7.35700721943171));
#54557=CARTESIAN_POINT('Ctrl Pts',(-21.,4.62503998887083,-7.35700721943171));
#54558=CARTESIAN_POINT('Ctrl Pts',(-50.,4.54657777868016,-7.28923990788708));
#54559=CARTESIAN_POINT('Ctrl Pts',(-21.,4.54657777868016,-7.28923990788708));
#54560=CARTESIAN_POINT('Ctrl Pts',(-50.,4.47217290162416,-7.21834255288981));
#54561=CARTESIAN_POINT('Ctrl Pts',(-21.,4.47217290162416,-7.21834255288981));
#54562=CARTESIAN_POINT('Ctrl Pts',(-50.,4.40207217433237,-7.14429034032177));
#54563=CARTESIAN_POINT('Ctrl Pts',(-21.,4.40207217433237,-7.14429034032177));
#54564=CARTESIAN_POINT('Ctrl Pts',(-50.,4.33637651734857,-7.06716577496009));
#54565=CARTESIAN_POINT('Ctrl Pts',(-21.,4.33637651734857,-7.06716577496009));
#54566=CARTESIAN_POINT('Ctrl Pts',(-50.,4.27498923356982,-6.98717136730191));
#54567=CARTESIAN_POINT('Ctrl Pts',(-21.,4.27498923356982,-6.98717136730191));
#54568=CARTESIAN_POINT('Ctrl Pts',(-50.,4.21757413484032,-6.90463617300865));
#54569=CARTESIAN_POINT('Ctrl Pts',(-21.,4.21757413484032,-6.90463617300865));
#54570=CARTESIAN_POINT('Ctrl Pts',(-50.,4.16348379256721,-6.82003644526658));
#54571=CARTESIAN_POINT('Ctrl Pts',(-21.,4.16348379256721,-6.82003644526658));
#54572=CARTESIAN_POINT('Ctrl Pts',(-50.,4.11183783259628,-6.73395053478792));
#54573=CARTESIAN_POINT('Ctrl Pts',(-21.,4.11183783259628,-6.73395053478792));
#54574=CARTESIAN_POINT('Ctrl Pts',(-50.,4.06165666819706,-6.64698999124062));
#54575=CARTESIAN_POINT('Ctrl Pts',(-21.,4.06165666819706,-6.64698999124062));
#54576=CARTESIAN_POINT('Ctrl Pts',(-50.,4.01197889710939,-6.55973735411151));
#54577=CARTESIAN_POINT('Ctrl Pts',(-21.,4.01197889710939,-6.55973735411151));
#54578=CARTESIAN_POINT('Ctrl Pts',(-50.,3.96197913233089,-6.47268455970493));
#54579=CARTESIAN_POINT('Ctrl Pts',(-21.,3.96197913233089,-6.47268455970493));
#54580=CARTESIAN_POINT('Ctrl Pts',(-50.,3.91110213900011,-6.38616193008433));
#54581=CARTESIAN_POINT('Ctrl Pts',(-21.,3.91110213900011,-6.38616193008433));
#54582=CARTESIAN_POINT('Ctrl Pts',(-50.,3.859023878729,-6.30036238594766));
#54583=CARTESIAN_POINT('Ctrl Pts',(-21.,3.859023878729,-6.30036238594766));
#54584=CARTESIAN_POINT('Ctrl Pts',(-50.,3.81627329006595,-6.23237673886416));
#54585=CARTESIAN_POINT('Ctrl Pts',(-21.,3.81627329006595,-6.23237673886416));
#54586=CARTESIAN_POINT('Ctrl Pts',(-50.,3.78357651403939,-6.1817683663582));
#54587=CARTESIAN_POINT('Ctrl Pts',(-21.,3.78357651403939,-6.1817683663582));
#54588=CARTESIAN_POINT('Ctrl Pts',(-50.,3.7614973065729,-6.1481985134482));
#54589=CARTESIAN_POINT('Ctrl Pts',(-21.,3.7614973065729,-6.1481985134482));
#54590=CARTESIAN_POINT('Ctrl Pts',(-50.,3.75038736519793,-6.13145585166881));
#54591=CARTESIAN_POINT('Ctrl Pts',(-21.,3.75038736519793,-6.13145585166881));
#54592=CARTESIAN_POINT('',(-50.,3.75038736519794,-6.13145585166881));
#54593=CARTESIAN_POINT('Origin',(-50.,0.,0.));
#54594=CARTESIAN_POINT('',(-50.,2.45543694297674,-6.75507110762463));
#54595=CARTESIAN_POINT('Ctrl Pts',(-50.,2.45543694297674,-6.75507110762463));
#54596=CARTESIAN_POINT('Ctrl Pts',(-21.,2.45543694297674,-6.75507110762463));
#54597=CARTESIAN_POINT('Ctrl Pts',(-50.,2.46297417772978,-6.77764561818537));
#54598=CARTESIAN_POINT('Ctrl Pts',(-21.,2.46297417772978,-6.77764561818537));
#54599=CARTESIAN_POINT('Ctrl Pts',(-50.,2.47820711493347,-6.82274841734025));
#54600=CARTESIAN_POINT('Ctrl Pts',(-21.,2.47820711493347,-6.82274841734025));
#54601=CARTESIAN_POINT('Ctrl Pts',(-50.,2.50153193679118,-6.89026394714059));
#54602=CARTESIAN_POINT('Ctrl Pts',(-21.,2.50153193679118,-6.89026394714059));
#54603=CARTESIAN_POINT('Ctrl Pts',(-50.,2.53358368474749,-6.98000697278327));
#54604=CARTESIAN_POINT('Ctrl Pts',(-21.,2.53358368474749,-6.98000697278327));
#54605=CARTESIAN_POINT('Ctrl Pts',(-50.,2.57514309471485,-7.09174914908801));
#54606=CARTESIAN_POINT('Ctrl Pts',(-21.,2.57514309471485,-7.09174914908801));
#54607=CARTESIAN_POINT('Ctrl Pts',(-50.,2.61790620462629,-7.20313763732345));
#54608=CARTESIAN_POINT('Ctrl Pts',(-21.,2.61790620462629,-7.20313763732345));
#54609=CARTESIAN_POINT('Ctrl Pts',(-50.,2.66128382072048,-7.31434056822034));
#54610=CARTESIAN_POINT('Ctrl Pts',(-21.,2.66128382072048,-7.31434056822034));
#54611=CARTESIAN_POINT('Ctrl Pts',(-50.,2.70427297026251,-7.42564364342468));
#54612=CARTESIAN_POINT('Ctrl Pts',(-21.,2.70427297026251,-7.42564364342468));
#54613=CARTESIAN_POINT('Ctrl Pts',(-50.,2.74553095355499,-7.53744508591865));
#54614=CARTESIAN_POINT('Ctrl Pts',(-21.,2.74553095355499,-7.53744508591865));
#54615=CARTESIAN_POINT('Ctrl Pts',(-50.,2.78345892001629,-7.65025207826714));
#54616=CARTESIAN_POINT('Ctrl Pts',(-21.,2.78345892001629,-7.65025207826714));
#54617=CARTESIAN_POINT('Ctrl Pts',(-50.,2.81629364412744,-7.76466852264525));
#54618=CARTESIAN_POINT('Ctrl Pts',(-21.,2.81629364412744,-7.76466852264525));
#54619=CARTESIAN_POINT('Ctrl Pts',(-50.,2.84216119689693,-7.88140953422486));
#54620=CARTESIAN_POINT('Ctrl Pts',(-21.,2.84216119689693,-7.88140953422486));
#54621=CARTESIAN_POINT('Ctrl Pts',(-50.,2.85947913898695,-8.00108902987832));
#54622=CARTESIAN_POINT('Ctrl Pts',(-21.,2.85947913898695,-8.00108902987832));
#54623=CARTESIAN_POINT('Ctrl Pts',(-50.,2.86748815125169,-8.12392974416385));
#54624=CARTESIAN_POINT('Ctrl Pts',(-21.,2.86748815125169,-8.12392974416385));
#54625=CARTESIAN_POINT('Ctrl Pts',(-50.,2.8666442371861,-8.24955186700095));
#54626=CARTESIAN_POINT('Ctrl Pts',(-21.,2.8666442371861,-8.24955186700095));
#54627=CARTESIAN_POINT('Ctrl Pts',(-50.,2.85932311928695,-8.37659160589212));
#54628=CARTESIAN_POINT('Ctrl Pts',(-21.,2.85932311928695,-8.37659160589212));
#54629=CARTESIAN_POINT('Ctrl Pts',(-50.,2.84893087833482,-8.50318672326558));
#54630=CARTESIAN_POINT('Ctrl Pts',(-21.,2.84893087833482,-8.50318672326558));
#54631=CARTESIAN_POINT('Ctrl Pts',(-50.,2.838231660712,-8.62789111098118));
#54632=CARTESIAN_POINT('Ctrl Pts',(-21.,2.838231660712,-8.62789111098118));
#54633=CARTESIAN_POINT('Ctrl Pts',(-50.,2.8281804649272,-8.7503085875302));
#54634=CARTESIAN_POINT('Ctrl Pts',(-21.,2.8281804649272,-8.7503085875302));
#54635=CARTESIAN_POINT('Ctrl Pts',(-50.,2.81593951016314,-8.87218721998315));
#54636=CARTESIAN_POINT('Ctrl Pts',(-21.,2.81593951016314,-8.87218721998315));
#54637=CARTESIAN_POINT('Ctrl Pts',(-50.,2.79564609540172,-8.99695638729624));
#54638=CARTESIAN_POINT('Ctrl Pts',(-21.,2.79564609540172,-8.99695638729624));
#54639=CARTESIAN_POINT('Ctrl Pts',(-50.,2.76185693608665,-9.12774569066013));
#54640=CARTESIAN_POINT('Ctrl Pts',(-21.,2.76185693608665,-9.12774569066013));
#54641=CARTESIAN_POINT('Ctrl Pts',(-50.,2.71205611361093,-9.26593773005304));
#54642=CARTESIAN_POINT('Ctrl Pts',(-21.,2.71205611361093,-9.26593773005304));
#54643=CARTESIAN_POINT('Ctrl Pts',(-50.,2.65001133311308,-9.40923210196585));
#54644=CARTESIAN_POINT('Ctrl Pts',(-21.,2.65001133311308,-9.40923210196585));
#54645=CARTESIAN_POINT('Ctrl Pts',(-50.,2.5873945538455,-9.5507160797281));
#54646=CARTESIAN_POINT('Ctrl Pts',(-21.,2.5873945538455,-9.5507160797281));
#54647=CARTESIAN_POINT('Ctrl Pts',(-50.,2.54042342638657,-9.68082891874335));
#54648=CARTESIAN_POINT('Ctrl Pts',(-21.,2.54042342638657,-9.68082891874335));
#54649=CARTESIAN_POINT('Ctrl Pts',(-50.,2.52733779392361,-9.78884102493588));
#54650=CARTESIAN_POINT('Ctrl Pts',(-21.,2.52733779392361,-9.78884102493588));
#54651=CARTESIAN_POINT('Ctrl Pts',(-50.,2.56562806487107,-9.86447715727042));
#54652=CARTESIAN_POINT('Ctrl Pts',(-21.,2.56562806487107,-9.86447715727042));
#54653=CARTESIAN_POINT('Ctrl Pts',(-50.,2.6691907234428,-9.89958344728561));
#54654=CARTESIAN_POINT('Ctrl Pts',(-21.,2.6691907234428,-9.89958344728561));
#54655=CARTESIAN_POINT('Ctrl Pts',(-50.,2.84860197903673,-9.88796382014256));
#54656=CARTESIAN_POINT('Ctrl Pts',(-21.,2.84860197903673,-9.88796382014256));
#54657=CARTESIAN_POINT('Ctrl Pts',(-50.,3.11165374758123,-9.82506278266417));
#54658=CARTESIAN_POINT('Ctrl Pts',(-21.,3.11165374758123,-9.82506278266417));
#54659=CARTESIAN_POINT('Ctrl Pts',(-50.,3.46376909107161,-9.70771911811945));
#54660=CARTESIAN_POINT('Ctrl Pts',(-21.,3.46376909107161,-9.70771911811945));
#54661=CARTESIAN_POINT('Ctrl Pts',(-50.,3.90844493048625,-9.5339037941241));
#54662=CARTESIAN_POINT('Ctrl Pts',(-21.,3.90844493048625,-9.5339037941241));
#54663=CARTESIAN_POINT('Ctrl Pts',(-50.,4.44766091491103,-9.30247791214345));
#54664=CARTESIAN_POINT('Ctrl Pts',(-21.,4.44766091491103,-9.30247791214345));
#54665=CARTESIAN_POINT('Ctrl Pts',(-50.,5.08228263794097,-9.01295415598311));
#54666=CARTESIAN_POINT('Ctrl Pts',(-21.,5.08228263794097,-9.01295415598311));
#54667=CARTESIAN_POINT('Ctrl Pts',(-50.,5.66641576644903,-8.73480497776003));
#54668=CARTESIAN_POINT('Ctrl Pts',(-21.,5.66641576644903,-8.73480497776003));
#54669=CARTESIAN_POINT('Ctrl Pts',(-50.,6.14741641494695,-8.50008023141016));
#54670=CARTESIAN_POINT('Ctrl Pts',(-21.,6.14741641494695,-8.50008023141016));
#54671=CARTESIAN_POINT('Ctrl Pts',(-50.,6.48712519233677,-8.33200677716551));
#54672=CARTESIAN_POINT('Ctrl Pts',(-21.,6.48712519233677,-8.33200677716551));
#54673=CARTESIAN_POINT('Ctrl Pts',(-50.,6.6617400018565,-8.24507247679879));
#54674=CARTESIAN_POINT('Ctrl Pts',(-21.,6.6617400018565,-8.24507247679879));
#54675=CARTESIAN_POINT('',(-21.5,2.55037217513312,-9.66931237308562));
#54676=CARTESIAN_POINT('Ctrl Pts',(-21.5,2.55037217513312,-9.66931237308562));
#54677=CARTESIAN_POINT('Ctrl Pts',(-21.4716714037525,2.55832628412868,-9.63791697607888));
#54678=CARTESIAN_POINT('Ctrl Pts',(-21.4424150110734,2.56959157653322,-9.60464841257241));
#54679=CARTESIAN_POINT('Ctrl Pts',(-21.2909879716435,2.63587850947584,-9.42991855559448));
#54680=CARTESIAN_POINT('Ctrl Pts',(-21.1630186724934,2.71837825362615,-9.27335939831189));
#54681=CARTESIAN_POINT('Ctrl Pts',(-21.,2.77045032493322,-9.08705700417233));
#54682=CARTESIAN_POINT('Ctrl Pts',(-50.,2.55037217513312,-9.66931237308562));
#54683=CARTESIAN_POINT('Ctrl Pts',(-45.1666666666667,2.55037217513312,-9.66931237308562));
#54684=CARTESIAN_POINT('Ctrl Pts',(-40.3333333333333,2.55037217513312,-9.66931237308562));
#54685=CARTESIAN_POINT('Ctrl Pts',(-30.8333333333333,2.55037217513312,-9.66931237308562));
#54686=CARTESIAN_POINT('Ctrl Pts',(-26.1666666666667,2.55037217513312,-9.66931237308562));
#54687=CARTESIAN_POINT('Ctrl Pts',(-21.5,2.55037217513312,-9.66931237308562));
#54688=CARTESIAN_POINT('Origin',(-21.25,0.,0.));
#54689=CARTESIAN_POINT('Origin',(-21.5,0.,0.));
#54690=CARTESIAN_POINT('Origin',(-35.75,0.,0.));
#54691=CARTESIAN_POINT('Ctrl Pts',(-50.,-0.718643267461624,-7.15148293042304));
#54692=CARTESIAN_POINT('Ctrl Pts',(-21.,-0.718643267461624,-7.15148293042304));
#54693=CARTESIAN_POINT('Ctrl Pts',(-50.,-0.721647166649912,-7.17509214524366));
#54694=CARTESIAN_POINT('Ctrl Pts',(-21.,-0.721647166649912,-7.17509214524366));
#54695=CARTESIAN_POINT('Ctrl Pts',(-50.,-0.72749213560466,-7.22233768688913));
#54696=CARTESIAN_POINT('Ctrl Pts',(-21.,-0.72749213560466,-7.22233768688913));
#54697=CARTESIAN_POINT('Ctrl Pts',(-50.,-0.735771087779772,-7.29328733826105));
#54698=CARTESIAN_POINT('Ctrl Pts',(-21.,-0.735771087779772,-7.29328733826105));
#54699=CARTESIAN_POINT('Ctrl Pts',(-50.,-0.745831500234844,-7.38804974272502));
#54700=CARTESIAN_POINT('Ctrl Pts',(-21.,-0.745831500234844,-7.38804974272502));
#54701=CARTESIAN_POINT('Ctrl Pts',(-50.,-0.756870878958097,-7.5067579169994));
#54702=CARTESIAN_POINT('Ctrl Pts',(-21.,-0.756870878958097,-7.5067579169994));
#54703=CARTESIAN_POINT('Ctrl Pts',(-50.,-0.766672302003446,-7.62566969516693));
#54704=CARTESIAN_POINT('Ctrl Pts',(-21.,-0.766672302003446,-7.62566969516693));
#54705=CARTESIAN_POINT('Ctrl Pts',(-50.,-0.775839563797133,-7.74468091618948));
#54706=CARTESIAN_POINT('Ctrl Pts',(-21.,-0.775839563797133,-7.74468091618948));
#54707=CARTESIAN_POINT('Ctrl Pts',(-50.,-0.785400272847099,-7.86361381479518));
#54708=CARTESIAN_POINT('Ctrl Pts',(-21.,-0.785400272847099,-7.86361381479518));
#54709=CARTESIAN_POINT('Ctrl Pts',(-50.,-0.796736942256156,-7.98224460192821));
#54710=CARTESIAN_POINT('Ctrl Pts',(-21.,-0.796736942256156,-7.98224460192821));
#54711=CARTESIAN_POINT('Ctrl Pts',(-50.,-0.811510144890449,-8.10033651802127));
#54712=CARTESIAN_POINT('Ctrl Pts',(-21.,-0.811510144890449,-8.10033651802127));
#54713=CARTESIAN_POINT('Ctrl Pts',(-50.,-0.831570515383447,-8.21766862525226));
#54714=CARTESIAN_POINT('Ctrl Pts',(-21.,-0.831570515383447,-8.21766862525226));
#54715=CARTESIAN_POINT('Ctrl Pts',(-50.,-0.858916682261846,-8.33407215281038));
#54716=CARTESIAN_POINT('Ctrl Pts',(-21.,-0.858916682261846,-8.33407215281038));
#54717=CARTESIAN_POINT('Ctrl Pts',(-50.,-0.895240742652424,-8.44941362598824));
#54718=CARTESIAN_POINT('Ctrl Pts',(-21.,-0.895240742652424,-8.44941362598824));
#54719=CARTESIAN_POINT('Ctrl Pts',(-50.,-0.941323460369318,-8.56356426545847));
#54720=CARTESIAN_POINT('Ctrl Pts',(-21.,-0.941323460369318,-8.56356426545847));
#54721=CARTESIAN_POINT('Ctrl Pts',(-50.,-0.996589197042053,-8.67637972666424));
#54722=CARTESIAN_POINT('Ctrl Pts',(-21.,-0.996589197042053,-8.67637972666424));
#54723=CARTESIAN_POINT('Ctrl Pts',(-50.,-1.05830577327405,-8.78766206238304));
#54724=CARTESIAN_POINT('Ctrl Pts',(-21.,-1.05830577327405,-8.78766206238304));
#54725=CARTESIAN_POINT('Ctrl Pts',(-50.,-1.12259642171968,-8.89721129760285));
#54726=CARTESIAN_POINT('Ctrl Pts',(-21.,-1.12259642171968,-8.89721129760285));
#54727=CARTESIAN_POINT('Ctrl Pts',(-50.,-1.18634328973517,-9.00492385207762));
#54728=CARTESIAN_POINT('Ctrl Pts',(-21.,-1.18634328973517,-9.00492385207762));
#54729=CARTESIAN_POINT('Ctrl Pts',(-50.,-1.24851405668088,-9.11085713692575));
#54730=CARTESIAN_POINT('Ctrl Pts',(-21.,-1.24851405668088,-9.11085713692575));
#54731=CARTESIAN_POINT('Ctrl Pts',(-50.,-1.31242393260393,-9.21535483920498));
#54732=CARTESIAN_POINT('Ctrl Pts',(-21.,-1.31242393260393,-9.21535483920498));
#54733=CARTESIAN_POINT('Ctrl Pts',(-50.,-1.38484298036779,-9.31896299195203));
#54734=CARTESIAN_POINT('Ctrl Pts',(-21.,-1.38484298036779,-9.31896299195203));
#54735=CARTESIAN_POINT('Ctrl Pts',(-50.,-1.47203331296336,-9.42213951575228));
#54736=CARTESIAN_POINT('Ctrl Pts',(-21.,-1.47203331296336,-9.42213951575228));
#54737=CARTESIAN_POINT('Ctrl Pts',(-50.,-1.576861582378,-9.52503847397034));
#54738=CARTESIAN_POINT('Ctrl Pts',(-21.,-1.576861582378,-9.52503847397034));
#54739=CARTESIAN_POINT('Ctrl Pts',(-50.,-1.69493509590243,-9.62722202065428));
#54740=CARTESIAN_POINT('Ctrl Pts',(-21.,-1.69493509590243,-9.62722202065428));
#54741=CARTESIAN_POINT('Ctrl Pts',(-50.,-1.81273846192755,-9.72752627760495));
#54742=CARTESIAN_POINT('Ctrl Pts',(-21.,-1.81273846192755,-9.72752627760495));
#54743=CARTESIAN_POINT('Ctrl Pts',(-50.,-1.91151183055746,-9.82437388645964));
#54744=CARTESIAN_POINT('Ctrl Pts',(-21.,-1.91151183055746,-9.82437388645964));
#54745=CARTESIAN_POINT('Ctrl Pts',(-50.,-1.97016627452818,-9.91601178835393));
#54746=CARTESIAN_POINT('Ctrl Pts',(-21.,-1.97016627452818,-9.91601178835393));
#54747=CARTESIAN_POINT('Ctrl Pts',(-50.,-1.96848522037067,-10.0007711148064));
#54748=CARTESIAN_POINT('Ctrl Pts',(-21.,-1.96848522037067,-10.0007711148064));
#54749=CARTESIAN_POINT('Ctrl Pts',(-50.,-1.89041053749867,-10.0773349427117));
#54750=CARTESIAN_POINT('Ctrl Pts',(-21.,-1.89041053749867,-10.0773349427117));
#54751=CARTESIAN_POINT('Ctrl Pts',(-50.,-1.72372501438528,-10.1447096468161));
#54752=CARTESIAN_POINT('Ctrl Pts',(-21.,-1.72372501438528,-10.1447096468161));
#54753=CARTESIAN_POINT('Ctrl Pts',(-50.,-1.45943182294451,-10.2021716552068));
#54754=CARTESIAN_POINT('Ctrl Pts',(-21.,-1.45943182294451,-10.2021716552068));
#54755=CARTESIAN_POINT('Ctrl Pts',(-50.,-1.09127335261449,-10.2492257884407));
#54756=CARTESIAN_POINT('Ctrl Pts',(-21.,-1.09127335261449,-10.2492257884407));
#54757=CARTESIAN_POINT('Ctrl Pts',(-50.,-0.615218622302492,-10.285561208657));
#54758=CARTESIAN_POINT('Ctrl Pts',(-21.,-0.615218622302492,-10.285561208657));
#54759=CARTESIAN_POINT('Ctrl Pts',(-50.,-0.0289898802580651,-10.3110107412798));
#54760=CARTESIAN_POINT('Ctrl Pts',(-21.,-0.0289898802580651,-10.3110107412798));
#54761=CARTESIAN_POINT('Ctrl Pts',(-50.,0.66840418497271,-10.3255108965746));
#54762=CARTESIAN_POINT('Ctrl Pts',(-21.,0.66840418497271,-10.3255108965746));
#54763=CARTESIAN_POINT('Ctrl Pts',(-50.,1.31537435394882,-10.3283530123025));
#54764=CARTESIAN_POINT('Ctrl Pts',(-21.,1.31537435394882,-10.3283530123025));
#54765=CARTESIAN_POINT('Ctrl Pts',(-50.,1.85058421429602,-10.3255716832032));
#54766=CARTESIAN_POINT('Ctrl Pts',(-21.,1.85058421429602,-10.3255716832032));
#54767=CARTESIAN_POINT('Ctrl Pts',(-50.,2.22957558565152,-10.3215368479529));
#54768=CARTESIAN_POINT('Ctrl Pts',(-21.,2.22957558565152,-10.3215368479529));
#54769=CARTESIAN_POINT('Ctrl Pts',(-50.,2.42461747220419,-10.3189742762293));
#54770=CARTESIAN_POINT('Ctrl Pts',(-21.,2.42461747220419,-10.3189742762293));
#54771=CARTESIAN_POINT('',(-21.5,-1.89755147577054,-9.81831443766195));
#54772=CARTESIAN_POINT('Ctrl Pts',(-50.,-1.89755147577054,-9.81831443766195));
#54773=CARTESIAN_POINT('Ctrl Pts',(-45.1666666666667,-1.89755147577054,
-9.81831443766195));
#54774=CARTESIAN_POINT('Ctrl Pts',(-40.3333333333333,-1.89755147577054,
-9.81831443766195));
#54775=CARTESIAN_POINT('Ctrl Pts',(-30.8333333333333,-1.89755147577054,
-9.81831443766195));
#54776=CARTESIAN_POINT('Ctrl Pts',(-26.1666666666667,-1.89755147577054,
-9.81831443766195));
#54777=CARTESIAN_POINT('Ctrl Pts',(-21.5,-1.89755147577054,-9.81831443766195));
#54778=CARTESIAN_POINT('',(-50.,-0.718643267461624,-7.15148293042304));
#54779=CARTESIAN_POINT('Ctrl Pts',(-21.5,-1.89755147577054,-9.81831443766195));
#54780=CARTESIAN_POINT('Ctrl Pts',(-21.4703246838902,-1.87577485631915,
-9.79229867840487));
#54781=CARTESIAN_POINT('Ctrl Pts',(-21.4396140182583,-1.84982079175854,
-9.7659920048413));
#54782=CARTESIAN_POINT('Ctrl Pts',(-21.2876118590989,-1.71298536185018,
-9.63694998390254));
#54783=CARTESIAN_POINT('Ctrl Pts',(-21.1610241576493,-1.57282267908268,
-9.53269100720236));
#54784=CARTESIAN_POINT('Ctrl Pts',(-21.,-1.44663677770971,-9.38920880763537));
#54785=CARTESIAN_POINT('Origin',(-50.,0.,0.));
#54786=CARTESIAN_POINT('',(-50.,0.718643267461627,-7.15148293042304));
#54787=CARTESIAN_POINT('Ctrl Pts',(-50.,2.42461747220419,-10.3189742762293));
#54788=CARTESIAN_POINT('Ctrl Pts',(-21.,2.42461747220419,-10.3189742762293));
#54789=CARTESIAN_POINT('Ctrl Pts',(-50.,2.40572662366171,-10.3043608046855));
#54790=CARTESIAN_POINT('Ctrl Pts',(-21.,2.40572662366171,-10.3043608046855));
#54791=CARTESIAN_POINT('Ctrl Pts',(-50.,2.36813316049665,-10.2750183870592));
#54792=CARTESIAN_POINT('Ctrl Pts',(-21.,2.36813316049665,-10.2750183870592));
#54793=CARTESIAN_POINT('Ctrl Pts',(-50.,2.31230766835601,-10.2306583371767));
#54794=CARTESIAN_POINT('Ctrl Pts',(-21.,2.31230766835601,-10.2306583371767));
#54795=CARTESIAN_POINT('Ctrl Pts',(-50.,2.2390045785598,-10.1708178342288));
#54796=CARTESIAN_POINT('Ctrl Pts',(-21.,2.2390045785598,-10.1708178342288));
#54797=CARTESIAN_POINT('Ctrl Pts',(-50.,2.14927498796815,-10.0948558607226));
#54798=CARTESIAN_POINT('Ctrl Pts',(-21.,2.14927498796815,-10.0948558607226));
#54799=CARTESIAN_POINT('Ctrl Pts',(-50.,2.06147268851079,-10.0177266439074));
#54800=CARTESIAN_POINT('Ctrl Pts',(-21.,2.06147268851079,-10.0177266439074));
#54801=CARTESIAN_POINT('Ctrl Pts',(-50.,1.97564250382672,-9.93942550853734));
#54802=CARTESIAN_POINT('Ctrl Pts',(-21.,1.97564250382672,-9.93942550853734));
#54803=CARTESIAN_POINT('Ctrl Pts',(-50.,1.89184818563464,-9.85995105817688));
#54804=CARTESIAN_POINT('Ctrl Pts',(-21.,1.89184818563464,-9.85995105817688));
#54805=CARTESIAN_POINT('Ctrl Pts',(-50.,1.81017697820953,-9.77930761193764));
#54806=CARTESIAN_POINT('Ctrl Pts',(-21.,1.81017697820953,-9.77930761193764));
#54807=CARTESIAN_POINT('Ctrl Pts',(-50.,1.73072865645713,-9.69750595756857));
#54808=CARTESIAN_POINT('Ctrl Pts',(-21.,1.73072865645713,-9.69750595756857));
#54809=CARTESIAN_POINT('Ctrl Pts',(-50.,1.65360100339141,-9.61456358834088));
#54810=CARTESIAN_POINT('Ctrl Pts',(-21.,1.65360100339141,-9.61456358834088));
#54811=CARTESIAN_POINT('Ctrl Pts',(-50.,1.57887480066182,-9.53050553264656));
#54812=CARTESIAN_POINT('Ctrl Pts',(-21.,1.57887480066182,-9.53050553264656));
#54813=CARTESIAN_POINT('Ctrl Pts',(-50.,1.50660194229105,-9.44536454178638));
#54814=CARTESIAN_POINT('Ctrl Pts',(-21.,1.50660194229105,-9.44536454178638));
#54815=CARTESIAN_POINT('Ctrl Pts',(-50.,1.43678361338666,-9.35918315674388));
#54816=CARTESIAN_POINT('Ctrl Pts',(-21.,1.43678361338666,-9.35918315674388));
#54817=CARTESIAN_POINT('Ctrl Pts',(-50.,1.3693914299125,-9.27200835121914));
#54818=CARTESIAN_POINT('Ctrl Pts',(-21.,1.3693914299125,-9.27200835121914));
#54819=CARTESIAN_POINT('Ctrl Pts',(-50.,1.30441156144786,-9.18388242219763));
#54820=CARTESIAN_POINT('Ctrl Pts',(-21.,1.30441156144786,-9.18388242219763));
#54821=CARTESIAN_POINT('Ctrl Pts',(-50.,1.24188395306769,-9.09483443436949));
#54822=CARTESIAN_POINT('Ctrl Pts',(-21.,1.24188395306769,-9.09483443436949));
#54823=CARTESIAN_POINT('Ctrl Pts',(-50.,1.18193820283021,-9.00487302535333));
#54824=CARTESIAN_POINT('Ctrl Pts',(-21.,1.18193820283021,-9.00487302535333));
#54825=CARTESIAN_POINT('Ctrl Pts',(-50.,1.12484423754393,-8.91397482898789));
#54826=CARTESIAN_POINT('Ctrl Pts',(-21.,1.12484423754393,-8.91397482898789));
#54827=CARTESIAN_POINT('Ctrl Pts',(-50.,1.07099928020948,-8.82209124999857));
#54828=CARTESIAN_POINT('Ctrl Pts',(-21.,1.07099928020948,-8.82209124999857));
#54829=CARTESIAN_POINT('Ctrl Pts',(-50.,1.02086710880845,-8.72916840803945));
#54830=CARTESIAN_POINT('Ctrl Pts',(-21.,1.02086710880845,-8.72916840803945));
#54831=CARTESIAN_POINT('Ctrl Pts',(-50.,0.974931241694465,-8.63516410958082));
#54832=CARTESIAN_POINT('Ctrl Pts',(-21.,0.974931241694465,-8.63516410958082));
#54833=CARTESIAN_POINT('Ctrl Pts',(-50.,0.933642367528787,-8.5400643944807));
#54834=CARTESIAN_POINT('Ctrl Pts',(-21.,0.933642367528787,-8.5400643944807));
#54835=CARTESIAN_POINT('Ctrl Pts',(-50.,0.897367099160984,-8.4439050185459));
#54836=CARTESIAN_POINT('Ctrl Pts',(-21.,0.897367099160984,-8.4439050185459));
#54837=CARTESIAN_POINT('Ctrl Pts',(-50.,0.866338577132719,-8.34677071475058));
#54838=CARTESIAN_POINT('Ctrl Pts',(-21.,0.866338577132719,-8.34677071475058));
#54839=CARTESIAN_POINT('Ctrl Pts',(-50.,0.840611930230857,-8.24877960511329));
#54840=CARTESIAN_POINT('Ctrl Pts',(-21.,0.840611930230857,-8.24877960511329));
#54841=CARTESIAN_POINT('Ctrl Pts',(-50.,0.820012171364339,-8.15007218998677));
#54842=CARTESIAN_POINT('Ctrl Pts',(-21.,0.820012171364339,-8.15007218998677));
#54843=CARTESIAN_POINT('Ctrl Pts',(-50.,0.804093633570272,-8.05079907170372));
#54844=CARTESIAN_POINT('Ctrl Pts',(-21.,0.804093633570272,-8.05079907170372));
#54845=CARTESIAN_POINT('Ctrl Pts',(-50.,0.792066365329068,-7.95110843081948));
#54846=CARTESIAN_POINT('Ctrl Pts',(-21.,0.792066365329068,-7.95110843081948));
#54847=CARTESIAN_POINT('Ctrl Pts',(-50.,0.782886239966143,-7.85113936329068));
#54848=CARTESIAN_POINT('Ctrl Pts',(-21.,0.782886239966143,-7.85113936329068));
#54849=CARTESIAN_POINT('Ctrl Pts',(-50.,0.775405338877349,-7.75101782957587));
#54850=CARTESIAN_POINT('Ctrl Pts',(-21.,0.775405338877349,-7.75101782957587));
#54851=CARTESIAN_POINT('Ctrl Pts',(-50.,0.768504714146026,-7.65085154280962));
#54852=CARTESIAN_POINT('Ctrl Pts',(-21.,0.768504714146026,-7.65085154280962));
#54853=CARTESIAN_POINT('Ctrl Pts',(-50.,0.761227274615911,-7.55072560028829));
#54854=CARTESIAN_POINT('Ctrl Pts',(-21.,0.761227274615911,-7.55072560028829));
#54855=CARTESIAN_POINT('Ctrl Pts',(-50.,0.752929449590465,-7.45069670452966));
#54856=CARTESIAN_POINT('Ctrl Pts',(-21.,0.752929449590465,-7.45069670452966));
#54857=CARTESIAN_POINT('Ctrl Pts',(-50.,0.743235585416283,-7.35079807608913));
#54858=CARTESIAN_POINT('Ctrl Pts',(-21.,0.743235585416283,-7.35079807608913));
#54859=CARTESIAN_POINT('Ctrl Pts',(-50.,0.734216502709278,-7.2709963393441));
#54860=CARTESIAN_POINT('Ctrl Pts',(-21.,0.734216502709278,-7.2709963393441));
#54861=CARTESIAN_POINT('Ctrl Pts',(-50.,0.72671587532212,-7.21121317182152));
#54862=CARTESIAN_POINT('Ctrl Pts',(-21.,0.72671587532212,-7.21121317182152));
#54863=CARTESIAN_POINT('Ctrl Pts',(-50.,0.721388610069064,-7.17138797035723));
#54864=CARTESIAN_POINT('Ctrl Pts',(-21.,0.721388610069064,-7.17138797035723));
#54865=CARTESIAN_POINT('Ctrl Pts',(-50.,0.718643267461621,-7.15148293042304));
#54866=CARTESIAN_POINT('Ctrl Pts',(-21.,0.718643267461621,-7.15148293042304));
#54867=CARTESIAN_POINT('',(-21.5,1.85780428234483,-9.82591284555797));
#54868=CARTESIAN_POINT('Ctrl Pts',(-21.5,1.85780428234483,-9.82591284555798));
#54869=CARTESIAN_POINT('Ctrl Pts',(-26.3333333333333,1.85780428234483,-9.82591284555798));
#54870=CARTESIAN_POINT('Ctrl Pts',(-31.1666666666667,1.85780428234483,-9.82591284555798));
#54871=CARTESIAN_POINT('Ctrl Pts',(-40.6666666666667,1.85780428234483,-9.82591284555798));
#54872=CARTESIAN_POINT('Ctrl Pts',(-45.3333333333333,1.85780428234483,-9.82591284555797));
#54873=CARTESIAN_POINT('Ctrl Pts',(-50.,1.85780428234483,-9.82591284555797));
#54874=CARTESIAN_POINT('Ctrl Pts',(-21.,1.45989994714919,-9.38715570044056));
#54875=CARTESIAN_POINT('Ctrl Pts',(-21.1708653764911,1.58343885080728,-9.54086217807748));
#54876=CARTESIAN_POINT('Ctrl Pts',(-21.337240031188,1.71664935045884,-9.68695766931646));
#54877=CARTESIAN_POINT('Ctrl Pts',(-21.5,1.85780428234483,-9.82591284555797));
#54878=CARTESIAN_POINT('Origin',(-35.75,0.,0.));
#54879=CARTESIAN_POINT('',(-21.5,-2.58947998462545,-9.65891264114259));
#54880=CARTESIAN_POINT('Origin',(-21.5,0.,0.));
#54881=CARTESIAN_POINT('Ctrl Pts',(-21.5,-2.58947998462545,-9.65891264114259));
#54882=CARTESIAN_POINT('Ctrl Pts',(-26.3333333333333,-2.58947998462545,
-9.65891264114259));
#54883=CARTESIAN_POINT('Ctrl Pts',(-31.1666666666667,-2.58947998462545,
-9.65891264114259));
#54884=CARTESIAN_POINT('Ctrl Pts',(-40.6666666666667,-2.58947998462545,
-9.65891264114259));
#54885=CARTESIAN_POINT('Ctrl Pts',(-45.3333333333333,-2.58947998462546,
-9.65891264114259));
#54886=CARTESIAN_POINT('Ctrl Pts',(-50.,-2.58947998462546,-9.65891264114259));
#54887=CARTESIAN_POINT('Origin',(-21.25,0.,0.));
#54888=CARTESIAN_POINT('Ctrl Pts',(-21.,-2.75760981235205,-9.09096189205628));
#54889=CARTESIAN_POINT('Ctrl Pts',(-21.0595504621632,-2.74206083288706,
-9.15790831820147));
#54890=CARTESIAN_POINT('Ctrl Pts',(-21.1201969196014,-2.72465875026456,
-9.22637318364334));
#54891=CARTESIAN_POINT('Ctrl Pts',(-21.1820623827142,-2.70512289983328,
-9.29649306846902));
#54892=CARTESIAN_POINT('Ctrl Pts',(-21.2426667634842,-2.68598527346419,
-9.36518361058578));
#54893=CARTESIAN_POINT('Ctrl Pts',(-21.304440959365,-2.66479906737499,-9.43546228599664));
#54894=CARTESIAN_POINT('Ctrl Pts',(-21.3675006106217,-2.64134946113942,
-9.50742323598161));
#54895=CARTESIAN_POINT('Ctrl Pts',(-21.4110415416836,-2.62515816181912,
-9.55711026564319));
#54896=CARTESIAN_POINT('Ctrl Pts',(-21.4551953158428,-2.60788916583244,
-9.60759844440427));
#54897=CARTESIAN_POINT('Ctrl Pts',(-21.5,-2.58947998461739,-9.65891264116508));
#54898=CARTESIAN_POINT('Ctrl Pts',(-50.,-2.29273028380004,-10.3490766663382));
#54899=CARTESIAN_POINT('Ctrl Pts',(-21.,-2.29273028380004,-10.3490766663382));
#54900=CARTESIAN_POINT('Ctrl Pts',(-50.,-2.30340980255016,-10.3277139514246));
#54901=CARTESIAN_POINT('Ctrl Pts',(-21.,-2.30340980255016,-10.3277139514246));
#54902=CARTESIAN_POINT('Ctrl Pts',(-50.,-2.32454914462407,-10.2849661542698));
#54903=CARTESIAN_POINT('Ctrl Pts',(-21.,-2.32454914462407,-10.2849661542698));
#54904=CARTESIAN_POINT('Ctrl Pts',(-50.,-2.35559907076766,-10.2207773570791));
#54905=CARTESIAN_POINT('Ctrl Pts',(-21.,-2.35559907076766,-10.2207773570791));
#54906=CARTESIAN_POINT('Ctrl Pts',(-50.,-2.39567905142538,-10.1350579081937));
#54907=CARTESIAN_POINT('Ctrl Pts',(-21.,-2.39567905142538,-10.1350579081937));
#54908=CARTESIAN_POINT('Ctrl Pts',(-50.,-2.44356395398247,-10.0276863246448));
#54909=CARTESIAN_POINT('Ctrl Pts',(-21.,-2.44356395398247,-10.0276863246448));
#54910=CARTESIAN_POINT('Ctrl Pts',(-50.,-2.48920597933682,-9.92009931149697));
#54911=CARTESIAN_POINT('Ctrl Pts',(-21.,-2.48920597933682,-9.92009931149697));
#54912=CARTESIAN_POINT('Ctrl Pts',(-50.,-2.53256271427195,-9.81231210474723));
#54913=CARTESIAN_POINT('Ctrl Pts',(-21.,-2.53256271427195,-9.81231210474723));
#54914=CARTESIAN_POINT('Ctrl Pts',(-50.,-2.57357611458342,-9.70435110708481));
#54915=CARTESIAN_POINT('Ctrl Pts',(-21.,-2.57357611458342,-9.70435110708481));
#54916=CARTESIAN_POINT('Ctrl Pts',(-50.,-2.61216944988784,-9.59625806376704));
#54917=CARTESIAN_POINT('Ctrl Pts',(-21.,-2.61216944988784,-9.59625806376704));
#54918=CARTESIAN_POINT('Ctrl Pts',(-50.,-2.6482575067302,-9.48808598492904));
#54919=CARTESIAN_POINT('Ctrl Pts',(-21.,-2.6482575067302,-9.48808598492904));
#54920=CARTESIAN_POINT('Ctrl Pts',(-50.,-2.68175977570501,-9.37989305792331));
#54921=CARTESIAN_POINT('Ctrl Pts',(-21.,-2.68175977570501,-9.37989305792331));
#54922=CARTESIAN_POINT('Ctrl Pts',(-50.,-2.71261433447333,-9.27173688239595));
#54923=CARTESIAN_POINT('Ctrl Pts',(-21.,-2.71261433447333,-9.27173688239595));
#54924=CARTESIAN_POINT('Ctrl Pts',(-50.,-2.74078863839312,-9.16366948222194));
#54925=CARTESIAN_POINT('Ctrl Pts',(-21.,-2.74078863839312,-9.16366948222194));
#54926=CARTESIAN_POINT('Ctrl Pts',(-50.,-2.76630007756038,-9.05572969970196));
#54927=CARTESIAN_POINT('Ctrl Pts',(-21.,-2.76630007756038,-9.05572969970196));
#54928=CARTESIAN_POINT('Ctrl Pts',(-50.,-2.78919460623265,-8.94794754130566));
#54929=CARTESIAN_POINT('Ctrl Pts',(-21.,-2.78919460623265,-8.94794754130566));
#54930=CARTESIAN_POINT('Ctrl Pts',(-50.,-2.80950303716262,-8.84035511450549));
#54931=CARTESIAN_POINT('Ctrl Pts',(-21.,-2.80950303716262,-8.84035511450549));
#54932=CARTESIAN_POINT('Ctrl Pts',(-50.,-2.82720199177778,-8.73299593720093));
#54933=CARTESIAN_POINT('Ctrl Pts',(-21.,-2.82720199177778,-8.73299593720093));
#54934=CARTESIAN_POINT('Ctrl Pts',(-50.,-2.84217845398458,-8.62593402210748));
#54935=CARTESIAN_POINT('Ctrl Pts',(-21.,-2.84217845398458,-8.62593402210748));
#54936=CARTESIAN_POINT('Ctrl Pts',(-50.,-2.85417908993455,-8.51926543389428));
#54937=CARTESIAN_POINT('Ctrl Pts',(-21.,-2.85417908993455,-8.51926543389428));
#54938=CARTESIAN_POINT('Ctrl Pts',(-50.,-2.86282492937103,-8.41311873833255));
#54939=CARTESIAN_POINT('Ctrl Pts',(-21.,-2.86282492937103,-8.41311873833255));
#54940=CARTESIAN_POINT('Ctrl Pts',(-50.,-2.86767474496505,-8.30764661663281));
#54941=CARTESIAN_POINT('Ctrl Pts',(-21.,-2.86767474496505,-8.30764661663281));
#54942=CARTESIAN_POINT('Ctrl Pts',(-50.,-2.8682745946465,-8.20302084448955));
#54943=CARTESIAN_POINT('Ctrl Pts',(-21.,-2.8682745946465,-8.20302084448955));
#54944=CARTESIAN_POINT('Ctrl Pts',(-50.,-2.86421236488387,-8.099424390731));
#54945=CARTESIAN_POINT('Ctrl Pts',(-21.,-2.86421236488387,-8.099424390731));
#54946=CARTESIAN_POINT('Ctrl Pts',(-50.,-2.85517326277626,-7.9970485375799));
#54947=CARTESIAN_POINT('Ctrl Pts',(-21.,-2.85517326277626,-7.9970485375799));
#54948=CARTESIAN_POINT('Ctrl Pts',(-50.,-2.84098400021346,-7.89607078269802));
#54949=CARTESIAN_POINT('Ctrl Pts',(-21.,-2.84098400021346,-7.89607078269802));
#54950=CARTESIAN_POINT('Ctrl Pts',(-50.,-2.82164615909785,-7.79662146983088));
#54951=CARTESIAN_POINT('Ctrl Pts',(-21.,-2.82164615909785,-7.79662146983088));
#54952=CARTESIAN_POINT('Ctrl Pts',(-50.,-2.79737835816915,-7.69875126136884));
#54953=CARTESIAN_POINT('Ctrl Pts',(-21.,-2.79737835816915,-7.69875126136884));
#54954=CARTESIAN_POINT('Ctrl Pts',(-50.,-2.76864747338962,-7.60240247767684));
#54955=CARTESIAN_POINT('Ctrl Pts',(-21.,-2.76864747338962,-7.60240247767684));
#54956=CARTESIAN_POINT('Ctrl Pts',(-50.,-2.73622951961898,-7.50736587770304));
#54957=CARTESIAN_POINT('Ctrl Pts',(-21.,-2.73622951961898,-7.50736587770304));
#54958=CARTESIAN_POINT('Ctrl Pts',(-50.,-2.70112557395893,-7.41331375298832));
#54959=CARTESIAN_POINT('Ctrl Pts',(-21.,-2.70112557395893,-7.41331375298832));
#54960=CARTESIAN_POINT('Ctrl Pts',(-50.,-2.66442452752942,-7.31986152676826));
#54961=CARTESIAN_POINT('Ctrl Pts',(-21.,-2.66442452752942,-7.31986152676826));
#54962=CARTESIAN_POINT('Ctrl Pts',(-50.,-2.62718125254576,-7.22662075191781));
#54963=CARTESIAN_POINT('Ctrl Pts',(-21.,-2.62718125254576,-7.22662075191781));
#54964=CARTESIAN_POINT('Ctrl Pts',(-50.,-2.59029498067661,-7.13325283216217));
#54965=CARTESIAN_POINT('Ctrl Pts',(-21.,-2.59029498067661,-7.13325283216217));
#54966=CARTESIAN_POINT('Ctrl Pts',(-50.,-2.55437015138428,-7.03952961984441));
#54967=CARTESIAN_POINT('Ctrl Pts',(-21.,-2.55437015138428,-7.03952961984441));
#54968=CARTESIAN_POINT('Ctrl Pts',(-50.,-2.5197596307744,-6.94531805563895));
#54969=CARTESIAN_POINT('Ctrl Pts',(-21.,-2.5197596307744,-6.94531805563895));
#54970=CARTESIAN_POINT('Ctrl Pts',(-50.,-2.49326086758344,-6.8695059418988));
#54971=CARTESIAN_POINT('Ctrl Pts',(-21.,-2.49326086758344,-6.8695059418988));
#54972=CARTESIAN_POINT('Ctrl Pts',(-50.,-2.47407975508802,-6.8123887688799));
#54973=CARTESIAN_POINT('Ctrl Pts',(-21.,-2.47407975508802,-6.8123887688799));
#54974=CARTESIAN_POINT('Ctrl Pts',(-50.,-2.46159994790965,-6.77419608843536));
#54975=CARTESIAN_POINT('Ctrl Pts',(-21.,-2.46159994790965,-6.77419608843536));
#54976=CARTESIAN_POINT('Ctrl Pts',(-50.,-2.45543694297675,-6.75507110762463));
#54977=CARTESIAN_POINT('Ctrl Pts',(-21.,-2.45543694297675,-6.75507110762463));
#54978=CARTESIAN_POINT('',(-50.,-2.45543694297674,-6.75507110762463));
#54979=CARTESIAN_POINT('Origin',(-50.,0.,0.));
#54980=CARTESIAN_POINT('',(-50.,-3.75038736519793,-6.13145585166881));
#54981=CARTESIAN_POINT('Ctrl Pts',(-50.,-3.75038736519793,-6.13145585166881));
#54982=CARTESIAN_POINT('Ctrl Pts',(-21.,-3.75038736519793,-6.13145585166881));
#54983=CARTESIAN_POINT('Ctrl Pts',(-50.,-3.7633374392529,-6.15142367620606));
#54984=CARTESIAN_POINT('Ctrl Pts',(-21.,-3.7633374392529,-6.15142367620606));
#54985=CARTESIAN_POINT('Ctrl Pts',(-50.,-3.78910264658076,-6.19145440139071));
#54986=CARTESIAN_POINT('Ctrl Pts',(-21.,-3.78910264658076,-6.19145440139071));
#54987=CARTESIAN_POINT('Ctrl Pts',(-50.,-3.82734562477572,-6.25178572573963));
#54988=CARTESIAN_POINT('Ctrl Pts',(-21.,-3.82734562477572,-6.25178572573963));
#54989=CARTESIAN_POINT('Ctrl Pts',(-50.,-3.87752560957259,-6.33279865263617));
#54990=CARTESIAN_POINT('Ctrl Pts',(-21.,-3.87752560957259,-6.33279865263617));
#54991=CARTESIAN_POINT('Ctrl Pts',(-50.,-3.93897729264122,-6.43496121510494));
#54992=CARTESIAN_POINT('Ctrl Pts',(-21.,-3.93897729264122,-6.43496121510494));
#54993=CARTESIAN_POINT('Ctrl Pts',(-50.,-3.99940195660266,-6.53784434718121));
#54994=CARTESIAN_POINT('Ctrl Pts',(-21.,-3.99940195660266,-6.53784434718121));
#54995=CARTESIAN_POINT('Ctrl Pts',(-50.,-4.0592984076569,-6.64109222642907));
#54996=CARTESIAN_POINT('Ctrl Pts',(-21.,-4.0592984076569,-6.64109222642907));
#54997=CARTESIAN_POINT('Ctrl Pts',(-50.,-4.11951535961712,-6.74409882925098));
#54998=CARTESIAN_POINT('Ctrl Pts',(-21.,-4.11951535961712,-6.74409882925098));
#54999=CARTESIAN_POINT('Ctrl Pts',(-50.,-4.18120131531612,-6.84606267872027));
#55000=CARTESIAN_POINT('Ctrl Pts',(-21.,-4.18120131531612,-6.84606267872027));
#55001=CARTESIAN_POINT('Ctrl Pts',(-50.,-4.24574967308285,-6.94604996627335));
#55002=CARTESIAN_POINT('Ctrl Pts',(-21.,-4.24574967308285,-6.94604996627335));
#55003=CARTESIAN_POINT('Ctrl Pts',(-50.,-4.31473193577955,-7.04305867353628));
#55004=CARTESIAN_POINT('Ctrl Pts',(-21.,-4.31473193577955,-7.04305867353628));
#55005=CARTESIAN_POINT('Ctrl Pts',(-50.,-4.38987557857684,-7.13606957084443));
#55006=CARTESIAN_POINT('Ctrl Pts',(-21.,-4.38987557857684,-7.13606957084443));
#55007=CARTESIAN_POINT('Ctrl Pts',(-50.,-4.4726472158023,-7.22422822821349));
#55008=CARTESIAN_POINT('Ctrl Pts',(-21.,-4.4726472158023,-7.22422822821349));
#55009=CARTESIAN_POINT('Ctrl Pts',(-50.,-4.56369441608956,-7.30707985875561));
#55010=CARTESIAN_POINT('Ctrl Pts',(-21.,-4.56369441608956,-7.30707985875561));
#55011=CARTESIAN_POINT('Ctrl Pts',(-50.,-4.66243591843162,-7.38474417264741));
#55012=CARTESIAN_POINT('Ctrl Pts',(-21.,-4.66243591843162,-7.38474417264741));
#55013=CARTESIAN_POINT('Ctrl Pts',(-50.,-4.76632422816958,-7.45822827381644));
#55014=CARTESIAN_POINT('Ctrl Pts',(-21.,-4.76632422816958,-7.45822827381644));
#55015=CARTESIAN_POINT('Ctrl Pts',(-50.,-4.87177973271099,-7.52903405731413));
#55016=CARTESIAN_POINT('Ctrl Pts',(-21.,-4.87177973271099,-7.52903405731413));
#55017=CARTESIAN_POINT('Ctrl Pts',(-50.,-4.97594840210465,-7.59842098612654));
#55018=CARTESIAN_POINT('Ctrl Pts',(-21.,-4.97594840210465,-7.59842098612654));
#55019=CARTESIAN_POINT('Ctrl Pts',(-50.,-5.07792505734327,-7.66688869302314));
#55020=CARTESIAN_POINT('Ctrl Pts',(-21.,-5.07792505734327,-7.66688869302314));
#55021=CARTESIAN_POINT('Ctrl Pts',(-50.,-5.18084571969554,-7.73330841361203));
#55022=CARTESIAN_POINT('Ctrl Pts',(-21.,-5.18084571969554,-7.73330841361203));
#55023=CARTESIAN_POINT('Ctrl Pts',(-50.,-5.29104691989087,-7.79523468647088));
#55024=CARTESIAN_POINT('Ctrl Pts',(-21.,-5.29104691989087,-7.79523468647088));
#55025=CARTESIAN_POINT('Ctrl Pts',(-50.,-5.41436931107715,-7.85036305479183));
#55026=CARTESIAN_POINT('Ctrl Pts',(-21.,-5.41436931107715,-7.85036305479183));
#55027=CARTESIAN_POINT('Ctrl Pts',(-50.,-5.55346250303877,-7.89758853118704));
#55028=CARTESIAN_POINT('Ctrl Pts',(-21.,-5.55346250303877,-7.89758853118704));
#55029=CARTESIAN_POINT('Ctrl Pts',(-50.,-5.70417884215966,-7.9384225480224));
#55030=CARTESIAN_POINT('Ctrl Pts',(-21.,-5.70417884215966,-7.9384225480224));
#55031=CARTESIAN_POINT('Ctrl Pts',(-50.,-5.85383639353758,-7.97768059592143));
#55032=CARTESIAN_POINT('Ctrl Pts',(-21.,-5.85383639353758,-7.97768059592143));
#55033=CARTESIAN_POINT('Ctrl Pts',(-50.,-5.98484872630544,-8.02208111792391));
#55034=CARTESIAN_POINT('Ctrl Pts',(-21.,-5.98484872630544,-8.02208111792391));
#55035=CARTESIAN_POINT('Ctrl Pts',(-50.,-6.07745474980597,-8.07919480518469));
#55036=CARTESIAN_POINT('Ctrl Pts',(-21.,-6.07745474980597,-8.07919480518469));
#55037=CARTESIAN_POINT('Ctrl Pts',(-50.,-6.11271586583108,-8.15628970164627));
#55038=CARTESIAN_POINT('Ctrl Pts',(-21.,-6.11271586583108,-8.15628970164627));
#55039=CARTESIAN_POINT('Ctrl Pts',(-50.,-6.07559280712476,-8.2591466623313));
#55040=CARTESIAN_POINT('Ctrl Pts',(-21.,-6.07559280712476,-8.2591466623313));
#55041=CARTESIAN_POINT('Ctrl Pts',(-50.,-5.9546471286083,-8.39217131123866));
#55042=CARTESIAN_POINT('Ctrl Pts',(-21.,-5.9546471286083,-8.39217131123866));
#55043=CARTESIAN_POINT('Ctrl Pts',(-50.,-5.74145902217939,-8.55861531001153));
#55044=CARTESIAN_POINT('Ctrl Pts',(-21.,-5.74145902217939,-8.55861531001153));
#55045=CARTESIAN_POINT('Ctrl Pts',(-50.,-5.43017572522592,-8.76074759285599));
#55046=CARTESIAN_POINT('Ctrl Pts',(-21.,-5.43017572522592,-8.76074759285599));
#55047=CARTESIAN_POINT('Ctrl Pts',(-50.,-5.01703058178298,-9.00003708168539));
#55048=CARTESIAN_POINT('Ctrl Pts',(-21.,-5.01703058178298,-9.00003708168539));
#55049=CARTESIAN_POINT('Ctrl Pts',(-50.,-4.49989887410451,-9.27732143685757));
#55050=CARTESIAN_POINT('Ctrl Pts',(-21.,-4.49989887410451,-9.27732143685757));
#55051=CARTESIAN_POINT('Ctrl Pts',(-50.,-3.87785991426877,-9.59297357001867));
#55052=CARTESIAN_POINT('Ctrl Pts',(-21.,-3.87785991426877,-9.59297357001867));
#55053=CARTESIAN_POINT('Ctrl Pts',(-50.,-3.29619308135874,-9.87624406382134));
#55054=CARTESIAN_POINT('Ctrl Pts',(-21.,-3.29619308135874,-9.87624406382134));
#55055=CARTESIAN_POINT('Ctrl Pts',(-50.,-2.8127788859222,-10.1059570283115));
#55056=CARTESIAN_POINT('Ctrl Pts',(-21.,-2.8127788859222,-10.1059570283115));
#55057=CARTESIAN_POINT('Ctrl Pts',(-50.,-2.46956880972213,-10.2667599606609));
#55058=CARTESIAN_POINT('Ctrl Pts',(-21.,-2.46956880972213,-10.2667599606609));
#55059=CARTESIAN_POINT('Ctrl Pts',(-50.,-2.29273028380004,-10.3490766663382));
#55060=CARTESIAN_POINT('Ctrl Pts',(-21.,-2.29273028380004,-10.3490766663382));
#55061=CARTESIAN_POINT('',(-21.5,-5.96964178495622,-8.0226789141349));
#55062=CARTESIAN_POINT('Ctrl Pts',(-21.5,-5.96964178495622,-8.0226789141349));
#55063=CARTESIAN_POINT('Ctrl Pts',(-21.4716400099246,-5.94010387156942,
-8.0093081760176));
#55064=CARTESIAN_POINT('Ctrl Pts',(-21.4423497933807,-5.90702876507278,
-7.99736128679948));
#55065=CARTESIAN_POINT('Ctrl Pts',(-21.2909092331881,-5.72905875837931,
-7.9402495905054));
#55066=CARTESIAN_POINT('Ctrl Pts',(-21.1629721875807,-5.55527241504855,
-7.90713720025227));
#55067=CARTESIAN_POINT('Ctrl Pts',(-21.,-5.37719972469147,-7.83171265565699));
#55068=CARTESIAN_POINT('Ctrl Pts',(-50.,-5.96964178495622,-8.0226789141349));
#55069=CARTESIAN_POINT('Ctrl Pts',(-45.1666666666667,-5.96964178495622,
-8.0226789141349));
#55070=CARTESIAN_POINT('Ctrl Pts',(-40.3333333333333,-5.96964178495622,
-8.0226789141349));
#55071=CARTESIAN_POINT('Ctrl Pts',(-30.8333333333333,-5.96964178495622,
-8.0226789141349));
#55072=CARTESIAN_POINT('Ctrl Pts',(-26.1666666666667,-5.96964178495622,
-8.0226789141349));
#55073=CARTESIAN_POINT('Ctrl Pts',(-21.5,-5.96964178495622,-8.0226789141349));
#55074=CARTESIAN_POINT('Origin',(-21.25,0.,0.));
#55075=CARTESIAN_POINT('Origin',(-21.5,0.,0.));
#55076=CARTESIAN_POINT('Origin',(-35.75,0.,0.));
#55077=CARTESIAN_POINT('Ctrl Pts',(-50.,-6.03932124977421,-3.89701874412038));
#55078=CARTESIAN_POINT('Ctrl Pts',(-21.,-6.03932124977421,-3.89701874412038));
#55079=CARTESIAN_POINT('Ctrl Pts',(-50.,-6.05965257770704,-3.90939030583537));
#55080=CARTESIAN_POINT('Ctrl Pts',(-21.,-6.05965257770704,-3.90939030583537));
#55081=CARTESIAN_POINT('Ctrl Pts',(-50.,-6.10023490810719,-3.93427763849175));
#55082=CARTESIAN_POINT('Ctrl Pts',(-21.,-6.10023490810719,-3.93427763849175));
#55083=CARTESIAN_POINT('Ctrl Pts',(-50.,-6.16086742147115,-3.97204127711522));
#55084=CARTESIAN_POINT('Ctrl Pts',(-21.,-6.16086742147115,-3.97204127711522));
#55085=CARTESIAN_POINT('Ctrl Pts',(-50.,-6.24122821720367,-4.02325912271413));
#55086=CARTESIAN_POINT('Ctrl Pts',(-21.,-6.24122821720367,-4.02325912271413));
#55087=CARTESIAN_POINT('Ctrl Pts',(-50.,-6.34092094513049,-4.08864152493875));
#55088=CARTESIAN_POINT('Ctrl Pts',(-21.,-6.34092094513049,-4.08864152493875));
#55089=CARTESIAN_POINT('Ctrl Pts',(-50.,-6.44000100425059,-4.15511874483724));
#55090=CARTESIAN_POINT('Ctrl Pts',(-21.,-6.44000100425059,-4.15511874483724));
#55091=CARTESIAN_POINT('Ctrl Pts',(-50.,-6.53876341785232,-4.22215377357323));
#55092=CARTESIAN_POINT('Ctrl Pts',(-21.,-6.53876341785232,-4.22215377357323));
#55093=CARTESIAN_POINT('Ctrl Pts',(-50.,-6.63770990687462,-4.2888323596294));
#55094=CARTESIAN_POINT('Ctrl Pts',(-21.,-6.63770990687462,-4.2888323596294));
#55095=CARTESIAN_POINT('Ctrl Pts',(-50.,-6.73752748880879,-4.35393408054299));
#55096=CARTESIAN_POINT('Ctrl Pts',(-21.,-6.73752748880879,-4.35393408054299));
#55097=CARTESIAN_POINT('Ctrl Pts',(-50.,-6.83906640781858,-4.4160130309926));
#55098=CARTESIAN_POINT('Ctrl Pts',(-21.,-6.83906640781858,-4.4160130309926));
#55099=CARTESIAN_POINT('Ctrl Pts',(-50.,-6.94330777957998,-4.47348457408032));
#55100=CARTESIAN_POINT('Ctrl Pts',(-21.,-6.94330777957998,-4.47348457408032));
#55101=CARTESIAN_POINT('Ctrl Pts',(-50.,-7.05136577826386,-4.52468089222283));
#55102=CARTESIAN_POINT('Ctrl Pts',(-21.,-7.05136577826386,-4.52468089222283));
#55103=CARTESIAN_POINT('Ctrl Pts',(-50.,-7.16419105444418,-4.56819583049617));
#55104=CARTESIAN_POINT('Ctrl Pts',(-21.,-7.16419105444418,-4.56819583049617));
#55105=CARTESIAN_POINT('Ctrl Pts',(-50.,-7.28216972266428,-4.60333867057275));
#55106=CARTESIAN_POINT('Ctrl Pts',(-21.,-7.28216972266428,-4.60333867057275));
#55107=CARTESIAN_POINT('Ctrl Pts',(-50.,-7.40483002515176,-4.63046946729401));
#55108=CARTESIAN_POINT('Ctrl Pts',(-21.,-7.40483002515176,-4.63046946729401));
#55109=CARTESIAN_POINT('Ctrl Pts',(-50.,-7.53031371454558,-4.65160090645338));
#55110=CARTESIAN_POINT('Ctrl Pts',(-21.,-7.53031371454558,-4.65160090645338));
#55111=CARTESIAN_POINT('Ctrl Pts',(-50.,-7.65604731918147,-4.66963928443128));
#55112=CARTESIAN_POINT('Ctrl Pts',(-21.,-7.65604731918147,-4.66963928443128));
#55113=CARTESIAN_POINT('Ctrl Pts',(-50.,-7.78000590743498,-4.68695765535521));
#55114=CARTESIAN_POINT('Ctrl Pts',(-21.,-7.78000590743498,-4.68695765535521));
#55115=CARTESIAN_POINT('Ctrl Pts',(-50.,-7.9015907237349,-4.70439891524807));
#55116=CARTESIAN_POINT('Ctrl Pts',(-21.,-7.9015907237349,-4.70439891524807));
#55117=CARTESIAN_POINT('Ctrl Pts',(-50.,-8.02313747309844,-4.71958541389958));
#55118=CARTESIAN_POINT('Ctrl Pts',(-21.,-8.02313747309844,-4.71958541389958));
#55119=CARTESIAN_POINT('Ctrl Pts',(-50.,-8.14929412649754,-4.72756454905465));
#55120=CARTESIAN_POINT('Ctrl Pts',(-21.,-8.14929412649754,-4.72756454905465));
#55121=CARTESIAN_POINT('Ctrl Pts',(-50.,-8.2843230642502,-4.72372591244526));
#55122=CARTESIAN_POINT('Ctrl Pts',(-21.,-8.2843230642502,-4.72372591244526));
#55123=CARTESIAN_POINT('Ctrl Pts',(-50.,-8.43013206622476,-4.7059243222351));
#55124=CARTESIAN_POINT('Ctrl Pts',(-21.,-8.43013206622476,-4.7059243222351));
#55125=CARTESIAN_POINT('Ctrl Pts',(-50.,-8.58364001156461,-4.67732113139128));
#55126=CARTESIAN_POINT('Ctrl Pts',(-21.,-8.58364001156461,-4.67732113139128));
#55127=CARTESIAN_POINT('Ctrl Pts',(-50.,-8.73551023481551,-4.6477574323839));
#55128=CARTESIAN_POINT('Ctrl Pts',(-21.,-8.73551023481551,-4.6477574323839));
#55129=CARTESIAN_POINT('Ctrl Pts',(-50.,-8.87281293245584,-4.63091679961492));
#55130=CARTESIAN_POINT('Ctrl Pts',(-21.,-8.87281293245584,-4.63091679961492));
#55131=CARTESIAN_POINT('Ctrl Pts',(-50.,-8.98102877679355,-4.64219420602678));
#55132=CARTESIAN_POINT('Ctrl Pts',(-21.,-8.98102877679355,-4.64219420602678));
#55133=CARTESIAN_POINT('Ctrl Pts',(-50.,-9.04624816652329,-4.69635508274639));
#55134=CARTESIAN_POINT('Ctrl Pts',(-21.,-9.04624816652329,-4.69635508274639));
#55135=CARTESIAN_POINT('Ctrl Pts',(-50.,-9.05742940904388,-4.80513309368965));
#55136=CARTESIAN_POINT('Ctrl Pts',(-21.,-9.05742940904388,-4.80513309368965));
#55137=CARTESIAN_POINT('Ctrl Pts',(-50.,-9.00617835005594,-4.97746052424366));
#55138=CARTESIAN_POINT('Ctrl Pts',(-21.,-9.00617835005594,-4.97746052424366));
#55139=CARTESIAN_POINT('Ctrl Pts',(-50.,-8.88631984769767,-5.21992023813997));
#55140=CARTESIAN_POINT('Ctrl Pts',(-21.,-8.88631984769767,-5.21992023813997));
#55141=CARTESIAN_POINT('Ctrl Pts',(-50.,-8.6935651987215,-5.53709589298789));
#55142=CARTESIAN_POINT('Ctrl Pts',(-21.,-8.6935651987215,-5.53709589298789));
#55143=CARTESIAN_POINT('Ctrl Pts',(-50.,-8.42515810469916,-5.93194523247474));
#55144=CARTESIAN_POINT('Ctrl Pts',(-21.,-8.42515810469916,-5.93194523247474));
#55145=CARTESIAN_POINT('Ctrl Pts',(-50.,-8.07954770829655,-6.40614484298506));
#55146=CARTESIAN_POINT('Ctrl Pts',(-21.,-8.07954770829655,-6.40614484298506));
#55147=CARTESIAN_POINT('Ctrl Pts',(-50.,-7.65606629865851,-6.96043017782053));
#55148=CARTESIAN_POINT('Ctrl Pts',(-21.,-7.65606629865851,-6.96043017782053));
#55149=CARTESIAN_POINT('Ctrl Pts',(-50.,-7.25490905174796,-7.46802385431575));
#55150=CARTESIAN_POINT('Ctrl Pts',(-21.,-7.25490905174796,-7.46802385431575));
#55151=CARTESIAN_POINT('Ctrl Pts',(-50.,-6.91903663131433,-7.8847336425335));
#55152=CARTESIAN_POINT('Ctrl Pts',(-21.,-6.91903663131433,-7.8847336425335));
#55153=CARTESIAN_POINT('Ctrl Pts',(-50.,-6.67958481505646,-8.17852534961221));
#55154=CARTESIAN_POINT('Ctrl Pts',(-21.,-6.67958481505646,-8.17852534961221));
#55155=CARTESIAN_POINT('Ctrl Pts',(-50.,-6.55597468860601,-8.32941749958287));
#55156=CARTESIAN_POINT('Ctrl Pts',(-21.,-6.55597468860601,-8.32941749958287));
#55157=CARTESIAN_POINT('',(-21.5,-8.85937132577942,-4.63805343996351));
#55158=CARTESIAN_POINT('Ctrl Pts',(-50.,-8.85937132577942,-4.63805343996351));
#55159=CARTESIAN_POINT('Ctrl Pts',(-45.1666666666667,-8.85937132577942,
-4.63805343996351));
#55160=CARTESIAN_POINT('Ctrl Pts',(-40.3333333333333,-8.85937132577942,
-4.63805343996351));
#55161=CARTESIAN_POINT('Ctrl Pts',(-30.8333333333333,-8.85937132577942,
-4.63805343996351));
#55162=CARTESIAN_POINT('Ctrl Pts',(-26.1666666666667,-8.85937132577942,
-4.63805343996351));
#55163=CARTESIAN_POINT('Ctrl Pts',(-21.5,-8.85937132577942,-4.63805343996351));
#55164=CARTESIAN_POINT('',(-50.,-6.03932124977421,-3.89701874412038));
#55165=CARTESIAN_POINT('Ctrl Pts',(-21.5,-8.85937132577942,-4.63805343996351));
#55166=CARTESIAN_POINT('Ctrl Pts',(-21.4716714037532,-8.82699312116188,
-4.63882198977592));
#55167=CARTESIAN_POINT('Ctrl Pts',(-21.442415011075,-8.79205190661509,-4.64240188595699));
#55168=CARTESIAN_POINT('Ctrl Pts',(-21.2909879716453,-8.60695266172876,
-4.66814581613047));
#55169=CARTESIAN_POINT('Ctrl Pts',(-21.1630186724949,-8.43596084926626,
-4.71373942955307));
#55170=CARTESIAN_POINT('Ctrl Pts',(-21.,-8.24274231917123,-4.72304976257329));
#55171=CARTESIAN_POINT('Origin',(-50.,0.,0.));
#55172=CARTESIAN_POINT('',(-50.,-5.14318775290069,-5.02073460645077));
#55173=CARTESIAN_POINT('Ctrl Pts',(-50.,-6.55597468860601,-8.32941749958287));
#55174=CARTESIAN_POINT('Ctrl Pts',(-21.,-6.55597468860601,-8.32941749958287));
#55175=CARTESIAN_POINT('Ctrl Pts',(-50.,-6.55632766789962,-8.30553668898452));
#55176=CARTESIAN_POINT('Ctrl Pts',(-21.,-6.55632766789962,-8.30553668898452));
#55177=CARTESIAN_POINT('Ctrl Pts',(-50.,-6.55682598292761,-8.25785023779518));
#55178=CARTESIAN_POINT('Ctrl Pts',(-21.,-6.55682598292761,-8.25785023779518));
#55179=CARTESIAN_POINT('Ctrl Pts',(-50.,-6.55695052439907,-8.18654607180369));
#55180=CARTESIAN_POINT('Ctrl Pts',(-21.,-6.55695052439907,-8.18654607180369));
#55181=CARTESIAN_POINT('Ctrl Pts',(-50.,-6.55586906420034,-8.0919254651127));
#55182=CARTESIAN_POINT('Ctrl Pts',(-21.,-6.55586906420034,-8.0919254651127));
#55183=CARTESIAN_POINT('Ctrl Pts',(-50.,-6.55242508650163,-7.97441053046901));
#55184=CARTESIAN_POINT('Ctrl Pts',(-21.,-6.55242508650163,-7.97441053046901));
#55185=CARTESIAN_POINT('Ctrl Pts',(-50.,-6.54686687486885,-7.85767464841055));
#55186=CARTESIAN_POINT('Ctrl Pts',(-21.,-6.54686687486885,-7.85767464841055));
#55187=CARTESIAN_POINT('Ctrl Pts',(-50.,-6.53916282696568,-7.74174994850129));
#55188=CARTESIAN_POINT('Ctrl Pts',(-21.,-6.53916282696568,-7.74174994850129));
#55189=CARTESIAN_POINT('Ctrl Pts',(-50.,-6.5292721024685,-7.6266854031787));
#55190=CARTESIAN_POINT('Ctrl Pts',(-21.,-6.5292721024685,-7.6266854031787));
#55191=CARTESIAN_POINT('Ctrl Pts',(-50.,-6.51714368227899,-7.51255191568566));
#55192=CARTESIAN_POINT('Ctrl Pts',(-21.,-6.51714368227899,-7.51255191568566));
#55193=CARTESIAN_POINT('Ctrl Pts',(-50.,-6.5027237919627,-7.39943421923609));
#55194=CARTESIAN_POINT('Ctrl Pts',(-21.,-6.5027237919627,-7.39943421923609));
#55195=CARTESIAN_POINT('Ctrl Pts',(-50.,-6.48596514159778,-7.28741967054497));
#55196=CARTESIAN_POINT('Ctrl Pts',(-21.,-6.48596514159778,-7.28741967054497));
#55197=CARTESIAN_POINT('Ctrl Pts',(-50.,-6.46683693263443,-7.17658703219621));
#55198=CARTESIAN_POINT('Ctrl Pts',(-21.,-6.46683693263443,-7.17658703219621));
#55199=CARTESIAN_POINT('Ctrl Pts',(-50.,-6.44533241567678,-7.06699729667253));
#55200=CARTESIAN_POINT('Ctrl Pts',(-21.,-6.44533241567678,-7.06699729667253));
#55201=CARTESIAN_POINT('Ctrl Pts',(-50.,-6.42148411170256,-6.9586779143977));
#55202=CARTESIAN_POINT('Ctrl Pts',(-21.,-6.42148411170256,-6.9586779143977));
#55203=CARTESIAN_POINT('Ctrl Pts',(-50.,-6.39534644338642,-6.85163598146165));
#55204=CARTESIAN_POINT('Ctrl Pts',(-21.,-6.39534644338642,-6.85163598146165));
#55205=CARTESIAN_POINT('Ctrl Pts',(-50.,-6.36696110296949,-6.74588705654512));
#55206=CARTESIAN_POINT('Ctrl Pts',(-21.,-6.36696110296949,-6.74588705654512));
#55207=CARTESIAN_POINT('Ctrl Pts',(-50.,-6.33632590879467,-6.64148049150319));
#55208=CARTESIAN_POINT('Ctrl Pts',(-21.,-6.33632590879467,-6.64148049150319));
#55209=CARTESIAN_POINT('Ctrl Pts',(-50.,-6.30336681095649,-6.53852299564495));
#55210=CARTESIAN_POINT('Ctrl Pts',(-21.,-6.30336681095649,-6.53852299564495));
#55211=CARTESIAN_POINT('Ctrl Pts',(-50.,-6.2678972444421,-6.43721103768399));
#55212=CARTESIAN_POINT('Ctrl Pts',(-21.,-6.2678972444421,-6.43721103768399));
#55213=CARTESIAN_POINT('Ctrl Pts',(-50.,-6.22963155144596,-6.33782488040964));
#55214=CARTESIAN_POINT('Ctrl Pts',(-21.,-6.22963155144596,-6.33782488040964));
#55215=CARTESIAN_POINT('Ctrl Pts',(-50.,-6.18823844577549,-6.2406935262026));
#55216=CARTESIAN_POINT('Ctrl Pts',(-21.,-6.18823844577549,-6.2406935262026));
#55217=CARTESIAN_POINT('Ctrl Pts',(-50.,-6.14338347043832,-6.14616869769857));
#55218=CARTESIAN_POINT('Ctrl Pts',(-21.,-6.14338347043832,-6.14616869769857));
#55219=CARTESIAN_POINT('Ctrl Pts',(-50.,-6.09477471117184,-6.05459405347559));
#55220=CARTESIAN_POINT('Ctrl Pts',(-21.,-6.09477471117184,-6.05459405347559));
#55221=CARTESIAN_POINT('Ctrl Pts',(-50.,-6.04221154361855,-5.96627851638222));
#55222=CARTESIAN_POINT('Ctrl Pts',(-21.,-6.04221154361855,-5.96627851638222));
#55223=CARTESIAN_POINT('Ctrl Pts',(-50.,-5.98561485393513,-5.88145719317904));
#55224=CARTESIAN_POINT('Ctrl Pts',(-21.,-5.98561485393513,-5.88145719317904));
#55225=CARTESIAN_POINT('Ctrl Pts',(-50.,-5.92504262139805,-5.80024683316115));
#55226=CARTESIAN_POINT('Ctrl Pts',(-21.,-5.92504262139805,-5.80024683316115));
#55227=CARTESIAN_POINT('Ctrl Pts',(-50.,-5.86071379627312,-5.72259822644884));
#55228=CARTESIAN_POINT('Ctrl Pts',(-21.,-5.86071379627312,-5.72259822644884));
#55229=CARTESIAN_POINT('Ctrl Pts',(-50.,-5.79302399301176,-5.64825683559838));
#55230=CARTESIAN_POINT('Ctrl Pts',(-21.,-5.79302399301176,-5.64825683559838));
#55231=CARTESIAN_POINT('Ctrl Pts',(-50.,-5.72258159055366,-5.57669744070723));
#55232=CARTESIAN_POINT('Ctrl Pts',(-21.,-5.72258159055366,-5.57669744070723));
#55233=CARTESIAN_POINT('Ctrl Pts',(-50.,-5.65014634083023,-5.50719043557996));
#55234=CARTESIAN_POINT('Ctrl Pts',(-21.,-5.65014634083023,-5.50719043557996));
#55235=CARTESIAN_POINT('Ctrl Pts',(-50.,-5.57653243923659,-5.43891687637388));
#55236=CARTESIAN_POINT('Ctrl Pts',(-21.,-5.57653243923659,-5.43891687637388));
#55237=CARTESIAN_POINT('Ctrl Pts',(-50.,-5.50252175190725,-5.37106909242141));
#55238=CARTESIAN_POINT('Ctrl Pts',(-21.,-5.50252175190725,-5.37106909242141));
#55239=CARTESIAN_POINT('Ctrl Pts',(-50.,-5.42877754716296,-5.30295185702147));
#55240=CARTESIAN_POINT('Ctrl Pts',(-21.,-5.42877754716296,-5.30295185702147));
#55241=CARTESIAN_POINT('Ctrl Pts',(-50.,-5.35574541658332,-5.23409735978387));
#55242=CARTESIAN_POINT('Ctrl Pts',(-21.,-5.35574541658332,-5.23409735978387));
#55243=CARTESIAN_POINT('Ctrl Pts',(-50.,-5.28368554926634,-5.16423261553338));
#55244=CARTESIAN_POINT('Ctrl Pts',(-21.,-5.28368554926634,-5.16423261553338));
#55245=CARTESIAN_POINT('Ctrl Pts',(-50.,-5.22691734521339,-5.10742564369891));
#55246=CARTESIAN_POINT('Ctrl Pts',(-21.,-5.22691734521339,-5.10742564369891));
#55247=CARTESIAN_POINT('Ctrl Pts',(-50.,-5.18485354740602,-5.06428722179623));
#55248=CARTESIAN_POINT('Ctrl Pts',(-21.,-5.18485354740602,-5.06428722179623));
#55249=CARTESIAN_POINT('Ctrl Pts',(-50.,-5.15703844666268,-5.03529159113598));
#55250=CARTESIAN_POINT('Ctrl Pts',(-21.,-5.15703844666268,-5.03529159113598));
#55251=CARTESIAN_POINT('Ctrl Pts',(-50.,-5.14318775290069,-5.02073460645076));
#55252=CARTESIAN_POINT('Ctrl Pts',(-21.,-5.14318775290069,-5.02073460645076));
#55253=CARTESIAN_POINT('',(-21.5,-6.52388598275277,-7.57884632935924));
#55254=CARTESIAN_POINT('Ctrl Pts',(-21.5,-6.52388598275277,-7.57884632935924));
#55255=CARTESIAN_POINT('Ctrl Pts',(-26.3333333333333,-6.52388598275277,
-7.57884632935924));
#55256=CARTESIAN_POINT('Ctrl Pts',(-31.1666666666667,-6.52388598275277,
-7.57884632935924));
#55257=CARTESIAN_POINT('Ctrl Pts',(-40.6666666666667,-6.52388598275277,
-7.57884632935924));
#55258=CARTESIAN_POINT('Ctrl Pts',(-45.3333333333333,-6.52388598275276,
-7.57884632935924));
#55259=CARTESIAN_POINT('Ctrl Pts',(-50.,-6.52388598275276,-7.57884632935924));
#55260=CARTESIAN_POINT('Ctrl Pts',(-21.,-6.42894112865204,-6.99419158761942));
#55261=CARTESIAN_POINT('Ctrl Pts',(-21.1171767610974,-6.45853087308246,
-7.12615087039119));
#55262=CARTESIAN_POINT('Ctrl Pts',(-21.2874825276444,-6.49694802882356,
-7.32162583711084));
#55263=CARTESIAN_POINT('Ctrl Pts',(-21.5,-6.52388598275277,-7.57884632935924));
#55264=CARTESIAN_POINT('Origin',(-35.75,0.,0.));
#55265=CARTESIAN_POINT('',(-21.5,-9.16615635178499,-3.9976965535958));
#55266=CARTESIAN_POINT('Origin',(-21.5,0.,0.));
#55267=CARTESIAN_POINT('Ctrl Pts',(-21.5,-9.16615635178499,-3.9976965535958));
#55268=CARTESIAN_POINT('Ctrl Pts',(-26.3333333333333,-9.16615635178499,
-3.9976965535958));
#55269=CARTESIAN_POINT('Ctrl Pts',(-31.1666666666667,-9.16615635178499,
-3.9976965535958));
#55270=CARTESIAN_POINT('Ctrl Pts',(-40.6666666666667,-9.16615635178499,
-3.9976965535958));
#55271=CARTESIAN_POINT('Ctrl Pts',(-45.3333333333333,-9.16615635178499,
-3.9976965535958));
#55272=CARTESIAN_POINT('Ctrl Pts',(-50.,-9.16615635178499,-3.9976965535958));
#55273=CARTESIAN_POINT('Origin',(-21.25,0.,0.));
#55274=CARTESIAN_POINT('Ctrl Pts',(-21.,-8.82694180863381,-3.51213586112389));
#55275=CARTESIAN_POINT('Ctrl Pts',(-21.1171767610952,-8.91085623419347,
-3.61818855777691));
#55276=CARTESIAN_POINT('Ctrl Pts',(-21.2874825276427,-9.03028230497426,
-3.77763683806661));
#55277=CARTESIAN_POINT('Ctrl Pts',(-21.5,-9.16615635178499,-3.9976965535958));
#55278=CARTESIAN_POINT('Ctrl Pts',(-50.,-9.52072790258051,-4.66001504343333));
#55279=CARTESIAN_POINT('Ctrl Pts',(-21.,-9.52072790258051,-4.66001504343333));
#55280=CARTESIAN_POINT('Ctrl Pts',(-50.,-9.5106844305395,-4.6383460245682));
#55281=CARTESIAN_POINT('Ctrl Pts',(-21.,-9.5106844305395,-4.6383460245682));
#55282=CARTESIAN_POINT('Ctrl Pts',(-50.,-9.49044302111884,-4.59516580583826));
#55283=CARTESIAN_POINT('Ctrl Pts',(-21.,-9.49044302111884,-4.59516580583826));
#55284=CARTESIAN_POINT('Ctrl Pts',(-50.,-9.45961751095234,-4.53086893560887));
#55285=CARTESIAN_POINT('Ctrl Pts',(-21.,-9.45961751095234,-4.53086893560887));
#55286=CARTESIAN_POINT('Ctrl Pts',(-50.,-9.41758880635275,-4.44608794271298));
#55287=CARTESIAN_POINT('Ctrl Pts',(-21.,-9.41758880635275,-4.44608794271298));
#55288=CARTESIAN_POINT('Ctrl Pts',(-50.,-9.36349807041911,-4.34170493100677));
#55289=CARTESIAN_POINT('Ctrl Pts',(-21.,-9.36349807041911,-4.34170493100677));
#55290=CARTESIAN_POINT('Ctrl Pts',(-50.,-9.30784049378005,-4.23894115315102));
#55291=CARTESIAN_POINT('Ctrl Pts',(-21.,-9.30784049378005,-4.23894115315102));
#55292=CARTESIAN_POINT('Ctrl Pts',(-50.,-9.25060154420976,-4.1378392686224));
#55293=CARTESIAN_POINT('Ctrl Pts',(-21.,-9.25060154420976,-4.1378392686224));
#55294=CARTESIAN_POINT('Ctrl Pts',(-50.,-9.19176567419237,-4.03846112001482));
#55295=CARTESIAN_POINT('Ctrl Pts',(-21.,-9.19176567419237,-4.03846112001482));
#55296=CARTESIAN_POINT('Ctrl Pts',(-50.,-9.13131768087278,-3.94089272529988));
#55297=CARTESIAN_POINT('Ctrl Pts',(-21.,-9.13131768087278,-3.94089272529988));
#55298=CARTESIAN_POINT('Ctrl Pts',(-50.,-9.06924587952332,-3.84523375831808));
#55299=CARTESIAN_POINT('Ctrl Pts',(-21.,-9.06924587952332,-3.84523375831808));
#55300=CARTESIAN_POINT('Ctrl Pts',(-50.,-9.0055455660548,-3.75158344307814));
#55301=CARTESIAN_POINT('Ctrl Pts',(-21.,-9.0055455660548,-3.75158344307814));
#55302=CARTESIAN_POINT('Ctrl Pts',(-50.,-8.94022316573707,-3.66002610520606));
#55303=CARTESIAN_POINT('Ctrl Pts',(-21.,-8.94022316573707,-3.66002610520606));
#55304=CARTESIAN_POINT('Ctrl Pts',(-50.,-8.87329906122102,-3.57061962548306));
#55305=CARTESIAN_POINT('Ctrl Pts',(-21.,-8.87329906122102,-3.57061962548306));
#55306=CARTESIAN_POINT('Ctrl Pts',(-50.,-8.80481446318767,-3.48337462556297));
#55307=CARTESIAN_POINT('Ctrl Pts',(-21.,-8.80481446318767,-3.48337462556297));
#55308=CARTESIAN_POINT('Ctrl Pts',(-50.,-8.7348214836506,-3.3982738856883));
#55309=CARTESIAN_POINT('Ctrl Pts',(-21.,-8.7348214836506,-3.3982738856883));
#55310=CARTESIAN_POINT('Ctrl Pts',(-50.,-8.66336443667969,-3.31531333416059));
#55311=CARTESIAN_POINT('Ctrl Pts',(-21.,-8.66336443667969,-3.31531333416059));
#55312=CARTESIAN_POINT('Ctrl Pts',(-50.,-8.59046276963722,-3.23453838205034));
#55313=CARTESIAN_POINT('Ctrl Pts',(-21.,-8.59046276963722,-3.23453838205034));
#55314=CARTESIAN_POINT('Ctrl Pts',(-50.,-8.51609606529771,-3.15607730017284));
#55315=CARTESIAN_POINT('Ctrl Pts',(-21.,-8.51609606529771,-3.15607730017284));
#55316=CARTESIAN_POINT('Ctrl Pts',(-50.,-8.44018147897284,-3.08018804824792));
#55317=CARTESIAN_POINT('Ctrl Pts',(-21.,-8.44018147897284,-3.08018804824792));
#55318=CARTESIAN_POINT('Ctrl Pts',(-50.,-8.36258324333989,-3.00724707660037));
#55319=CARTESIAN_POINT('Ctrl Pts',(-21.,-8.36258324333989,-3.00724707660037));
#55320=CARTESIAN_POINT('Ctrl Pts',(-50.,-8.28314562863609,-2.93769454582461));
#55321=CARTESIAN_POINT('Ctrl Pts',(-21.,-8.28314562863609,-2.93769454582461));
#55322=CARTESIAN_POINT('Ctrl Pts',(-50.,-8.201719906256,-2.87199246251599));
#55323=CARTESIAN_POINT('Ctrl Pts',(-21.,-8.201719906256,-2.87199246251599));
#55324=CARTESIAN_POINT('Ctrl Pts',(-50.,-8.11819217840571,-2.81057710920625));
#55325=CARTESIAN_POINT('Ctrl Pts',(-21.,-8.11819217840571,-2.81057710920625));
#55326=CARTESIAN_POINT('Ctrl Pts',(-50.,-8.03251572538561,-2.75381386341092));
#55327=CARTESIAN_POINT('Ctrl Pts',(-21.,-8.03251572538561,-2.75381386341092));
#55328=CARTESIAN_POINT('Ctrl Pts',(-50.,-7.94472127708621,-2.70194887521209));
#55329=CARTESIAN_POINT('Ctrl Pts',(-21.,-7.94472127708621,-2.70194887521209));
#55330=CARTESIAN_POINT('Ctrl Pts',(-50.,-7.85491172665132,-2.65506217582471));
#55331=CARTESIAN_POINT('Ctrl Pts',(-21.,-7.85491172665132,-2.65506217582471));
#55332=CARTESIAN_POINT('Ctrl Pts',(-50.,-7.76326299008741,-2.61301442971916));
#55333=CARTESIAN_POINT('Ctrl Pts',(-21.,-7.76326299008741,-2.61301442971916));
#55334=CARTESIAN_POINT('Ctrl Pts',(-50.,-7.67002106404108,-2.5754046559055));
#55335=CARTESIAN_POINT('Ctrl Pts',(-21.,-7.67002106404108,-2.5754046559055));
#55336=CARTESIAN_POINT('Ctrl Pts',(-50.,-7.57550619462173,-2.54149568187359));
#55337=CARTESIAN_POINT('Ctrl Pts',(-21.,-7.57550619462173,-2.54149568187359));
#55338=CARTESIAN_POINT('Ctrl Pts',(-50.,-7.4800863304027,-2.5103005111467));
#55339=CARTESIAN_POINT('Ctrl Pts',(-21.,-7.4800863304027,-2.5103005111467));
#55340=CARTESIAN_POINT('Ctrl Pts',(-50.,-7.3841397096708,-2.4807280346756));
#55341=CARTESIAN_POINT('Ctrl Pts',(-21.,-7.3841397096708,-2.4807280346756));
#55342=CARTESIAN_POINT('Ctrl Pts',(-50.,-7.28802033430286,-2.45171132733138));
#55343=CARTESIAN_POINT('Ctrl Pts',(-21.,-7.28802033430286,-2.45171132733138));
#55344=CARTESIAN_POINT('Ctrl Pts',(-50.,-7.19202414084635,-2.42233623016115));
#55345=CARTESIAN_POINT('Ctrl Pts',(-21.,-7.19202414084635,-2.42233623016115));
#55346=CARTESIAN_POINT('Ctrl Pts',(-50.,-7.09634961812101,-2.39198792562662));
#55347=CARTESIAN_POINT('Ctrl Pts',(-21.,-7.09634961812101,-2.39198792562662));
#55348=CARTESIAN_POINT('Ctrl Pts',(-50.,-7.00111274457534,-2.36030757076476));
#55349=CARTESIAN_POINT('Ctrl Pts',(-21.,-7.00111274457534,-2.36030757076476));
#55350=CARTESIAN_POINT('Ctrl Pts',(-50.,-6.92531873868941,-2.33375705829959));
#55351=CARTESIAN_POINT('Ctrl Pts',(-21.,-6.92531873868941,-2.33375705829959));
#55352=CARTESIAN_POINT('Ctrl Pts',(-50.,-6.86870350660446,-2.31314148102898));
#55353=CARTESIAN_POINT('Ctrl Pts',(-21.,-6.86870350660446,-2.31314148102898));
#55354=CARTESIAN_POINT('Ctrl Pts',(-50.,-6.8310622341282,-2.29908584041335));
#55355=CARTESIAN_POINT('Ctrl Pts',(-21.,-6.8310622341282,-2.29908584041335));
#55356=CARTESIAN_POINT('Ctrl Pts',(-50.,-6.8122671513043,-2.29198004120026));
#55357=CARTESIAN_POINT('Ctrl Pts',(-21.,-6.8122671513043,-2.29198004120026));
#55358=CARTESIAN_POINT('',(-50.,-6.8122671513043,-2.29198004120026));
#55359=CARTESIAN_POINT('Origin',(-50.,0.,0.));
#55360=CARTESIAN_POINT('',(-50.,-7.13209349341826,-0.89072928050049));
#55361=CARTESIAN_POINT('Ctrl Pts',(-50.,-7.13209349341826,-0.89072928050049));
#55362=CARTESIAN_POINT('Ctrl Pts',(-21.,-7.13209349341826,-0.89072928050049));
#55363=CARTESIAN_POINT('Ctrl Pts',(-50.,-7.15577920638447,-0.893054239868308));
#55364=CARTESIAN_POINT('Ctrl Pts',(-21.,-7.15577920638447,-0.893054239868308));
#55365=CARTESIAN_POINT('Ctrl Pts',(-50.,-7.20314083161155,-0.89786893854071));
#55366=CARTESIAN_POINT('Ctrl Pts',(-21.,-7.20314083161155,-0.89786893854071));
#55367=CARTESIAN_POINT('Ctrl Pts',(-50.,-7.27415386726379,-0.90558533966873));
#55368=CARTESIAN_POINT('Ctrl Pts',(-21.,-7.27415386726379,-0.90558533966873));
#55369=CARTESIAN_POINT('Ctrl Pts',(-50.,-7.36877903277666,-0.916863781503486));
#55370=CARTESIAN_POINT('Ctrl Pts',(-21.,-7.36877903277666,-0.916863781503486));
#55371=CARTESIAN_POINT('Ctrl Pts',(-50.,-7.4869674381447,-0.932516236860826));
#55372=CARTESIAN_POINT('Ctrl Pts',(-21.,-7.4869674381447,-0.932516236860826));
#55373=CARTESIAN_POINT('Ctrl Pts',(-50.,-7.60507887157754,-0.949420915891056));
#55374=CARTESIAN_POINT('Ctrl Pts',(-21.,-7.60507887157754,-0.949420915891056));
#55375=CARTESIAN_POINT('Ctrl Pts',(-50.,-7.72314614047142,-0.966965984543332));
#55376=CARTESIAN_POINT('Ctrl Pts',(-21.,-7.72314614047142,-0.966965984543332));
#55377=CARTESIAN_POINT('Ctrl Pts',(-50.,-7.84122460090589,-0.984110042106142));
#55378=CARTESIAN_POINT('Ctrl Pts',(-21.,-7.84122460090589,-0.984110042106142));
#55379=CARTESIAN_POINT('Ctrl Pts',(-50.,-7.95940371279084,-0.999455440216892));
#55380=CARTESIAN_POINT('Ctrl Pts',(-21.,-7.95940371279084,-0.999455440216892));
#55381=CARTESIAN_POINT('Ctrl Pts',(-50.,-8.0778221648407,-1.01133055607812));
#55382=CARTESIAN_POINT('Ctrl Pts',(-21.,-8.0778221648407,-1.01133055607812));
#55383=CARTESIAN_POINT('Ctrl Pts',(-50.,-8.19667636355292,-1.01788199103989));
#55384=CARTESIAN_POINT('Ctrl Pts',(-21.,-8.19667636355292,-1.01788199103989));
#55385=CARTESIAN_POINT('Ctrl Pts',(-50.,-8.31624650623966,-1.017123671327));
#55386=CARTESIAN_POINT('Ctrl Pts',(-21.,-8.31624650623966,-1.017123671327));
#55387=CARTESIAN_POINT('Ctrl Pts',(-50.,-8.43677899171613,-1.00737622330388));
#55388=CARTESIAN_POINT('Ctrl Pts',(-21.,-8.43677899171613,-1.00737622330388));
#55389=CARTESIAN_POINT('Ctrl Pts',(-50.,-8.55832200571467,-0.98784980243911));
#55390=CARTESIAN_POINT('Ctrl Pts',(-21.,-8.55832200571467,-0.98784980243911));
#55391=CARTESIAN_POINT('Ctrl Pts',(-50.,-8.68060673111004,-0.959073494961789));
#55392=CARTESIAN_POINT('Ctrl Pts',(-21.,-8.68060673111004,-0.959073494961789));
#55393=CARTESIAN_POINT('Ctrl Pts',(-50.,-8.80283221651881,-0.923666931425906));
#55394=CARTESIAN_POINT('Ctrl Pts',(-21.,-8.80283221651881,-0.923666931425906));
#55395=CARTESIAN_POINT('Ctrl Pts',(-50.,-8.92394083882956,-0.885365181899303));
#55396=CARTESIAN_POINT('Ctrl Pts',(-21.,-8.92394083882956,-0.885365181899303));
#55397=CARTESIAN_POINT('Ctrl Pts',(-50.,-9.04313782728701,-0.847184879177381));
#55398=CARTESIAN_POINT('Ctrl Pts',(-21.,-9.04313782728701,-0.847184879177381));
#55399=CARTESIAN_POINT('Ctrl Pts',(-50.,-9.1602494406401,-0.810145236641717));
#55400=CARTESIAN_POINT('Ctrl Pts',(-21.,-9.1602494406401,-0.810145236641717));
#55401=CARTESIAN_POINT('Ctrl Pts',(-50.,-9.27634845263042,-0.771090641047726));
#55402=CARTESIAN_POINT('Ctrl Pts',(-21.,-9.27634845263042,-0.771090641047726));
#55403=CARTESIAN_POINT('Ctrl Pts',(-50.,-9.39347368681776,-0.723542272923874));
#55404=CARTESIAN_POINT('Ctrl Pts',(-21.,-9.39347368681776,-0.723542272923874));
#55405=CARTESIAN_POINT('Ctrl Pts',(-50.,-9.51346503399365,-0.66149692044243));
#55406=CARTESIAN_POINT('Ctrl Pts',(-21.,-9.51346503399365,-0.66149692044243));
#55407=CARTESIAN_POINT('Ctrl Pts',(-50.,-9.63711058491003,-0.582194086890198));
#55408=CARTESIAN_POINT('Ctrl Pts',(-21.,-9.63711058491003,-0.582194086890198));
#55409=CARTESIAN_POINT('Ctrl Pts',(-50.,-9.76300600524289,-0.489818901108928));
#55410=CARTESIAN_POINT('Ctrl Pts',(-21.,-9.76300600524289,-0.489818901108928));
#55411=CARTESIAN_POINT('Ctrl Pts',(-50.,-9.88700914008587,-0.397288908358524));
#55412=CARTESIAN_POINT('Ctrl Pts',(-21.,-9.88700914008587,-0.397288908358524));
#55413=CARTESIAN_POINT('Ctrl Pts',(-50.,-10.0034077194239,-0.322542614674783));
#55414=CARTESIAN_POINT('Ctrl Pts',(-21.,-10.0034077194239,-0.322542614674783));
#55415=CARTESIAN_POINT('Ctrl Pts',(-50.,-10.1057999094475,-0.285750111589544));
#55416=CARTESIAN_POINT('Ctrl Pts',(-21.,-10.1057999094475,-0.285750111589544));
#55417=CARTESIAN_POINT('Ctrl Pts',(-50.,-10.1880600728826,-0.306249742693304));
#55418=CARTESIAN_POINT('Ctrl Pts',(-21.,-10.1880600728826,-0.306249742693304));
#55419=CARTESIAN_POINT('Ctrl Pts',(-50.,-10.2453310344199,-0.399403984752717));
#55420=CARTESIAN_POINT('Ctrl Pts',(-21.,-10.2453310344199,-0.399403984752717));
#55421=CARTESIAN_POINT('Ctrl Pts',(-50.,-10.2739254957461,-0.576902635874918));
#55422=CARTESIAN_POINT('Ctrl Pts',(-21.,-10.2739254957461,-0.576902635874918));
#55423=CARTESIAN_POINT('Ctrl Pts',(-50.,-10.2711360438186,-0.847355944984258));
#55424=CARTESIAN_POINT('Ctrl Pts',(-21.,-10.2711360438186,-0.847355944984258));
#55425=CARTESIAN_POINT('Ctrl Pts',(-50.,-10.23508746503,-1.21675444348887));
#55426=CARTESIAN_POINT('Ctrl Pts',(-21.,-10.23508746503,-1.21675444348887));
#55427=CARTESIAN_POINT('Ctrl Pts',(-50.,-10.1645797371964,-1.68895887943845));
#55428=CARTESIAN_POINT('Ctrl Pts',(-21.,-10.1645797371964,-1.68895887943845));
#55429=CARTESIAN_POINT('Ctrl Pts',(-50.,-10.0589430297105,-2.26615269674877));
#55430=CARTESIAN_POINT('Ctrl Pts',(-21.,-10.0589430297105,-2.26615269674877));
#55431=CARTESIAN_POINT('Ctrl Pts',(-50.,-9.91789485710769,-2.94928822483091));
#55432=CARTESIAN_POINT('Ctrl Pts',(-21.,-9.91789485710769,-2.94928822483091));
#55433=CARTESIAN_POINT('Ctrl Pts',(-50.,-9.77670130881801,-3.5806699311609));
#55434=CARTESIAN_POINT('Ctrl Pts',(-21.,-9.77670130881801,-3.5806699311609));
#55435=CARTESIAN_POINT('Ctrl Pts',(-50.,-9.65489431545908,-4.10184205893951));
#55436=CARTESIAN_POINT('Ctrl Pts',(-21.,-9.65489431545908,-4.10184205893951));
#55437=CARTESIAN_POINT('Ctrl Pts',(-50.,-9.56662712803709,-4.47043349004179));
#55438=CARTESIAN_POINT('Ctrl Pts',(-21.,-9.56662712803709,-4.47043349004179));
#55439=CARTESIAN_POINT('Ctrl Pts',(-50.,-9.52072790258051,-4.66001504343333));
#55440=CARTESIAN_POINT('Ctrl Pts',(-21.,-9.52072790258051,-4.66001504343333));
#55441=CARTESIAN_POINT('',(-21.5,-9.99439372247306,-0.334804600014791));
#55442=CARTESIAN_POINT('Ctrl Pts',(-21.5,-9.99439372247306,-0.334804600014791));
#55443=CARTESIAN_POINT('Ctrl Pts',(-21.4716714037528,-9.96555542937999,
-0.349545415954781));
#55444=CARTESIAN_POINT('Ctrl Pts',(-21.4424150110742,-9.9356277416069,-0.367931215781418));
#55445=CARTESIAN_POINT('Ctrl Pts',(-21.2909879716444,-9.78002895717525,
-0.471437247884559));
#55446=CARTESIAN_POINT('Ctrl Pts',(-21.1630186724943,-9.6457529849523,-0.586706241102769));
#55447=CARTESIAN_POINT('Ctrl Pts',(-21.,-9.47570870673866,-0.678928939607902));
#55448=CARTESIAN_POINT('Ctrl Pts',(-50.,-9.99439372247306,-0.334804600014792));
#55449=CARTESIAN_POINT('Ctrl Pts',(-45.1666666666667,-9.99439372247306,
-0.334804600014792));
#55450=CARTESIAN_POINT('Ctrl Pts',(-40.3333333333333,-9.99439372247306,
-0.334804600014792));
#55451=CARTESIAN_POINT('Ctrl Pts',(-30.8333333333333,-9.99439372247306,
-0.334804600014792));
#55452=CARTESIAN_POINT('Ctrl Pts',(-26.1666666666667,-9.99439372247306,
-0.334804600014791));
#55453=CARTESIAN_POINT('Ctrl Pts',(-21.5,-9.99439372247306,-0.334804600014791));
#55454=CARTESIAN_POINT('Origin',(-21.25,0.,0.));
#55455=CARTESIAN_POINT('Origin',(-21.5,0.,0.));
#55456=CARTESIAN_POINT('Origin',(-35.75,0.,0.));
#55457=CARTESIAN_POINT('Ctrl Pts',(-50.,-6.8122671513043,2.29198004120026));
#55458=CARTESIAN_POINT('Ctrl Pts',(-21.,-6.8122671513043,2.29198004120026));
#55459=CARTESIAN_POINT('Ctrl Pts',(-50.,-6.83461600336474,2.30016217089616));
#55460=CARTESIAN_POINT('Ctrl Pts',(-21.,-6.83461600336474,2.30016217089616));
#55461=CARTESIAN_POINT('Ctrl Pts',(-50.,-6.8793763726903,2.31637371632821));
#55462=CARTESIAN_POINT('Ctrl Pts',(-21.,-6.8793763726903,2.31637371632821));
#55463=CARTESIAN_POINT('Ctrl Pts',(-50.,-6.94670492800217,2.34023288057449));
#55464=CARTESIAN_POINT('Ctrl Pts',(-21.,-6.94670492800217,2.34023288057449));
#55465=CARTESIAN_POINT('Ctrl Pts',(-50.,-7.03685278876406,2.37112767623027));
#55466=CARTESIAN_POINT('Ctrl Pts',(-21.,-7.03685278876406,2.37112767623027));
#55467=CARTESIAN_POINT('Ctrl Pts',(-50.,-7.15012820840451,2.4083053284885));
#55468=CARTESIAN_POINT('Ctrl Pts',(-21.,-7.15012820840451,2.4083053284885));
#55469=CARTESIAN_POINT('Ctrl Pts',(-50.,-7.26387759821705,2.44432136933076));
#55470=CARTESIAN_POINT('Ctrl Pts',(-21.,-7.26387759821705,2.44432136933076));
#55471=CARTESIAN_POINT('Ctrl Pts',(-50.,-7.37786505179862,2.47974127678492));
#55472=CARTESIAN_POINT('Ctrl Pts',(-21.,-7.37786505179862,2.47974127678492));
#55473=CARTESIAN_POINT('Ctrl Pts',(-50.,-7.49168859641893,2.51552733857386));
#55474=CARTESIAN_POINT('Ctrl Pts',(-21.,-7.49168859641893,2.51552733857386));
#55475=CARTESIAN_POINT('Ctrl Pts',(-50.,-7.60482241577417,2.55297760756074));
#55476=CARTESIAN_POINT('Ctrl Pts',(-21.,-7.60482241577417,2.55297760756074));
#55477=CARTESIAN_POINT('Ctrl Pts',(-50.,-7.71666617412861,2.59365833862295));
#55478=CARTESIAN_POINT('Ctrl Pts',(-21.,-7.71666617412861,2.59365833862295));
#55479=CARTESIAN_POINT('Ctrl Pts',(-50.,-7.82659266808561,2.63932460382938));
#55480=CARTESIAN_POINT('Ctrl Pts',(-21.,-7.82659266808561,2.63932460382938));
#55481=CARTESIAN_POINT('Ctrl Pts',(-50.,-7.93399262158453,2.69188736687836));
#55482=CARTESIAN_POINT('Ctrl Pts',(-21.,-7.93399262158453,2.69188736687836));
#55483=CARTESIAN_POINT('Ctrl Pts',(-50.,-8.03835937937461,2.75296659957235));
#55484=CARTESIAN_POINT('Ctrl Pts',(-21.,-8.03835937937461,2.75296659957235));
#55485=CARTESIAN_POINT('Ctrl Pts',(-50.,-8.13939365460193,2.82329483425037));
#55486=CARTESIAN_POINT('Ctrl Pts',(-21.,-8.13939365460193,2.82329483425037));
#55487=CARTESIAN_POINT('Ctrl Pts',(-50.,-8.2370828133169,2.90227874531213));
#55488=CARTESIAN_POINT('Ctrl Pts',(-21.,-8.2370828133169,2.90227874531213));
#55489=CARTESIAN_POINT('Ctrl Pts',(-50.,-8.33184183835821,2.98721060740198));
#55490=CARTESIAN_POINT('Ctrl Pts',(-21.,-8.33184183835821,2.98721060740198));
#55491=CARTESIAN_POINT('Ctrl Pts',(-50.,-8.4243384303954,3.07426635319921));
#55492=CARTESIAN_POINT('Ctrl Pts',(-21.,-8.4243384303954,3.07426635319921));
#55493=CARTESIAN_POINT('Ctrl Pts',(-50.,-8.51516539363766,3.16038325236223));
#55494=CARTESIAN_POINT('Ctrl Pts',(-21.,-8.51516539363766,3.16038325236223));
#55495=CARTESIAN_POINT('Ctrl Pts',(-50.,-8.60460841273967,3.24456764186082));
#55496=CARTESIAN_POINT('Ctrl Pts',(-21.,-8.60460841273967,3.24456764186082));
#55497=CARTESIAN_POINT('Ctrl Pts',(-50.,-8.69226485417113,3.33012809006974));
#55498=CARTESIAN_POINT('Ctrl Pts',(-21.,-8.69226485417113,3.33012809006974));
#55499=CARTESIAN_POINT('Ctrl Pts',(-50.,-8.77716058006919,3.42378642402312));
#55500=CARTESIAN_POINT('Ctrl Pts',(-21.,-8.77716058006919,3.42378642402312));
#55501=CARTESIAN_POINT('Ctrl Pts',(-50.,-8.85834857876282,3.53174964938136));
#55502=CARTESIAN_POINT('Ctrl Pts',(-21.,-8.85834857876282,3.53174964938136));
#55503=CARTESIAN_POINT('Ctrl Pts',(-50.,-8.93534116084886,3.65684682750522));
#55504=CARTESIAN_POINT('Ctrl Pts',(-21.,-8.93534116084886,3.65684682750522));
#55505=CARTESIAN_POINT('Ctrl Pts',(-50.,-9.00868892417181,3.79469796977264));
#55506=CARTESIAN_POINT('Ctrl Pts',(-21.,-9.00868892417181,3.79469796977264));
#55507=CARTESIAN_POINT('Ctrl Pts',(-50.,-9.08026462895257,3.93186755639596));
#55508=CARTESIAN_POINT('Ctrl Pts',(-21.,-9.08026462895257,3.93186755639596));
#55509=CARTESIAN_POINT('Ctrl Pts',(-50.,-9.15270492381554,4.04971509082727));
#55510=CARTESIAN_POINT('Ctrl Pts',(-21.,-9.15270492381554,4.04971509082727));
#55511=CARTESIAN_POINT('Ctrl Pts',(-50.,-9.22899343053301,4.12729029694314));
#55512=CARTESIAN_POINT('Ctrl Pts',(-21.,-9.22899343053301,4.12729029694314));
#55513=CARTESIAN_POINT('Ctrl Pts',(-50.,-9.31200173345042,4.1445121148068));
#55514=CARTESIAN_POINT('Ctrl Pts',(-21.,-9.31200173345042,4.1445121148068));
#55515=CARTESIAN_POINT('Ctrl Pts',(-50.,-9.4040191976898,4.08543198173291));
#55516=CARTESIAN_POINT('Ctrl Pts',(-21.,-9.4040191976898,4.08543198173291));
#55517=CARTESIAN_POINT('Ctrl Pts',(-50.,-9.50679569557631,3.93791789477537));
#55518=CARTESIAN_POINT('Ctrl Pts',(-21.,-9.50679569557631,3.93791789477537));
#55519=CARTESIAN_POINT('Ctrl Pts',(-50.,-9.6216277792442,3.69303758521427));
#55520=CARTESIAN_POINT('Ctrl Pts',(-21.,-9.6216277792442,3.69303758521427));
#55521=CARTESIAN_POINT('Ctrl Pts',(-50.,-9.74942513377921,3.34458014605707));
#55522=CARTESIAN_POINT('Ctrl Pts',(-21.,-9.74942513377921,3.34458014605707));
#55523=CARTESIAN_POINT('Ctrl Pts',(-50.,-9.89078169235227,2.88854649339194));
#55524=CARTESIAN_POINT('Ctrl Pts',(-21.,-9.89078169235227,2.88854649339194));
#55525=CARTESIAN_POINT('Ctrl Pts',(-50.,-10.0460413192499,2.32267878361756));
#55526=CARTESIAN_POINT('Ctrl Pts',(-21.,-10.0460413192499,2.32267878361756));
#55527=CARTESIAN_POINT('Ctrl Pts',(-50.,-10.2153627041086,1.64599643173284));
#55528=CARTESIAN_POINT('Ctrl Pts',(-21.,-10.2153627041086,1.64599643173284));
#55529=CARTESIAN_POINT('Ctrl Pts',(-50.,-10.3620979683038,1.01587958589521));
#55530=CARTESIAN_POINT('Ctrl Pts',(-21.,-10.3620979683038,1.01587958589521));
#55531=CARTESIAN_POINT('Ctrl Pts',(-50.,-10.478481770919,0.493469650218983));
#55532=CARTESIAN_POINT('Ctrl Pts',(-21.,-10.478481770919,0.493469650218983));
#55533=CARTESIAN_POINT('Ctrl Pts',(-50.,-10.5588816113278,0.123082548500185));
#55534=CARTESIAN_POINT('Ctrl Pts',(-21.,-10.5588816113278,0.123082548500185));
#55535=CARTESIAN_POINT('Ctrl Pts',(-50.,-10.5997841913839,-0.0676394565978716));
#55536=CARTESIAN_POINT('Ctrl Pts',(-21.,-10.5997841913839,-0.0676394565978716));
#55537=CARTESIAN_POINT('',(-21.5,-9.14990386923578,4.03475639707581));
#55538=CARTESIAN_POINT('Ctrl Pts',(-50.,-9.14990386923578,4.03475639707581));
#55539=CARTESIAN_POINT('Ctrl Pts',(-45.1666666666667,-9.14990386923578,
4.03475639707581));
#55540=CARTESIAN_POINT('Ctrl Pts',(-40.3333333333333,-9.14990386923578,
4.03475639707581));
#55541=CARTESIAN_POINT('Ctrl Pts',(-30.8333333333333,-9.14990386923578,
4.03475639707581));
#55542=CARTESIAN_POINT('Ctrl Pts',(-26.1666666666667,-9.14990386923578,
4.03475639707581));
#55543=CARTESIAN_POINT('Ctrl Pts',(-21.5,-9.14990386923578,4.03475639707581));
#55544=CARTESIAN_POINT('',(-50.,-6.8122671513043,2.29198004120026));
#55545=CARTESIAN_POINT('Ctrl Pts',(-21.5,-9.14990386923578,4.03475639707581));
#55546=CARTESIAN_POINT('Ctrl Pts',(-21.4716714037525,-9.13031726529289,
4.00896291438906));
#55547=CARTESIAN_POINT('Ctrl Pts',(-21.4424150110734,-9.11133064989622,
3.97941274405917));
#55548=CARTESIAN_POINT('Ctrl Pts',(-21.2909879716434,-9.01605057346993,
3.81864524910234));
#55549=CARTESIAN_POINT('Ctrl Pts',(-21.1630186724937,-8.94508544457167,
3.65653131387716));
#55550=CARTESIAN_POINT('Ctrl Pts',(-21.,-8.83189477299562,3.49966208636385));
#55551=CARTESIAN_POINT('Origin',(-50.,0.,0.));
#55552=CARTESIAN_POINT('',(-50.,-7.13209349341826,0.890729280500487));
#55553=CARTESIAN_POINT('Ctrl Pts',(-50.,-10.5997841913839,-0.0676394565978716));
#55554=CARTESIAN_POINT('Ctrl Pts',(-21.,-10.5997841913839,-0.0676394565978716));
#55555=CARTESIAN_POINT('Ctrl Pts',(-50.,-10.5813335008211,-0.0524740444052785));
#55556=CARTESIAN_POINT('Ctrl Pts',(-21.,-10.5813335008211,-0.0524740444052785));
#55557=CARTESIAN_POINT('Ctrl Pts',(-50.,-10.5443614263321,-0.0223524300248229));
#55558=CARTESIAN_POINT('Ctrl Pts',(-21.,-10.5443614263321,-0.0223524300248229));
#55559=CARTESIAN_POINT('Ctrl Pts',(-50.,-10.4886912348662,0.0222023607441701));
#55560=CARTESIAN_POINT('Ctrl Pts',(-21.,-10.4886912348662,0.0222023607441701));
#55561=CARTESIAN_POINT('Ctrl Pts',(-50.,-10.4140395862599,0.0803518244312856));
#55562=CARTESIAN_POINT('Ctrl Pts',(-21.,-10.4140395862599,0.0803518244312856));
#55563=CARTESIAN_POINT('Ctrl Pts',(-50.,-10.3200154257224,0.150928577557961));
#55564=CARTESIAN_POINT('Ctrl Pts',(-21.,-10.3200154257224,0.150928577557961));
#55565=CARTESIAN_POINT('Ctrl Pts',(-50.,-10.2252821497258,0.219366624691659));
#55566=CARTESIAN_POINT('Ctrl Pts',(-21.,-10.2252821497258,0.219366624691659));
#55567=CARTESIAN_POINT('Ctrl Pts',(-50.,-10.1298451744404,0.285621225675486));
#55568=CARTESIAN_POINT('Ctrl Pts',(-21.,-10.1298451744404,0.285621225675486));
#55569=CARTESIAN_POINT('Ctrl Pts',(-50.,-10.0337173245343,0.349629916443316));
#55570=CARTESIAN_POINT('Ctrl Pts',(-21.,-10.0337173245343,0.349629916443316));
#55571=CARTESIAN_POINT('Ctrl Pts',(-50.,-9.93692222450759,0.411308601209035));
#55572=CARTESIAN_POINT('Ctrl Pts',(-21.,-9.93692222450759,0.411308601209035));
#55573=CARTESIAN_POINT('Ctrl Pts',(-50.,-9.83949259364292,0.470562407132083));
#55574=CARTESIAN_POINT('Ctrl Pts',(-21.,-9.83949259364292,0.470562407132083));
#55575=CARTESIAN_POINT('Ctrl Pts',(-50.,-9.74146724538631,0.527299895441832));
#55576=CARTESIAN_POINT('Ctrl Pts',(-21.,-9.74146724538631,0.527299895441832));
#55577=CARTESIAN_POINT('Ctrl Pts',(-50.,-9.64288855622378,0.581447879194613));
#55578=CARTESIAN_POINT('Ctrl Pts',(-21.,-9.64288855622378,0.581447879194613));
#55579=CARTESIAN_POINT('Ctrl Pts',(-50.,-9.54380000381903,0.632963053309265));
#55580=CARTESIAN_POINT('Ctrl Pts',(-21.,-9.54380000381903,0.632963053309265));
#55581=CARTESIAN_POINT('Ctrl Pts',(-50.,-9.44424332627553,0.68185372865074));
#55582=CARTESIAN_POINT('Ctrl Pts',(-21.,-9.44424332627553,0.68185372865074));
#55583=CARTESIAN_POINT('Ctrl Pts',(-50.,-9.34425800352241,0.728158030239756));
#55584=CARTESIAN_POINT('Ctrl Pts',(-21.,-9.34425800352241,0.728158030239756));
#55585=CARTESIAN_POINT('Ctrl Pts',(-50.,-9.24388219451328,0.771898853704203));
#55586=CARTESIAN_POINT('Ctrl Pts',(-21.,-9.24388219451328,0.771898853704203));
#55587=CARTESIAN_POINT('Ctrl Pts',(-50.,-9.14315312384119,0.813043722977555));
#55588=CARTESIAN_POINT('Ctrl Pts',(-21.,-9.14315312384119,0.813043722977555));
#55589=CARTESIAN_POINT('Ctrl Pts',(-50.,-9.04210805084257,0.851468211346448));
#55590=CARTESIAN_POINT('Ctrl Pts',(-21.,-9.04210805084257,0.851468211346448));
#55591=CARTESIAN_POINT('Ctrl Pts',(-50.,-8.94078425956014,0.886903960171005));
#55592=CARTESIAN_POINT('Ctrl Pts',(-21.,-8.94078425956014,0.886903960171005));
#55593=CARTESIAN_POINT('Ctrl Pts',(-50.,-8.83922276353739,0.918952892194649));
#55594=CARTESIAN_POINT('Ctrl Pts',(-21.,-8.83922276353739,0.918952892194649));
#55595=CARTESIAN_POINT('Ctrl Pts',(-50.,-8.73747423363077,0.947150867813171));
#55596=CARTESIAN_POINT('Ctrl Pts',(-21.,-8.73747423363077,0.947150867813171));
#55597=CARTESIAN_POINT('Ctrl Pts',(-50.,-8.63560512714608,0.971017102543951));
#55598=CARTESIAN_POINT('Ctrl Pts',(-21.,-8.63560512714608,0.971017102543951));
#55599=CARTESIAN_POINT('Ctrl Pts',(-50.,-8.53370212161309,0.990109101007577));
#55600=CARTESIAN_POINT('Ctrl Pts',(-21.,-8.53370212161309,0.990109101007577));
#55601=CARTESIAN_POINT('Ctrl Pts',(-50.,-8.43188165539955,1.00407739851957));
#55602=CARTESIAN_POINT('Ctrl Pts',(-21.,-8.43188165539955,1.00407739851957));
#55603=CARTESIAN_POINT('Ctrl Pts',(-50.,-8.33027821569813,1.01271355471894));
#55604=CARTESIAN_POINT('Ctrl Pts',(-21.,-8.33027821569813,1.01271355471894));
#55605=CARTESIAN_POINT('Ctrl Pts',(-50.,-8.2290192302709,1.01599010763451));
#55606=CARTESIAN_POINT('Ctrl Pts',(-21.,-8.2290192302709,1.01599010763451));
#55607=CARTESIAN_POINT('Ctrl Pts',(-50.,-8.12820273854249,1.01410892133532));
#55608=CARTESIAN_POINT('Ctrl Pts',(-21.,-8.12820273854249,1.01410892133532));
#55609=CARTESIAN_POINT('Ctrl Pts',(-50.,-8.02787639670185,1.00753800115478));
#55610=CARTESIAN_POINT('Ctrl Pts',(-21.,-8.02787639670185,1.00753800115478));
#55611=CARTESIAN_POINT('Ctrl Pts',(-50.,-7.92800888935854,0.997080466154163));
#55612=CARTESIAN_POINT('Ctrl Pts',(-21.,-7.92800888935854,0.997080466154163));
#55613=CARTESIAN_POINT('Ctrl Pts',(-50.,-7.82850348500033,0.983785216334555));
#55614=CARTESIAN_POINT('Ctrl Pts',(-21.,-7.82850348500033,0.983785216334555));
#55615=CARTESIAN_POINT('Ctrl Pts',(-50.,-7.7292275500742,0.968799418422935));
#55616=CARTESIAN_POINT('Ctrl Pts',(-21.,-7.7292275500742,0.968799418422935));
#55617=CARTESIAN_POINT('Ctrl Pts',(-50.,-7.63003710778607,0.953237934402831));
#55618=CARTESIAN_POINT('Ctrl Pts',(-21.,-7.63003710778607,0.953237934402831));
#55619=CARTESIAN_POINT('Ctrl Pts',(-50.,-7.53080214904746,0.938052795086852));
#55620=CARTESIAN_POINT('Ctrl Pts',(-21.,-7.53080214904746,0.938052795086852));
#55621=CARTESIAN_POINT('Ctrl Pts',(-50.,-7.43143474677318,0.923884053007731));
#55622=CARTESIAN_POINT('Ctrl Pts',(-21.,-7.43143474677318,0.923884053007731));
#55623=CARTESIAN_POINT('Ctrl Pts',(-50.,-7.33188369780814,0.911105335666499));
#55624=CARTESIAN_POINT('Ctrl Pts',(-21.,-7.33188369780814,0.911105335666499));
#55625=CARTESIAN_POINT('Ctrl Pts',(-50.,-7.25207582250743,0.902140734147994));
#55626=CARTESIAN_POINT('Ctrl Pts',(-21.,-7.25207582250743,0.902140734147994));
#55627=CARTESIAN_POINT('Ctrl Pts',(-50.,-7.19212249719958,0.89615029887462));
#55628=CARTESIAN_POINT('Ctrl Pts',(-21.,-7.19212249719958,0.89615029887462));
#55629=CARTESIAN_POINT('Ctrl Pts',(-50.,-7.15211036864424,0.892482057440589));
#55630=CARTESIAN_POINT('Ctrl Pts',(-21.,-7.15211036864424,0.892482057440589));
#55631=CARTESIAN_POINT('Ctrl Pts',(-50.,-7.13209349341826,0.890729280500492));
#55632=CARTESIAN_POINT('Ctrl Pts',(-21.,-7.13209349341826,0.890729280500492));
#55633=CARTESIAN_POINT('',(-21.5,-9.99295703981581,0.375246053138013));
#55634=CARTESIAN_POINT('Ctrl Pts',(-21.5,-9.99295703981581,0.375246053138014));
#55635=CARTESIAN_POINT('Ctrl Pts',(-26.3333333333333,-9.99295703981581,
0.375246053138014));
#55636=CARTESIAN_POINT('Ctrl Pts',(-31.1666666666667,-9.99295703981581,
0.375246053138014));
#55637=CARTESIAN_POINT('Ctrl Pts',(-40.6666666666667,-9.99295703981581,
0.375246053138014));
#55638=CARTESIAN_POINT('Ctrl Pts',(-45.3333333333333,-9.99295703981581,
0.375246053138014));
#55639=CARTESIAN_POINT('Ctrl Pts',(-50.,-9.99295703981581,0.375246053138014));
#55640=CARTESIAN_POINT('Ctrl Pts',(-21.,-9.47665840807863,0.665541446186863));
#55641=CARTESIAN_POINT('Ctrl Pts',(-21.0648600646508,-9.54397725880582,
0.632805485551036));
#55642=CARTESIAN_POINT('Ctrl Pts',(-21.1289204402943,-9.61037774907841,
0.598586462592499));
#55643=CARTESIAN_POINT('Ctrl Pts',(-21.1924157855611,-9.67606071176893,
0.562824879831496));
#55644=CARTESIAN_POINT('Ctrl Pts',(-21.2961101180201,-9.7833276451402,0.504422591655944));
#55645=CARTESIAN_POINT('Ctrl Pts',(-21.3982975031995,-9.88867999737076,
0.441915547520289));
#55646=CARTESIAN_POINT('Ctrl Pts',(-21.5,-9.99295703981581,0.375246053138013));
#55647=CARTESIAN_POINT('Origin',(-35.75,0.,0.));
#55648=CARTESIAN_POINT('',(-21.5,-8.84053003053573,4.67386657695701));
#55649=CARTESIAN_POINT('Origin',(-21.5,0.,0.));
#55650=CARTESIAN_POINT('Ctrl Pts',(-21.5,-8.84053003053573,4.67386657695702));
#55651=CARTESIAN_POINT('Ctrl Pts',(-26.3333333333333,-8.84053003053573,
4.67386657695702));
#55652=CARTESIAN_POINT('Ctrl Pts',(-31.1666666666667,-8.84053003053573,
4.67386657695702));
#55653=CARTESIAN_POINT('Ctrl Pts',(-40.6666666666667,-8.84053003053573,
4.67386657695702));
#55654=CARTESIAN_POINT('Ctrl Pts',(-45.3333333333333,-8.84053003053573,
4.67386657695702));
#55655=CARTESIAN_POINT('Ctrl Pts',(-50.,-8.84053003053573,4.67386657695702));
#55656=CARTESIAN_POINT('Origin',(-21.25,0.,0.));
#55657=CARTESIAN_POINT('Ctrl Pts',(-21.,-8.24940658621528,4.71140010775012));
#55658=CARTESIAN_POINT('Ctrl Pts',(-21.1171767610998,-8.38464171182995,
4.71088427266307));
#55659=CARTESIAN_POINT('Ctrl Pts',(-21.2874825276465,-8.58376433439286,
4.70484095794187));
#55660=CARTESIAN_POINT('Ctrl Pts',(-21.5,-8.84053003053573,4.67386657695702));
#55661=CARTESIAN_POINT('Ctrl Pts',(-50.,-9.57942322326164,4.53813295416029));
#55662=CARTESIAN_POINT('Ctrl Pts',(-21.,-9.57942322326164,4.53813295416029));
#55663=CARTESIAN_POINT('Ctrl Pts',(-50.,-9.55621969972587,4.54379106380403));
#55664=CARTESIAN_POINT('Ctrl Pts',(-21.,-9.55621969972587,4.54379106380403));
#55665=CARTESIAN_POINT('Ctrl Pts',(-50.,-9.50983973295391,4.55488811868959));
#55666=CARTESIAN_POINT('Ctrl Pts',(-21.,-9.50983973295391,4.55488811868959));
#55667=CARTESIAN_POINT('Ctrl Pts',(-50.,-9.44035102435851,4.57087620725774));
#55668=CARTESIAN_POINT('Ctrl Pts',(-21.,-9.44035102435851,4.57087620725774));
#55669=CARTESIAN_POINT('Ctrl Pts',(-50.,-9.34786210629442,4.59087692729648));
#55670=CARTESIAN_POINT('Ctrl Pts',(-21.,-9.34786210629442,4.59087692729648));
#55671=CARTESIAN_POINT('Ctrl Pts',(-50.,-9.23252715927803,4.61366883031981));
#55672=CARTESIAN_POINT('Ctrl Pts',(-21.,-9.23252715927803,4.61366883031981));
#55673=CARTESIAN_POINT('Ctrl Pts',(-50.,-9.11748127106242,4.63422615215906));
#55674=CARTESIAN_POINT('Ctrl Pts',(-21.,-9.11748127106242,4.63422615215906));
#55675=CARTESIAN_POINT('Ctrl Pts',(-50.,-9.00274873347492,4.65251093331389));
#55676=CARTESIAN_POINT('Ctrl Pts',(-21.,-9.00274873347492,4.65251093331389));
#55677=CARTESIAN_POINT('Ctrl Pts',(-50.,-8.8883682032848,4.66847246002033));
#55678=CARTESIAN_POINT('Ctrl Pts',(-21.,-8.8883682032848,4.66847246002033));
#55679=CARTESIAN_POINT('Ctrl Pts',(-50.,-8.7743974532252,4.68204521487955));
#55680=CARTESIAN_POINT('Ctrl Pts',(-21.,-8.7743974532252,4.68204521487955));
#55681=CARTESIAN_POINT('Ctrl Pts',(-50.,-8.66090712613407,4.69315791678054));
#55682=CARTESIAN_POINT('Ctrl Pts',(-21.,-8.66090712613407,4.69315791678054));
#55683=CARTESIAN_POINT('Ctrl Pts',(-50.,-8.5479718655136,4.70174502276072));
#55684=CARTESIAN_POINT('Ctrl Pts',(-21.,-8.5479718655136,4.70174502276072));
#55685=CARTESIAN_POINT('Ctrl Pts',(-50.,-8.4356616058832,4.70775898013052));
#55686=CARTESIAN_POINT('Ctrl Pts',(-21.,-8.4356616058832,4.70775898013052));
#55687=CARTESIAN_POINT('Ctrl Pts',(-50.,-8.32403430863484,4.71117963661127));
#55688=CARTESIAN_POINT('Ctrl Pts',(-21.,-8.32403430863484,4.71117963661127));
#55689=CARTESIAN_POINT('Ctrl Pts',(-50.,-8.21312397255121,4.71203258951797));
#55690=CARTESIAN_POINT('Ctrl Pts',(-21.,-8.21312397255121,4.71203258951797));
#55691=CARTESIAN_POINT('Ctrl Pts',(-50.,-8.1029496259928,4.71036931800664));
#55692=CARTESIAN_POINT('Ctrl Pts',(-21.,-8.1029496259928,4.71036931800664));
#55693=CARTESIAN_POINT('Ctrl Pts',(-50.,-7.99353571494822,4.70622700687469));
#55694=CARTESIAN_POINT('Ctrl Pts',(-21.,-7.99353571494822,4.70622700687469));
#55695=CARTESIAN_POINT('Ctrl Pts',(-50.,-7.8849298684541,4.69959254734285));
#55696=CARTESIAN_POINT('Ctrl Pts',(-21.,-7.8849298684541,4.69959254734285));
#55697=CARTESIAN_POINT('Ctrl Pts',(-50.,-7.77721964274024,4.69037000103626));
#55698=CARTESIAN_POINT('Ctrl Pts',(-21.,-7.77721964274024,4.69037000103626));
#55699=CARTESIAN_POINT('Ctrl Pts',(-50.,-7.67055506601851,4.67833376211481));
#55700=CARTESIAN_POINT('Ctrl Pts',(-21.,-7.67055506601851,4.67833376211481));
#55701=CARTESIAN_POINT('Ctrl Pts',(-50.,-7.56514580946327,4.66314297047291));
#55702=CARTESIAN_POINT('Ctrl Pts',(-21.,-7.56514580946327,4.66314297047291));
#55703=CARTESIAN_POINT('Ctrl Pts',(-50.,-7.46123890856565,4.64440143603747));
#55704=CARTESIAN_POINT('Ctrl Pts',(-21.,-7.46123890856565,4.64440143603747));
#55705=CARTESIAN_POINT('Ctrl Pts',(-50.,-7.35910284385827,4.62170482170181));
#55706=CARTESIAN_POINT('Ctrl Pts',(-21.,-7.35910284385827,4.62170482170181));
#55707=CARTESIAN_POINT('Ctrl Pts',(-50.,-7.25900770064673,4.59469206087561));
#55708=CARTESIAN_POINT('Ctrl Pts',(-21.,-7.25900770064673,4.59469206087561));
#55709=CARTESIAN_POINT('Ctrl Pts',(-50.,-7.16121001331941,4.56309881747208));
#55710=CARTESIAN_POINT('Ctrl Pts',(-21.,-7.16121001331941,4.56309881747208));
#55711=CARTESIAN_POINT('Ctrl Pts',(-50.,-7.06592138953324,4.5267956450212));
#55712=CARTESIAN_POINT('Ctrl Pts',(-21.,-7.06592138953324,4.5267956450212));
#55713=CARTESIAN_POINT('Ctrl Pts',(-50.,-6.9732685530375,4.48581308997575));
#55714=CARTESIAN_POINT('Ctrl Pts',(-21.,-6.9732685530375,4.48581308997575));
#55715=CARTESIAN_POINT('Ctrl Pts',(-50.,-6.88325224876452,4.44037556328962));
#55716=CARTESIAN_POINT('Ctrl Pts',(-21.,-6.88325224876452,4.44037556328962));
#55717=CARTESIAN_POINT('Ctrl Pts',(-50.,-6.79571235355295,4.39092540044367));
#55718=CARTESIAN_POINT('Ctrl Pts',(-21.,-6.79571235355295,4.39092540044367));
#55719=CARTESIAN_POINT('Ctrl Pts',(-50.,-6.71027219290964,4.33817259947066));
#55720=CARTESIAN_POINT('Ctrl Pts',(-21.,-6.71027219290964,4.33817259947066));
#55721=CARTESIAN_POINT('Ctrl Pts',(-50.,-6.62638951409907,4.28302021638686));
#55722=CARTESIAN_POINT('Ctrl Pts',(-21.,-6.62638951409907,4.28302021638686));
#55723=CARTESIAN_POINT('Ctrl Pts',(-50.,-6.54344708143028,4.22644426515767));
#55724=CARTESIAN_POINT('Ctrl Pts',(-21.,-6.54344708143028,4.22644426515767));
#55725=CARTESIAN_POINT('Ctrl Pts',(-50.,-6.46083145580807,4.1693867325325));
#55726=CARTESIAN_POINT('Ctrl Pts',(-21.,-6.46083145580807,4.1693867325325));
#55727=CARTESIAN_POINT('Ctrl Pts',(-50.,-6.37801243240243,4.11264895980536));
#55728=CARTESIAN_POINT('Ctrl Pts',(-21.,-6.37801243240243,4.11264895980536));
#55729=CARTESIAN_POINT('Ctrl Pts',(-50.,-6.29463308326085,4.05676946424956));
#55730=CARTESIAN_POINT('Ctrl Pts',(-21.,-6.29463308326085,4.05676946424956));
#55731=CARTESIAN_POINT('Ctrl Pts',(-50.,-6.21048516503746,4.00206265639536));
#55732=CARTESIAN_POINT('Ctrl Pts',(-21.,-6.21048516503746,4.00206265639536));
#55733=CARTESIAN_POINT('Ctrl Pts',(-50.,-6.14247034880463,3.95935849016754));
#55734=CARTESIAN_POINT('Ctrl Pts',(-21.,-6.14247034880463,3.95935849016754));
#55735=CARTESIAN_POINT('Ctrl Pts',(-50.,-6.09105342163039,3.92794852152394));
#55736=CARTESIAN_POINT('Ctrl Pts',(-21.,-6.09105342163039,3.92794852152394));
#55737=CARTESIAN_POINT('Ctrl Pts',(-50.,-6.0565953297729,3.90728293824429));
#55738=CARTESIAN_POINT('Ctrl Pts',(-21.,-6.0565953297729,3.90728293824429));
#55739=CARTESIAN_POINT('Ctrl Pts',(-50.,-6.03932124977421,3.89701874412039));
#55740=CARTESIAN_POINT('Ctrl Pts',(-21.,-6.03932124977421,3.89701874412039));
#55741=CARTESIAN_POINT('',(-50.,-6.03932124977422,3.89701874412038));
#55742=CARTESIAN_POINT('Origin',(-50.,0.,0.));
#55743=CARTESIAN_POINT('',(-50.,-5.14318775290069,5.02073460645076));
#55744=CARTESIAN_POINT('Ctrl Pts',(-50.,-5.14318775290069,5.02073460645076));
#55745=CARTESIAN_POINT('Ctrl Pts',(-21.,-5.14318775290069,5.02073460645076));
#55746=CARTESIAN_POINT('Ctrl Pts',(-50.,-5.1597732798141,5.03780325407688));
#55747=CARTESIAN_POINT('Ctrl Pts',(-21.,-5.1597732798141,5.03780325407688));
#55748=CARTESIAN_POINT('Ctrl Pts',(-50.,-5.19306705314332,5.071830148219));
#55749=CARTESIAN_POINT('Ctrl Pts',(-21.,-5.19306705314332,5.071830148219));
#55750=CARTESIAN_POINT('Ctrl Pts',(-50.,-5.24337588200476,5.12253927774717));
#55751=CARTESIAN_POINT('Ctrl Pts',(-21.,-5.24337588200476,5.12253927774717));
#55752=CARTESIAN_POINT('Ctrl Pts',(-50.,-5.31119154860082,5.18948821771405));
#55753=CARTESIAN_POINT('Ctrl Pts',(-21.,-5.31119154860082,5.18948821771405));
#55754=CARTESIAN_POINT('Ctrl Pts',(-50.,-5.39711839642203,5.27213248760413));
#55755=CARTESIAN_POINT('Ctrl Pts',(-21.,-5.39711839642203,5.27213248760413));
#55756=CARTESIAN_POINT('Ctrl Pts',(-50.,-5.48397628091718,5.35393582972231));
#55757=CARTESIAN_POINT('Ctrl Pts',(-21.,-5.48397628091718,5.35393582972231));
#55758=CARTESIAN_POINT('Ctrl Pts',(-50.,-5.57130730604024,5.43530536621495));
#55759=CARTESIAN_POINT('Ctrl Pts',(-21.,-5.57130730604024,5.43530536621495));
#55760=CARTESIAN_POINT('Ctrl Pts',(-50.,-5.65833178588016,5.51693367893109));
#55761=CARTESIAN_POINT('Ctrl Pts',(-21.,-5.65833178588016,5.51693367893109));
#55762=CARTESIAN_POINT('Ctrl Pts',(-50.,-5.74401277228714,5.59976212994534));
#55763=CARTESIAN_POINT('Ctrl Pts',(-21.,-5.74401277228714,5.59976212994534));
#55764=CARTESIAN_POINT('Ctrl Pts',(-50.,-5.82712980893039,5.68494139022769));
#55765=CARTESIAN_POINT('Ctrl Pts',(-21.,-5.82712980893039,5.68494139022769));
#55766=CARTESIAN_POINT('Ctrl Pts',(-50.,-5.906356307844,5.77378059171821));
#55767=CARTESIAN_POINT('Ctrl Pts',(-21.,-5.906356307844,5.77378059171821));
#55768=CARTESIAN_POINT('Ctrl Pts',(-50.,-5.98031419419066,5.86773709824143));
#55769=CARTESIAN_POINT('Ctrl Pts',(-21.,-5.98031419419066,5.86773709824143));
#55770=CARTESIAN_POINT('Ctrl Pts',(-50.,-6.04784410793973,5.96805062448362));
#55771=CARTESIAN_POINT('Ctrl Pts',(-21.,-6.04784410793973,5.96805062448362));
#55772=CARTESIAN_POINT('Ctrl Pts',(-50.,-6.108358567083,6.07525130357771));
#55773=CARTESIAN_POINT('Ctrl Pts',(-21.,-6.108358567083,6.07525130357771));
#55774=CARTESIAN_POINT('Ctrl Pts',(-50.,-6.16210362315516,6.18879908596403));
#55775=CARTESIAN_POINT('Ctrl Pts',(-21.,-6.16210362315516,6.18879908596403));
#55776=CARTESIAN_POINT('Ctrl Pts',(-50.,-6.2106280007764,6.30643444970003));
#55777=CARTESIAN_POINT('Ctrl Pts',(-21.,-6.2106280007764,6.30643444970003));
#55778=CARTESIAN_POINT('Ctrl Pts',(-50.,-6.25619247809081,6.42500173364409));
#55779=CARTESIAN_POINT('Ctrl Pts',(-21.,-6.25619247809081,6.42500173364409));
#55780=CARTESIAN_POINT('Ctrl Pts',(-50.,-6.30066002212815,6.5419987212145));
#55781=CARTESIAN_POINT('Ctrl Pts',(-21.,-6.30066002212815,6.5419987212145));
#55782=CARTESIAN_POINT('Ctrl Pts',(-50.,-6.34471916009928,6.65665410688205));
#55783=CARTESIAN_POINT('Ctrl Pts',(-21.,-6.34471916009928,6.65665410688205));
#55784=CARTESIAN_POINT('Ctrl Pts',(-50.,-6.38657159771068,6.77177411160809));
#55785=CARTESIAN_POINT('Ctrl Pts',(-21.,-6.38657159771068,6.77177411160809));
#55786=CARTESIAN_POINT('Ctrl Pts',(-50.,-6.42242317562759,6.89299222970744));
#55787=CARTESIAN_POINT('Ctrl Pts',(-21.,-6.42242317562759,6.89299222970744));
#55788=CARTESIAN_POINT('Ctrl Pts',(-50.,-6.44872754699223,7.02548988707821));
#55789=CARTESIAN_POINT('Ctrl Pts',(-21.,-6.44872754699223,7.02548988707821));
#55790=CARTESIAN_POINT('Ctrl Pts',(-50.,-6.46381783511374,7.17160437943005));
#55791=CARTESIAN_POINT('Ctrl Pts',(-21.,-6.46381783511374,7.17160437943005));
#55792=CARTESIAN_POINT('Ctrl Pts',(-50.,-6.47009051734937,7.32762836882426));
#55793=CARTESIAN_POINT('Ctrl Pts',(-21.,-6.47009051734937,7.32762836882426));
#55794=CARTESIAN_POINT('Ctrl Pts',(-50.,-6.47506234591768,7.48226943041517));
#55795=CARTESIAN_POINT('Ctrl Pts',(-21.,-6.47506234591768,7.48226943041517));
#55796=CARTESIAN_POINT('Ctrl Pts',(-50.,-6.48919666748604,7.61987705609476));
#55797=CARTESIAN_POINT('Ctrl Pts',(-21.,-6.48919666748604,7.61987705609476));
#55798=CARTESIAN_POINT('Ctrl Pts',(-50.,-6.52427161652488,7.72287024427254));
#55799=CARTESIAN_POINT('Ctrl Pts',(-21.,-6.52427161652488,7.72287024427254));
#55800=CARTESIAN_POINT('Ctrl Pts',(-50.,-6.59158724650179,7.774402518864));
#55801=CARTESIAN_POINT('Ctrl Pts',(-21.,-6.59158724650179,7.774402518864));
#55802=CARTESIAN_POINT('Ctrl Pts',(-50.,-6.70012602613047,7.76109803970118));
#55803=CARTESIAN_POINT('Ctrl Pts',(-21.,-6.70012602613047,7.76109803970118));
#55804=CARTESIAN_POINT('Ctrl Pts',(-50.,-6.8567284146999,7.67278549097179));
#55805=CARTESIAN_POINT('Ctrl Pts',(-21.,-6.8567284146999,7.67278549097179));
#55806=CARTESIAN_POINT('Ctrl Pts',(-50.,-7.06643813146967,7.50197972952742));
#55807=CARTESIAN_POINT('Ctrl Pts',(-21.,-7.06643813146967,7.50197972952742));
#55808=CARTESIAN_POINT('Ctrl Pts',(-50.,-7.33276958593085,7.24347961909277));
#55809=CARTESIAN_POINT('Ctrl Pts',(-21.,-7.33276958593085,7.24347961909277));
#55810=CARTESIAN_POINT('Ctrl Pts',(-50.,-7.65799303086079,6.89393980750813));
#55811=CARTESIAN_POINT('Ctrl Pts',(-21.,-7.65799303086079,6.89393980750813));
#55812=CARTESIAN_POINT('Ctrl Pts',(-50.,-8.04339791890053,6.45147524510253));
#55813=CARTESIAN_POINT('Ctrl Pts',(-21.,-8.04339791890053,6.45147524510253));
#55814=CARTESIAN_POINT('Ctrl Pts',(-50.,-8.48955268435888,5.91527130817043));
#55815=CARTESIAN_POINT('Ctrl Pts',(-21.,-8.48955268435888,5.91527130817043));
#55816=CARTESIAN_POINT('Ctrl Pts',(-50.,-8.89515404237518,5.41122169201928));
#55817=CARTESIAN_POINT('Ctrl Pts',(-21.,-8.89515404237518,5.41122169201928));
#55818=CARTESIAN_POINT('Ctrl Pts',(-50.,-9.22667740150299,4.99104364314351));
#55819=CARTESIAN_POINT('Ctrl Pts',(-21.,-9.22667740150299,4.99104364314351));
#55820=CARTESIAN_POINT('Ctrl Pts',(-50.,-9.45982009531033,4.6922205788033));
#55821=CARTESIAN_POINT('Ctrl Pts',(-21.,-9.45982009531033,4.6922205788033));
#55822=CARTESIAN_POINT('Ctrl Pts',(-50.,-9.57942322326164,4.53813295416029));
#55823=CARTESIAN_POINT('Ctrl Pts',(-21.,-9.57942322326164,4.53813295416029));
#55824=CARTESIAN_POINT('',(-21.5,-6.49316333848958,7.60518440668567));
#55825=CARTESIAN_POINT('Ctrl Pts',(-21.5,-6.49316333848958,7.60518440668567));
#55826=CARTESIAN_POINT('Ctrl Pts',(-21.471671403753,-6.48670779082223,7.57344697283542));
#55827=CARTESIAN_POINT('Ctrl Pts',(-21.4424150110746,-6.48242277983734,
7.5385852056463));
#55828=CARTESIAN_POINT('Ctrl Pts',(-21.290987971645,-6.46633279908609,7.35239822189698));
#55829=CARTESIAN_POINT('Ctrl Pts',(-21.1630186724948,-6.47273402762092,
7.17554799773173));
#55830=CARTESIAN_POINT('Ctrl Pts',(-21.,-6.43881576337966,6.98510211559241));
#55831=CARTESIAN_POINT('Ctrl Pts',(-50.,-6.49316333848958,7.60518440668567));
#55832=CARTESIAN_POINT('Ctrl Pts',(-45.1666666666667,-6.49316333848958,
7.60518440668567));
#55833=CARTESIAN_POINT('Ctrl Pts',(-40.3333333333333,-6.49316333848958,
7.60518440668567));
#55834=CARTESIAN_POINT('Ctrl Pts',(-30.8333333333333,-6.49316333848958,
7.60518440668567));
#55835=CARTESIAN_POINT('Ctrl Pts',(-26.1666666666667,-6.49316333848958,
7.60518440668567));
#55836=CARTESIAN_POINT('Ctrl Pts',(-21.5,-6.49316333848958,7.60518440668567));
#55837=CARTESIAN_POINT('Origin',(-21.25,0.,0.));
#55838=CARTESIAN_POINT('Origin',(-21.5,0.,0.));
#55839=CARTESIAN_POINT('Origin',(-35.75,0.,0.));
#55840=CARTESIAN_POINT('Ctrl Pts',(-50.,-2.45543694297674,6.75507110762463));
#55841=CARTESIAN_POINT('Ctrl Pts',(-21.,-2.45543694297674,6.75507110762463));
#55842=CARTESIAN_POINT('Ctrl Pts',(-50.,-2.46297417772978,6.77764561818537));
#55843=CARTESIAN_POINT('Ctrl Pts',(-21.,-2.46297417772978,6.77764561818537));
#55844=CARTESIAN_POINT('Ctrl Pts',(-50.,-2.47820711493347,6.82274841734025));
#55845=CARTESIAN_POINT('Ctrl Pts',(-21.,-2.47820711493347,6.82274841734025));
#55846=CARTESIAN_POINT('Ctrl Pts',(-50.,-2.50153193679118,6.89026394714059));
#55847=CARTESIAN_POINT('Ctrl Pts',(-21.,-2.50153193679118,6.89026394714059));
#55848=CARTESIAN_POINT('Ctrl Pts',(-50.,-2.53358368474749,6.98000697278327));
#55849=CARTESIAN_POINT('Ctrl Pts',(-21.,-2.53358368474749,6.98000697278327));
#55850=CARTESIAN_POINT('Ctrl Pts',(-50.,-2.57514309471485,7.09174914908801));
#55851=CARTESIAN_POINT('Ctrl Pts',(-21.,-2.57514309471485,7.09174914908801));
#55852=CARTESIAN_POINT('Ctrl Pts',(-50.,-2.61790620462629,7.20313763732345));
#55853=CARTESIAN_POINT('Ctrl Pts',(-21.,-2.61790620462629,7.20313763732345));
#55854=CARTESIAN_POINT('Ctrl Pts',(-50.,-2.66128382072048,7.31434056822034));
#55855=CARTESIAN_POINT('Ctrl Pts',(-21.,-2.66128382072048,7.31434056822034));
#55856=CARTESIAN_POINT('Ctrl Pts',(-50.,-2.70427297026251,7.42564364342468));
#55857=CARTESIAN_POINT('Ctrl Pts',(-21.,-2.70427297026251,7.42564364342468));
#55858=CARTESIAN_POINT('Ctrl Pts',(-50.,-2.74553095355499,7.53744508591865));
#55859=CARTESIAN_POINT('Ctrl Pts',(-21.,-2.74553095355499,7.53744508591865));
#55860=CARTESIAN_POINT('Ctrl Pts',(-50.,-2.78345892001629,7.65025207826714));
#55861=CARTESIAN_POINT('Ctrl Pts',(-21.,-2.78345892001629,7.65025207826714));
#55862=CARTESIAN_POINT('Ctrl Pts',(-50.,-2.81629364412744,7.76466852264525));
#55863=CARTESIAN_POINT('Ctrl Pts',(-21.,-2.81629364412744,7.76466852264525));
#55864=CARTESIAN_POINT('Ctrl Pts',(-50.,-2.84216119689693,7.88140953422486));
#55865=CARTESIAN_POINT('Ctrl Pts',(-21.,-2.84216119689693,7.88140953422486));
#55866=CARTESIAN_POINT('Ctrl Pts',(-50.,-2.85947913898695,8.00108902987832));
#55867=CARTESIAN_POINT('Ctrl Pts',(-21.,-2.85947913898695,8.00108902987832));
#55868=CARTESIAN_POINT('Ctrl Pts',(-50.,-2.86748815125169,8.12392974416385));
#55869=CARTESIAN_POINT('Ctrl Pts',(-21.,-2.86748815125169,8.12392974416385));
#55870=CARTESIAN_POINT('Ctrl Pts',(-50.,-2.8666442371861,8.24955186700095));
#55871=CARTESIAN_POINT('Ctrl Pts',(-21.,-2.8666442371861,8.24955186700095));
#55872=CARTESIAN_POINT('Ctrl Pts',(-50.,-2.85932311928695,8.37659160589212));
#55873=CARTESIAN_POINT('Ctrl Pts',(-21.,-2.85932311928695,8.37659160589212));
#55874=CARTESIAN_POINT('Ctrl Pts',(-50.,-2.84893087833482,8.50318672326558));
#55875=CARTESIAN_POINT('Ctrl Pts',(-21.,-2.84893087833482,8.50318672326558));
#55876=CARTESIAN_POINT('Ctrl Pts',(-50.,-2.838231660712,8.62789111098118));
#55877=CARTESIAN_POINT('Ctrl Pts',(-21.,-2.838231660712,8.62789111098118));
#55878=CARTESIAN_POINT('Ctrl Pts',(-50.,-2.8281804649272,8.7503085875302));
#55879=CARTESIAN_POINT('Ctrl Pts',(-21.,-2.8281804649272,8.7503085875302));
#55880=CARTESIAN_POINT('Ctrl Pts',(-50.,-2.81593951016314,8.87218721998315));
#55881=CARTESIAN_POINT('Ctrl Pts',(-21.,-2.81593951016314,8.87218721998315));
#55882=CARTESIAN_POINT('Ctrl Pts',(-50.,-2.79564609540172,8.99695638729624));
#55883=CARTESIAN_POINT('Ctrl Pts',(-21.,-2.79564609540172,8.99695638729624));
#55884=CARTESIAN_POINT('Ctrl Pts',(-50.,-2.76185693608665,9.12774569066013));
#55885=CARTESIAN_POINT('Ctrl Pts',(-21.,-2.76185693608665,9.12774569066013));
#55886=CARTESIAN_POINT('Ctrl Pts',(-50.,-2.71205611361093,9.26593773005304));
#55887=CARTESIAN_POINT('Ctrl Pts',(-21.,-2.71205611361093,9.26593773005304));
#55888=CARTESIAN_POINT('Ctrl Pts',(-50.,-2.65001133311308,9.40923210196585));
#55889=CARTESIAN_POINT('Ctrl Pts',(-21.,-2.65001133311308,9.40923210196585));
#55890=CARTESIAN_POINT('Ctrl Pts',(-50.,-2.5873945538455,9.5507160797281));
#55891=CARTESIAN_POINT('Ctrl Pts',(-21.,-2.5873945538455,9.5507160797281));
#55892=CARTESIAN_POINT('Ctrl Pts',(-50.,-2.54042342638657,9.68082891874335));
#55893=CARTESIAN_POINT('Ctrl Pts',(-21.,-2.54042342638657,9.68082891874335));
#55894=CARTESIAN_POINT('Ctrl Pts',(-50.,-2.52733779392361,9.78884102493588));
#55895=CARTESIAN_POINT('Ctrl Pts',(-21.,-2.52733779392361,9.78884102493588));
#55896=CARTESIAN_POINT('Ctrl Pts',(-50.,-2.56562806487107,9.86447715727042));
#55897=CARTESIAN_POINT('Ctrl Pts',(-21.,-2.56562806487107,9.86447715727042));
#55898=CARTESIAN_POINT('Ctrl Pts',(-50.,-2.6691907234428,9.89958344728561));
#55899=CARTESIAN_POINT('Ctrl Pts',(-21.,-2.6691907234428,9.89958344728561));
#55900=CARTESIAN_POINT('Ctrl Pts',(-50.,-2.84860197903673,9.88796382014256));
#55901=CARTESIAN_POINT('Ctrl Pts',(-21.,-2.84860197903673,9.88796382014256));
#55902=CARTESIAN_POINT('Ctrl Pts',(-50.,-3.11165374758123,9.82506278266417));
#55903=CARTESIAN_POINT('Ctrl Pts',(-21.,-3.11165374758123,9.82506278266417));
#55904=CARTESIAN_POINT('Ctrl Pts',(-50.,-3.46376909107161,9.70771911811945));
#55905=CARTESIAN_POINT('Ctrl Pts',(-21.,-3.46376909107161,9.70771911811945));
#55906=CARTESIAN_POINT('Ctrl Pts',(-50.,-3.90844493048625,9.5339037941241));
#55907=CARTESIAN_POINT('Ctrl Pts',(-21.,-3.90844493048625,9.5339037941241));
#55908=CARTESIAN_POINT('Ctrl Pts',(-50.,-4.44766091491103,9.30247791214345));
#55909=CARTESIAN_POINT('Ctrl Pts',(-21.,-4.44766091491103,9.30247791214345));
#55910=CARTESIAN_POINT('Ctrl Pts',(-50.,-5.08228263794097,9.01295415598311));
#55911=CARTESIAN_POINT('Ctrl Pts',(-21.,-5.08228263794097,9.01295415598311));
#55912=CARTESIAN_POINT('Ctrl Pts',(-50.,-5.66641576644903,8.73480497776003));
#55913=CARTESIAN_POINT('Ctrl Pts',(-21.,-5.66641576644903,8.73480497776003));
#55914=CARTESIAN_POINT('Ctrl Pts',(-50.,-6.14741641494695,8.50008023141016));
#55915=CARTESIAN_POINT('Ctrl Pts',(-21.,-6.14741641494695,8.50008023141016));
#55916=CARTESIAN_POINT('Ctrl Pts',(-50.,-6.48712519233678,8.33200677716551));
#55917=CARTESIAN_POINT('Ctrl Pts',(-21.,-6.48712519233678,8.33200677716551));
#55918=CARTESIAN_POINT('Ctrl Pts',(-50.,-6.6617400018565,8.24507247679879));
#55919=CARTESIAN_POINT('Ctrl Pts',(-21.,-6.6617400018565,8.24507247679879));
#55920=CARTESIAN_POINT('',(-21.5,-2.55037217513312,9.66931237308562));
#55921=CARTESIAN_POINT('Ctrl Pts',(-50.,-2.55037217513312,9.66931237308562));
#55922=CARTESIAN_POINT('Ctrl Pts',(-45.1666666666667,-2.55037217513312,
9.66931237308562));
#55923=CARTESIAN_POINT('Ctrl Pts',(-40.3333333333333,-2.55037217513312,
9.66931237308562));
#55924=CARTESIAN_POINT('Ctrl Pts',(-30.8333333333333,-2.55037217513312,
9.66931237308562));
#55925=CARTESIAN_POINT('Ctrl Pts',(-26.1666666666667,-2.55037217513312,
9.66931237308562));
#55926=CARTESIAN_POINT('Ctrl Pts',(-21.5,-2.55037217513312,9.66931237308562));
#55927=CARTESIAN_POINT('',(-50.,-2.45543694297674,6.75507110762463));
#55928=CARTESIAN_POINT('Ctrl Pts',(-21.5,-2.55037217513312,9.66931237308562));
#55929=CARTESIAN_POINT('Ctrl Pts',(-21.471671403753,-2.55832628412853,9.63791697607945));
#55930=CARTESIAN_POINT('Ctrl Pts',(-21.4424150110746,-2.56959157653279,
9.60464841257371));
#55931=CARTESIAN_POINT('Ctrl Pts',(-21.2909879716447,-2.63587850947504,
9.42991855559593));
#55932=CARTESIAN_POINT('Ctrl Pts',(-21.1630186724946,-2.71837825362579,
9.27335939831321));
#55933=CARTESIAN_POINT('Ctrl Pts',(-21.,-2.77045032493322,9.08705700417233));
#55934=CARTESIAN_POINT('Origin',(-50.,0.,0.));
#55935=CARTESIAN_POINT('',(-50.,-3.75038736519794,6.13145585166881));
#55936=CARTESIAN_POINT('Ctrl Pts',(-50.,-6.6617400018565,8.24507247679879));
#55937=CARTESIAN_POINT('Ctrl Pts',(-21.,-6.6617400018565,8.24507247679879));
#55938=CARTESIAN_POINT('Ctrl Pts',(-50.,-6.63837938775657,8.24010262588657));
#55939=CARTESIAN_POINT('Ctrl Pts',(-21.,-6.63837938775657,8.24010262588657));
#55940=CARTESIAN_POINT('Ctrl Pts',(-50.,-6.59177764993375,8.2299772134607));
#55941=CARTESIAN_POINT('Ctrl Pts',(-21.,-6.59177764993375,8.2299772134607));
#55942=CARTESIAN_POINT('Ctrl Pts',(-50.,-6.52223351516926,8.21423196280605));
#55943=CARTESIAN_POINT('Ctrl Pts',(-21.,-6.52223351516926,8.21423196280605));
#55944=CARTESIAN_POINT('Ctrl Pts',(-50.,-6.43022589217209,8.1921225513));
#55945=CARTESIAN_POINT('Ctrl Pts',(-21.,-6.43022589217209,8.1921225513));
#55946=CARTESIAN_POINT('Ctrl Pts',(-50.,-6.31642365942377,8.16261538830187));
#55947=CARTESIAN_POINT('Ctrl Pts',(-21.,-6.31642365942377,8.16261538830187));
#55948=CARTESIAN_POINT('Ctrl Pts',(-50.,-6.20385140809547,8.1312203551374));
#55949=CARTESIAN_POINT('Ctrl Pts',(-21.,-6.20385140809547,8.1312203551374));
#55950=CARTESIAN_POINT('Ctrl Pts',(-50.,-6.09254749437728,8.0979137913074));
#55951=CARTESIAN_POINT('Ctrl Pts',(-21.,-6.09254749437728,8.0979137913074));
#55952=CARTESIAN_POINT('Ctrl Pts',(-50.,-5.9825687506924,8.06266677783295));
#55953=CARTESIAN_POINT('Ctrl Pts',(-21.,-5.9825687506924,8.06266677783295));
#55954=CARTESIAN_POINT('Ctrl Pts',(-50.,-5.87399565540877,8.02544535222689));
#55955=CARTESIAN_POINT('Ctrl Pts',(-21.,-5.87399565540877,8.02544535222689));
#55956=CARTESIAN_POINT('Ctrl Pts',(-50.,-5.7669227832391,7.98621594320599));
#55957=CARTESIAN_POINT('Ctrl Pts',(-21.,-5.7669227832391,7.98621594320599));
#55958=CARTESIAN_POINT('Ctrl Pts',(-50.,-5.66144582368073,7.94495188520329));
#55959=CARTESIAN_POINT('Ctrl Pts',(-21.,-5.66144582368073,7.94495188520329));
#55960=CARTESIAN_POINT('Ctrl Pts',(-50.,-5.5576484178972,7.90164067817667));
#55961=CARTESIAN_POINT('Ctrl Pts',(-21.,-5.5576484178972,7.90164067817667));
#55962=CARTESIAN_POINT('Ctrl Pts',(-50.,-5.45559153104423,7.85628931405591));
#55963=CARTESIAN_POINT('Ctrl Pts',(-21.,-5.45559153104423,7.85628931405591));
#55964=CARTESIAN_POINT('Ctrl Pts',(-50.,-5.35529468870783,7.80893560674388));
#55965=CARTESIAN_POINT('Ctrl Pts',(-21.,-5.35529468870783,7.80893560674388));
#55966=CARTESIAN_POINT('Ctrl Pts',(-50.,-5.25675269887972,7.75963419345371));
#55967=CARTESIAN_POINT('Ctrl Pts',(-21.,-5.25675269887972,7.75963419345371));
#55968=CARTESIAN_POINT('Ctrl Pts',(-50.,-5.15997145275563,7.70842918324715));
#55969=CARTESIAN_POINT('Ctrl Pts',(-21.,-5.15997145275563,7.70842918324715));
#55970=CARTESIAN_POINT('Ctrl Pts',(-50.,-5.06499955030094,7.65532943098672));
#55971=CARTESIAN_POINT('Ctrl Pts',(-21.,-5.06499955030094,7.65532943098672));
#55972=CARTESIAN_POINT('Ctrl Pts',(-50.,-4.9719575030537,7.60028648840776));
#55973=CARTESIAN_POINT('Ctrl Pts',(-21.,-4.9719575030537,7.60028648840776));
#55974=CARTESIAN_POINT('Ctrl Pts',(-50.,-4.88107836846757,7.54316218647348));
#55975=CARTESIAN_POINT('Ctrl Pts',(-21.,-4.88107836846757,7.54316218647348));
#55976=CARTESIAN_POINT('Ctrl Pts',(-50.,-4.79269894740031,7.48374039375355));
#55977=CARTESIAN_POINT('Ctrl Pts',(-21.,-4.79269894740031,7.48374039375355));
#55978=CARTESIAN_POINT('Ctrl Pts',(-50.,-4.70721371156899,7.42177134000892));
#55979=CARTESIAN_POINT('Ctrl Pts',(-21.,-4.70721371156899,7.42177134000892));
#55980=CARTESIAN_POINT('Ctrl Pts',(-50.,-4.62503998887083,7.35700721943171));
#55981=CARTESIAN_POINT('Ctrl Pts',(-21.,-4.62503998887083,7.35700721943171));
#55982=CARTESIAN_POINT('Ctrl Pts',(-50.,-4.54657777868016,7.28923990788708));
#55983=CARTESIAN_POINT('Ctrl Pts',(-21.,-4.54657777868016,7.28923990788708));
#55984=CARTESIAN_POINT('Ctrl Pts',(-50.,-4.47217290162416,7.21834255288981));
#55985=CARTESIAN_POINT('Ctrl Pts',(-21.,-4.47217290162416,7.21834255288981));
#55986=CARTESIAN_POINT('Ctrl Pts',(-50.,-4.40207217433237,7.14429034032177));
#55987=CARTESIAN_POINT('Ctrl Pts',(-21.,-4.40207217433237,7.14429034032177));
#55988=CARTESIAN_POINT('Ctrl Pts',(-50.,-4.33637651734857,7.06716577496009));
#55989=CARTESIAN_POINT('Ctrl Pts',(-21.,-4.33637651734857,7.06716577496009));
#55990=CARTESIAN_POINT('Ctrl Pts',(-50.,-4.27498923356982,6.98717136730191));
#55991=CARTESIAN_POINT('Ctrl Pts',(-21.,-4.27498923356982,6.98717136730191));
#55992=CARTESIAN_POINT('Ctrl Pts',(-50.,-4.21757413484033,6.90463617300865));
#55993=CARTESIAN_POINT('Ctrl Pts',(-21.,-4.21757413484033,6.90463617300865));
#55994=CARTESIAN_POINT('Ctrl Pts',(-50.,-4.16348379256721,6.82003644526658));
#55995=CARTESIAN_POINT('Ctrl Pts',(-21.,-4.16348379256721,6.82003644526658));
#55996=CARTESIAN_POINT('Ctrl Pts',(-50.,-4.11183783259628,6.73395053478792));
#55997=CARTESIAN_POINT('Ctrl Pts',(-21.,-4.11183783259628,6.73395053478792));
#55998=CARTESIAN_POINT('Ctrl Pts',(-50.,-4.06165666819706,6.64698999124062));
#55999=CARTESIAN_POINT('Ctrl Pts',(-21.,-4.06165666819706,6.64698999124062));
#56000=CARTESIAN_POINT('Ctrl Pts',(-50.,-4.01197889710939,6.55973735411151));
#56001=CARTESIAN_POINT('Ctrl Pts',(-21.,-4.01197889710939,6.55973735411151));
#56002=CARTESIAN_POINT('Ctrl Pts',(-50.,-3.96197913233089,6.47268455970493));
#56003=CARTESIAN_POINT('Ctrl Pts',(-21.,-3.96197913233089,6.47268455970493));
#56004=CARTESIAN_POINT('Ctrl Pts',(-50.,-3.91110213900011,6.38616193008433));
#56005=CARTESIAN_POINT('Ctrl Pts',(-21.,-3.91110213900011,6.38616193008433));
#56006=CARTESIAN_POINT('Ctrl Pts',(-50.,-3.859023878729,6.30036238594766));
#56007=CARTESIAN_POINT('Ctrl Pts',(-21.,-3.859023878729,6.30036238594766));
#56008=CARTESIAN_POINT('Ctrl Pts',(-50.,-3.81627329006595,6.23237673886416));
#56009=CARTESIAN_POINT('Ctrl Pts',(-21.,-3.81627329006595,6.23237673886416));
#56010=CARTESIAN_POINT('Ctrl Pts',(-50.,-3.78357651403939,6.1817683663582));
#56011=CARTESIAN_POINT('Ctrl Pts',(-21.,-3.78357651403939,6.1817683663582));
#56012=CARTESIAN_POINT('Ctrl Pts',(-50.,-3.7614973065729,6.1481985134482));
#56013=CARTESIAN_POINT('Ctrl Pts',(-21.,-3.7614973065729,6.1481985134482));
#56014=CARTESIAN_POINT('Ctrl Pts',(-50.,-3.75038736519793,6.13145585166881));
#56015=CARTESIAN_POINT('Ctrl Pts',(-21.,-3.75038736519793,6.13145585166881));
#56016=CARTESIAN_POINT('',(-21.5,-5.93712762672243,8.04677050399782));
#56017=CARTESIAN_POINT('Ctrl Pts',(-21.5,-5.93712762672243,8.04677050399782));
#56018=CARTESIAN_POINT('Ctrl Pts',(-26.3333333333333,-5.93712762672243,
8.04677050399782));
#56019=CARTESIAN_POINT('Ctrl Pts',(-31.1666666666667,-5.93712762672243,
8.04677050399782));
#56020=CARTESIAN_POINT('Ctrl Pts',(-40.6666666666667,-5.93712762672243,
8.04677050399782));
#56021=CARTESIAN_POINT('Ctrl Pts',(-45.3333333333333,-5.93712762672243,
8.04677050399782));
#56022=CARTESIAN_POINT('Ctrl Pts',(-50.,-5.93712762672243,8.04677050399782));
#56023=CARTESIAN_POINT('Ctrl Pts',(-21.,-5.38825861761966,7.82410819644306));
#56024=CARTESIAN_POINT('Ctrl Pts',(-21.1171767610869,-5.5103250680882,7.88231976704395));
#56025=CARTESIAN_POINT('Ctrl Pts',(-21.2874825276357,-5.69235044790141,
7.96327099664389));
#56026=CARTESIAN_POINT('Ctrl Pts',(-21.5,-5.93712762672243,8.04677050399782));
#56027=CARTESIAN_POINT('Origin',(-35.75,0.,0.));
#56028=CARTESIAN_POINT('',(-21.5,-1.85780428234483,9.82591284555797));
#56029=CARTESIAN_POINT('Origin',(-21.5,0.,0.));
#56030=CARTESIAN_POINT('Ctrl Pts',(-21.5,-1.85780428234483,9.82591284555797));
#56031=CARTESIAN_POINT('Ctrl Pts',(-26.3333333333333,-1.85780428234483,
9.82591284555797));
#56032=CARTESIAN_POINT('Ctrl Pts',(-31.1666666666667,-1.85780428234483,
9.82591284555797));
#56033=CARTESIAN_POINT('Ctrl Pts',(-40.6666666666667,-1.85780428234483,
9.82591284555797));
#56034=CARTESIAN_POINT('Ctrl Pts',(-45.3333333333333,-1.85780428234483,
9.82591284555798));
#56035=CARTESIAN_POINT('Ctrl Pts',(-50.,-1.85780428234483,9.82591284555798));
#56036=CARTESIAN_POINT('Origin',(-21.25,0.,0.));
#56037=CARTESIAN_POINT('Ctrl Pts',(-21.,-1.45989994714919,9.38715570044056));
#56038=CARTESIAN_POINT('Ctrl Pts',(-21.1708653764906,-1.58343885080689,
9.54086217807701));
#56039=CARTESIAN_POINT('Ctrl Pts',(-21.3372400311872,-1.71664935045818,
9.68695766931578));
#56040=CARTESIAN_POINT('Ctrl Pts',(-21.5,-1.85780428234483,9.82591284555798));
#56041=CARTESIAN_POINT('Ctrl Pts',(-50.,-2.42461747220419,10.3189742762293));
#56042=CARTESIAN_POINT('Ctrl Pts',(-21.,-2.42461747220419,10.3189742762293));
#56043=CARTESIAN_POINT('Ctrl Pts',(-50.,-2.40572662366171,10.3043608046855));
#56044=CARTESIAN_POINT('Ctrl Pts',(-21.,-2.40572662366171,10.3043608046855));
#56045=CARTESIAN_POINT('Ctrl Pts',(-50.,-2.36813316049665,10.2750183870592));
#56046=CARTESIAN_POINT('Ctrl Pts',(-21.,-2.36813316049665,10.2750183870592));
#56047=CARTESIAN_POINT('Ctrl Pts',(-50.,-2.31230766835601,10.2306583371767));
#56048=CARTESIAN_POINT('Ctrl Pts',(-21.,-2.31230766835601,10.2306583371767));
#56049=CARTESIAN_POINT('Ctrl Pts',(-50.,-2.2390045785598,10.1708178342288));
#56050=CARTESIAN_POINT('Ctrl Pts',(-21.,-2.2390045785598,10.1708178342288));
#56051=CARTESIAN_POINT('Ctrl Pts',(-50.,-2.14927498796815,10.0948558607226));
#56052=CARTESIAN_POINT('Ctrl Pts',(-21.,-2.14927498796815,10.0948558607226));
#56053=CARTESIAN_POINT('Ctrl Pts',(-50.,-2.0614726885108,10.0177266439074));
#56054=CARTESIAN_POINT('Ctrl Pts',(-21.,-2.0614726885108,10.0177266439074));
#56055=CARTESIAN_POINT('Ctrl Pts',(-50.,-1.97564250382673,9.93942550853734));
#56056=CARTESIAN_POINT('Ctrl Pts',(-21.,-1.97564250382673,9.93942550853734));
#56057=CARTESIAN_POINT('Ctrl Pts',(-50.,-1.89184818563464,9.85995105817688));
#56058=CARTESIAN_POINT('Ctrl Pts',(-21.,-1.89184818563464,9.85995105817688));
#56059=CARTESIAN_POINT('Ctrl Pts',(-50.,-1.81017697820954,9.77930761193764));
#56060=CARTESIAN_POINT('Ctrl Pts',(-21.,-1.81017697820954,9.77930761193764));
#56061=CARTESIAN_POINT('Ctrl Pts',(-50.,-1.73072865645713,9.69750595756857));
#56062=CARTESIAN_POINT('Ctrl Pts',(-21.,-1.73072865645713,9.69750595756857));
#56063=CARTESIAN_POINT('Ctrl Pts',(-50.,-1.65360100339141,9.61456358834088));
#56064=CARTESIAN_POINT('Ctrl Pts',(-21.,-1.65360100339141,9.61456358834088));
#56065=CARTESIAN_POINT('Ctrl Pts',(-50.,-1.57887480066182,9.53050553264656));
#56066=CARTESIAN_POINT('Ctrl Pts',(-21.,-1.57887480066182,9.53050553264656));
#56067=CARTESIAN_POINT('Ctrl Pts',(-50.,-1.50660194229105,9.44536454178638));
#56068=CARTESIAN_POINT('Ctrl Pts',(-21.,-1.50660194229105,9.44536454178638));
#56069=CARTESIAN_POINT('Ctrl Pts',(-50.,-1.43678361338666,9.35918315674388));
#56070=CARTESIAN_POINT('Ctrl Pts',(-21.,-1.43678361338666,9.35918315674388));
#56071=CARTESIAN_POINT('Ctrl Pts',(-50.,-1.3693914299125,9.27200835121914));
#56072=CARTESIAN_POINT('Ctrl Pts',(-21.,-1.3693914299125,9.27200835121914));
#56073=CARTESIAN_POINT('Ctrl Pts',(-50.,-1.30441156144786,9.18388242219763));
#56074=CARTESIAN_POINT('Ctrl Pts',(-21.,-1.30441156144786,9.18388242219763));
#56075=CARTESIAN_POINT('Ctrl Pts',(-50.,-1.24188395306769,9.09483443436949));
#56076=CARTESIAN_POINT('Ctrl Pts',(-21.,-1.24188395306769,9.09483443436949));
#56077=CARTESIAN_POINT('Ctrl Pts',(-50.,-1.18193820283021,9.00487302535333));
#56078=CARTESIAN_POINT('Ctrl Pts',(-21.,-1.18193820283021,9.00487302535333));
#56079=CARTESIAN_POINT('Ctrl Pts',(-50.,-1.12484423754393,8.91397482898789));
#56080=CARTESIAN_POINT('Ctrl Pts',(-21.,-1.12484423754393,8.91397482898789));
#56081=CARTESIAN_POINT('Ctrl Pts',(-50.,-1.07099928020948,8.82209124999857));
#56082=CARTESIAN_POINT('Ctrl Pts',(-21.,-1.07099928020948,8.82209124999857));
#56083=CARTESIAN_POINT('Ctrl Pts',(-50.,-1.02086710880846,8.72916840803945));
#56084=CARTESIAN_POINT('Ctrl Pts',(-21.,-1.02086710880846,8.72916840803945));
#56085=CARTESIAN_POINT('Ctrl Pts',(-50.,-0.974931241694467,8.63516410958082));
#56086=CARTESIAN_POINT('Ctrl Pts',(-21.,-0.974931241694467,8.63516410958082));
#56087=CARTESIAN_POINT('Ctrl Pts',(-50.,-0.933642367528788,8.5400643944807));
#56088=CARTESIAN_POINT('Ctrl Pts',(-21.,-0.933642367528788,8.5400643944807));
#56089=CARTESIAN_POINT('Ctrl Pts',(-50.,-0.897367099160985,8.4439050185459));
#56090=CARTESIAN_POINT('Ctrl Pts',(-21.,-0.897367099160985,8.4439050185459));
#56091=CARTESIAN_POINT('Ctrl Pts',(-50.,-0.86633857713272,8.34677071475058));
#56092=CARTESIAN_POINT('Ctrl Pts',(-21.,-0.86633857713272,8.34677071475058));
#56093=CARTESIAN_POINT('Ctrl Pts',(-50.,-0.840611930230858,8.24877960511329));
#56094=CARTESIAN_POINT('Ctrl Pts',(-21.,-0.840611930230858,8.24877960511329));
#56095=CARTESIAN_POINT('Ctrl Pts',(-50.,-0.82001217136434,8.15007218998677));
#56096=CARTESIAN_POINT('Ctrl Pts',(-21.,-0.82001217136434,8.15007218998677));
#56097=CARTESIAN_POINT('Ctrl Pts',(-50.,-0.804093633570273,8.05079907170372));
#56098=CARTESIAN_POINT('Ctrl Pts',(-21.,-0.804093633570273,8.05079907170372));
#56099=CARTESIAN_POINT('Ctrl Pts',(-50.,-0.792066365329069,7.95110843081948));
#56100=CARTESIAN_POINT('Ctrl Pts',(-21.,-0.792066365329069,7.95110843081948));
#56101=CARTESIAN_POINT('Ctrl Pts',(-50.,-0.782886239966145,7.85113936329068));
#56102=CARTESIAN_POINT('Ctrl Pts',(-21.,-0.782886239966145,7.85113936329068));
#56103=CARTESIAN_POINT('Ctrl Pts',(-50.,-0.775405338877351,7.75101782957587));
#56104=CARTESIAN_POINT('Ctrl Pts',(-21.,-0.775405338877351,7.75101782957587));
#56105=CARTESIAN_POINT('Ctrl Pts',(-50.,-0.768504714146027,7.65085154280962));
#56106=CARTESIAN_POINT('Ctrl Pts',(-21.,-0.768504714146027,7.65085154280962));
#56107=CARTESIAN_POINT('Ctrl Pts',(-50.,-0.761227274615912,7.55072560028829));
#56108=CARTESIAN_POINT('Ctrl Pts',(-21.,-0.761227274615912,7.55072560028829));
#56109=CARTESIAN_POINT('Ctrl Pts',(-50.,-0.752929449590466,7.45069670452966));
#56110=CARTESIAN_POINT('Ctrl Pts',(-21.,-0.752929449590466,7.45069670452966));
#56111=CARTESIAN_POINT('Ctrl Pts',(-50.,-0.743235585416284,7.35079807608913));
#56112=CARTESIAN_POINT('Ctrl Pts',(-21.,-0.743235585416284,7.35079807608913));
#56113=CARTESIAN_POINT('Ctrl Pts',(-50.,-0.734216502709279,7.2709963393441));
#56114=CARTESIAN_POINT('Ctrl Pts',(-21.,-0.734216502709279,7.2709963393441));
#56115=CARTESIAN_POINT('Ctrl Pts',(-50.,-0.726715875322121,7.21121317182152));
#56116=CARTESIAN_POINT('Ctrl Pts',(-21.,-0.726715875322121,7.21121317182152));
#56117=CARTESIAN_POINT('Ctrl Pts',(-50.,-0.721388610069065,7.17138797035723));
#56118=CARTESIAN_POINT('Ctrl Pts',(-21.,-0.721388610069065,7.17138797035723));
#56119=CARTESIAN_POINT('Ctrl Pts',(-50.,-0.718643267461623,7.15148293042304));
#56120=CARTESIAN_POINT('Ctrl Pts',(-21.,-0.718643267461623,7.15148293042304));
#56121=CARTESIAN_POINT('',(-50.,-0.718643267461628,7.15148293042304));
#56122=CARTESIAN_POINT('Origin',(-50.,0.,0.));
#56123=CARTESIAN_POINT('',(-50.,0.718643267461623,7.15148293042304));
#56124=CARTESIAN_POINT('Ctrl Pts',(-50.,0.718643267461623,7.15148293042304));
#56125=CARTESIAN_POINT('Ctrl Pts',(-21.,0.718643267461623,7.15148293042304));
#56126=CARTESIAN_POINT('Ctrl Pts',(-50.,0.721647166649911,7.17509214524366));
#56127=CARTESIAN_POINT('Ctrl Pts',(-21.,0.721647166649911,7.17509214524366));
#56128=CARTESIAN_POINT('Ctrl Pts',(-50.,0.72749213560466,7.22233768688913));
#56129=CARTESIAN_POINT('Ctrl Pts',(-21.,0.72749213560466,7.22233768688913));
#56130=CARTESIAN_POINT('Ctrl Pts',(-50.,0.735771087779772,7.29328733826105));
#56131=CARTESIAN_POINT('Ctrl Pts',(-21.,0.735771087779772,7.29328733826105));
#56132=CARTESIAN_POINT('Ctrl Pts',(-50.,0.745831500234843,7.38804974272502));
#56133=CARTESIAN_POINT('Ctrl Pts',(-21.,0.745831500234843,7.38804974272502));
#56134=CARTESIAN_POINT('Ctrl Pts',(-50.,0.756870878958096,7.5067579169994));
#56135=CARTESIAN_POINT('Ctrl Pts',(-21.,0.756870878958096,7.5067579169994));
#56136=CARTESIAN_POINT('Ctrl Pts',(-50.,0.766672302003445,7.62566969516693));
#56137=CARTESIAN_POINT('Ctrl Pts',(-21.,0.766672302003445,7.62566969516693));
#56138=CARTESIAN_POINT('Ctrl Pts',(-50.,0.775839563797132,7.74468091618948));
#56139=CARTESIAN_POINT('Ctrl Pts',(-21.,0.775839563797132,7.74468091618948));
#56140=CARTESIAN_POINT('Ctrl Pts',(-50.,0.785400272847098,7.86361381479518));
#56141=CARTESIAN_POINT('Ctrl Pts',(-21.,0.785400272847098,7.86361381479518));
#56142=CARTESIAN_POINT('Ctrl Pts',(-50.,0.796736942256154,7.98224460192821));
#56143=CARTESIAN_POINT('Ctrl Pts',(-21.,0.796736942256154,7.98224460192821));
#56144=CARTESIAN_POINT('Ctrl Pts',(-50.,0.811510144890448,8.10033651802127));
#56145=CARTESIAN_POINT('Ctrl Pts',(-21.,0.811510144890448,8.10033651802127));
#56146=CARTESIAN_POINT('Ctrl Pts',(-50.,0.831570515383446,8.21766862525226));
#56147=CARTESIAN_POINT('Ctrl Pts',(-21.,0.831570515383446,8.21766862525226));
#56148=CARTESIAN_POINT('Ctrl Pts',(-50.,0.858916682261844,8.33407215281038));
#56149=CARTESIAN_POINT('Ctrl Pts',(-21.,0.858916682261844,8.33407215281038));
#56150=CARTESIAN_POINT('Ctrl Pts',(-50.,0.895240742652423,8.44941362598824));
#56151=CARTESIAN_POINT('Ctrl Pts',(-21.,0.895240742652423,8.44941362598824));
#56152=CARTESIAN_POINT('Ctrl Pts',(-50.,0.941323460369316,8.56356426545847));
#56153=CARTESIAN_POINT('Ctrl Pts',(-21.,0.941323460369316,8.56356426545847));
#56154=CARTESIAN_POINT('Ctrl Pts',(-50.,0.996589197042052,8.67637972666424));
#56155=CARTESIAN_POINT('Ctrl Pts',(-21.,0.996589197042052,8.67637972666424));
#56156=CARTESIAN_POINT('Ctrl Pts',(-50.,1.05830577327405,8.78766206238304));
#56157=CARTESIAN_POINT('Ctrl Pts',(-21.,1.05830577327405,8.78766206238304));
#56158=CARTESIAN_POINT('Ctrl Pts',(-50.,1.12259642171968,8.89721129760285));
#56159=CARTESIAN_POINT('Ctrl Pts',(-21.,1.12259642171968,8.89721129760285));
#56160=CARTESIAN_POINT('Ctrl Pts',(-50.,1.18634328973517,9.00492385207762));
#56161=CARTESIAN_POINT('Ctrl Pts',(-21.,1.18634328973517,9.00492385207762));
#56162=CARTESIAN_POINT('Ctrl Pts',(-50.,1.24851405668088,9.11085713692575));
#56163=CARTESIAN_POINT('Ctrl Pts',(-21.,1.24851405668088,9.11085713692575));
#56164=CARTESIAN_POINT('Ctrl Pts',(-50.,1.31242393260393,9.21535483920498));
#56165=CARTESIAN_POINT('Ctrl Pts',(-21.,1.31242393260393,9.21535483920498));
#56166=CARTESIAN_POINT('Ctrl Pts',(-50.,1.38484298036779,9.31896299195203));
#56167=CARTESIAN_POINT('Ctrl Pts',(-21.,1.38484298036779,9.31896299195203));
#56168=CARTESIAN_POINT('Ctrl Pts',(-50.,1.47203331296336,9.42213951575228));
#56169=CARTESIAN_POINT('Ctrl Pts',(-21.,1.47203331296336,9.42213951575228));
#56170=CARTESIAN_POINT('Ctrl Pts',(-50.,1.576861582378,9.52503847397034));
#56171=CARTESIAN_POINT('Ctrl Pts',(-21.,1.576861582378,9.52503847397034));
#56172=CARTESIAN_POINT('Ctrl Pts',(-50.,1.69493509590243,9.62722202065427));
#56173=CARTESIAN_POINT('Ctrl Pts',(-21.,1.69493509590243,9.62722202065427));
#56174=CARTESIAN_POINT('Ctrl Pts',(-50.,1.81273846192755,9.72752627760495));
#56175=CARTESIAN_POINT('Ctrl Pts',(-21.,1.81273846192755,9.72752627760495));
#56176=CARTESIAN_POINT('Ctrl Pts',(-50.,1.91151183055746,9.82437388645964));
#56177=CARTESIAN_POINT('Ctrl Pts',(-21.,1.91151183055746,9.82437388645964));
#56178=CARTESIAN_POINT('Ctrl Pts',(-50.,1.97016627452818,9.91601178835393));
#56179=CARTESIAN_POINT('Ctrl Pts',(-21.,1.97016627452818,9.91601178835393));
#56180=CARTESIAN_POINT('Ctrl Pts',(-50.,1.96848522037066,10.0007711148064));
#56181=CARTESIAN_POINT('Ctrl Pts',(-21.,1.96848522037066,10.0007711148064));
#56182=CARTESIAN_POINT('Ctrl Pts',(-50.,1.89041053749867,10.0773349427117));
#56183=CARTESIAN_POINT('Ctrl Pts',(-21.,1.89041053749867,10.0773349427117));
#56184=CARTESIAN_POINT('Ctrl Pts',(-50.,1.72372501438528,10.1447096468161));
#56185=CARTESIAN_POINT('Ctrl Pts',(-21.,1.72372501438528,10.1447096468161));
#56186=CARTESIAN_POINT('Ctrl Pts',(-50.,1.45943182294451,10.2021716552068));
#56187=CARTESIAN_POINT('Ctrl Pts',(-21.,1.45943182294451,10.2021716552068));
#56188=CARTESIAN_POINT('Ctrl Pts',(-50.,1.09127335261449,10.2492257884407));
#56189=CARTESIAN_POINT('Ctrl Pts',(-21.,1.09127335261449,10.2492257884407));
#56190=CARTESIAN_POINT('Ctrl Pts',(-50.,0.615218622302491,10.285561208657));
#56191=CARTESIAN_POINT('Ctrl Pts',(-21.,0.615218622302491,10.285561208657));
#56192=CARTESIAN_POINT('Ctrl Pts',(-50.,0.0289898802580638,10.3110107412798));
#56193=CARTESIAN_POINT('Ctrl Pts',(-21.,0.0289898802580638,10.3110107412798));
#56194=CARTESIAN_POINT('Ctrl Pts',(-50.,-0.668404184972711,10.3255108965746));
#56195=CARTESIAN_POINT('Ctrl Pts',(-21.,-0.668404184972711,10.3255108965746));
#56196=CARTESIAN_POINT('Ctrl Pts',(-50.,-1.31537435394882,10.3283530123025));
#56197=CARTESIAN_POINT('Ctrl Pts',(-21.,-1.31537435394882,10.3283530123025));
#56198=CARTESIAN_POINT('Ctrl Pts',(-50.,-1.85058421429603,10.3255716832032));
#56199=CARTESIAN_POINT('Ctrl Pts',(-21.,-1.85058421429603,10.3255716832032));
#56200=CARTESIAN_POINT('Ctrl Pts',(-50.,-2.22957558565152,10.3215368479529));
#56201=CARTESIAN_POINT('Ctrl Pts',(-21.,-2.22957558565152,10.3215368479529));
#56202=CARTESIAN_POINT('Ctrl Pts',(-50.,-2.42461747220419,10.3189742762293));
#56203=CARTESIAN_POINT('Ctrl Pts',(-21.,-2.42461747220419,10.3189742762293));
#56204=CARTESIAN_POINT('',(-21.5,1.89755147577054,9.81831443766195));
#56205=CARTESIAN_POINT('Ctrl Pts',(-21.5,1.89755147577054,9.81831443766194));
#56206=CARTESIAN_POINT('Ctrl Pts',(-21.47032468389,1.87577485631896,9.79229867840465));
#56207=CARTESIAN_POINT('Ctrl Pts',(-21.4396140182577,1.84982079175808,9.76599200484083));
#56208=CARTESIAN_POINT('Ctrl Pts',(-21.2876118590982,1.71298536184934,9.63694998390189));
#56209=CARTESIAN_POINT('Ctrl Pts',(-21.1610241576491,1.57282267908252,9.53269100720219));
#56210=CARTESIAN_POINT('Ctrl Pts',(-21.,1.44663677770971,9.38920880763537));
#56211=CARTESIAN_POINT('Ctrl Pts',(-50.,1.89755147577054,9.81831443766195));
#56212=CARTESIAN_POINT('Ctrl Pts',(-45.1666666666667,1.89755147577054,9.81831443766195));
#56213=CARTESIAN_POINT('Ctrl Pts',(-40.3333333333333,1.89755147577054,9.81831443766195));
#56214=CARTESIAN_POINT('Ctrl Pts',(-30.8333333333333,1.89755147577054,9.81831443766195));
#56215=CARTESIAN_POINT('Ctrl Pts',(-26.1666666666667,1.89755147577054,9.81831443766195));
#56216=CARTESIAN_POINT('Ctrl Pts',(-21.5,1.89755147577054,9.81831443766195));
#56217=CARTESIAN_POINT('Origin',(-21.25,0.,0.));
#56218=CARTESIAN_POINT('Origin',(-21.5,0.,0.));
#56219=CARTESIAN_POINT('Origin',(-35.75,0.,0.));
#56220=CARTESIAN_POINT('Ctrl Pts',(-50.,3.75038736519793,6.13145585166881));
#56221=CARTESIAN_POINT('Ctrl Pts',(-21.,3.75038736519793,6.13145585166881));
#56222=CARTESIAN_POINT('Ctrl Pts',(-50.,3.7633374392529,6.15142367620606));
#56223=CARTESIAN_POINT('Ctrl Pts',(-21.,3.7633374392529,6.15142367620606));
#56224=CARTESIAN_POINT('Ctrl Pts',(-50.,3.78910264658076,6.19145440139071));
#56225=CARTESIAN_POINT('Ctrl Pts',(-21.,3.78910264658076,6.19145440139071));
#56226=CARTESIAN_POINT('Ctrl Pts',(-50.,3.82734562477572,6.25178572573963));
#56227=CARTESIAN_POINT('Ctrl Pts',(-21.,3.82734562477572,6.25178572573963));
#56228=CARTESIAN_POINT('Ctrl Pts',(-50.,3.87752560957259,6.33279865263617));
#56229=CARTESIAN_POINT('Ctrl Pts',(-21.,3.87752560957259,6.33279865263617));
#56230=CARTESIAN_POINT('Ctrl Pts',(-50.,3.93897729264122,6.43496121510494));
#56231=CARTESIAN_POINT('Ctrl Pts',(-21.,3.93897729264122,6.43496121510494));
#56232=CARTESIAN_POINT('Ctrl Pts',(-50.,3.99940195660266,6.53784434718121));
#56233=CARTESIAN_POINT('Ctrl Pts',(-21.,3.99940195660266,6.53784434718121));
#56234=CARTESIAN_POINT('Ctrl Pts',(-50.,4.05929840765689,6.64109222642907));
#56235=CARTESIAN_POINT('Ctrl Pts',(-21.,4.05929840765689,6.64109222642907));
#56236=CARTESIAN_POINT('Ctrl Pts',(-50.,4.11951535961712,6.74409882925098));
#56237=CARTESIAN_POINT('Ctrl Pts',(-21.,4.11951535961712,6.74409882925098));
#56238=CARTESIAN_POINT('Ctrl Pts',(-50.,4.18120131531612,6.84606267872027));
#56239=CARTESIAN_POINT('Ctrl Pts',(-21.,4.18120131531612,6.84606267872027));
#56240=CARTESIAN_POINT('Ctrl Pts',(-50.,4.24574967308284,6.94604996627335));
#56241=CARTESIAN_POINT('Ctrl Pts',(-21.,4.24574967308284,6.94604996627335));
#56242=CARTESIAN_POINT('Ctrl Pts',(-50.,4.31473193577955,7.04305867353628));
#56243=CARTESIAN_POINT('Ctrl Pts',(-21.,4.31473193577955,7.04305867353628));
#56244=CARTESIAN_POINT('Ctrl Pts',(-50.,4.38987557857684,7.13606957084443));
#56245=CARTESIAN_POINT('Ctrl Pts',(-21.,4.38987557857684,7.13606957084443));
#56246=CARTESIAN_POINT('Ctrl Pts',(-50.,4.4726472158023,7.22422822821349));
#56247=CARTESIAN_POINT('Ctrl Pts',(-21.,4.4726472158023,7.22422822821349));
#56248=CARTESIAN_POINT('Ctrl Pts',(-50.,4.56369441608956,7.30707985875561));
#56249=CARTESIAN_POINT('Ctrl Pts',(-21.,4.56369441608956,7.30707985875561));
#56250=CARTESIAN_POINT('Ctrl Pts',(-50.,4.66243591843161,7.38474417264741));
#56251=CARTESIAN_POINT('Ctrl Pts',(-21.,4.66243591843161,7.38474417264741));
#56252=CARTESIAN_POINT('Ctrl Pts',(-50.,4.76632422816958,7.45822827381644));
#56253=CARTESIAN_POINT('Ctrl Pts',(-21.,4.76632422816958,7.45822827381644));
#56254=CARTESIAN_POINT('Ctrl Pts',(-50.,4.87177973271099,7.52903405731413));
#56255=CARTESIAN_POINT('Ctrl Pts',(-21.,4.87177973271099,7.52903405731413));
#56256=CARTESIAN_POINT('Ctrl Pts',(-50.,4.97594840210465,7.59842098612655));
#56257=CARTESIAN_POINT('Ctrl Pts',(-21.,4.97594840210465,7.59842098612655));
#56258=CARTESIAN_POINT('Ctrl Pts',(-50.,5.07792505734327,7.66688869302314));
#56259=CARTESIAN_POINT('Ctrl Pts',(-21.,5.07792505734327,7.66688869302314));
#56260=CARTESIAN_POINT('Ctrl Pts',(-50.,5.18084571969554,7.73330841361203));
#56261=CARTESIAN_POINT('Ctrl Pts',(-21.,5.18084571969554,7.73330841361203));
#56262=CARTESIAN_POINT('Ctrl Pts',(-50.,5.29104691989087,7.79523468647088));
#56263=CARTESIAN_POINT('Ctrl Pts',(-21.,5.29104691989087,7.79523468647088));
#56264=CARTESIAN_POINT('Ctrl Pts',(-50.,5.41436931107715,7.85036305479183));
#56265=CARTESIAN_POINT('Ctrl Pts',(-21.,5.41436931107715,7.85036305479183));
#56266=CARTESIAN_POINT('Ctrl Pts',(-50.,5.55346250303877,7.89758853118705));
#56267=CARTESIAN_POINT('Ctrl Pts',(-21.,5.55346250303877,7.89758853118705));
#56268=CARTESIAN_POINT('Ctrl Pts',(-50.,5.70417884215966,7.9384225480224));
#56269=CARTESIAN_POINT('Ctrl Pts',(-21.,5.70417884215966,7.9384225480224));
#56270=CARTESIAN_POINT('Ctrl Pts',(-50.,5.85383639353758,7.97768059592143));
#56271=CARTESIAN_POINT('Ctrl Pts',(-21.,5.85383639353758,7.97768059592143));
#56272=CARTESIAN_POINT('Ctrl Pts',(-50.,5.98484872630544,8.02208111792391));
#56273=CARTESIAN_POINT('Ctrl Pts',(-21.,5.98484872630544,8.02208111792391));
#56274=CARTESIAN_POINT('Ctrl Pts',(-50.,6.07745474980597,8.07919480518469));
#56275=CARTESIAN_POINT('Ctrl Pts',(-21.,6.07745474980597,8.07919480518469));
#56276=CARTESIAN_POINT('Ctrl Pts',(-50.,6.11271586583108,8.15628970164627));
#56277=CARTESIAN_POINT('Ctrl Pts',(-21.,6.11271586583108,8.15628970164627));
#56278=CARTESIAN_POINT('Ctrl Pts',(-50.,6.07559280712476,8.2591466623313));
#56279=CARTESIAN_POINT('Ctrl Pts',(-21.,6.07559280712476,8.2591466623313));
#56280=CARTESIAN_POINT('Ctrl Pts',(-50.,5.9546471286083,8.39217131123866));
#56281=CARTESIAN_POINT('Ctrl Pts',(-21.,5.9546471286083,8.39217131123866));
#56282=CARTESIAN_POINT('Ctrl Pts',(-50.,5.74145902217939,8.55861531001153));
#56283=CARTESIAN_POINT('Ctrl Pts',(-21.,5.74145902217939,8.55861531001153));
#56284=CARTESIAN_POINT('Ctrl Pts',(-50.,5.43017572522592,8.760747592856));
#56285=CARTESIAN_POINT('Ctrl Pts',(-21.,5.43017572522592,8.760747592856));
#56286=CARTESIAN_POINT('Ctrl Pts',(-50.,5.01703058178298,9.00003708168539));
#56287=CARTESIAN_POINT('Ctrl Pts',(-21.,5.01703058178298,9.00003708168539));
#56288=CARTESIAN_POINT('Ctrl Pts',(-50.,4.4998988741045,9.27732143685757));
#56289=CARTESIAN_POINT('Ctrl Pts',(-21.,4.4998988741045,9.27732143685757));
#56290=CARTESIAN_POINT('Ctrl Pts',(-50.,3.87785991426877,9.59297357001867));
#56291=CARTESIAN_POINT('Ctrl Pts',(-21.,3.87785991426877,9.59297357001867));
#56292=CARTESIAN_POINT('Ctrl Pts',(-50.,3.29619308135874,9.87624406382134));
#56293=CARTESIAN_POINT('Ctrl Pts',(-21.,3.29619308135874,9.87624406382134));
#56294=CARTESIAN_POINT('Ctrl Pts',(-50.,2.8127788859222,10.1059570283115));
#56295=CARTESIAN_POINT('Ctrl Pts',(-21.,2.8127788859222,10.1059570283115));
#56296=CARTESIAN_POINT('Ctrl Pts',(-50.,2.46956880972213,10.2667599606609));
#56297=CARTESIAN_POINT('Ctrl Pts',(-21.,2.46956880972213,10.2667599606609));
#56298=CARTESIAN_POINT('Ctrl Pts',(-50.,2.29273028380004,10.3490766663382));
#56299=CARTESIAN_POINT('Ctrl Pts',(-21.,2.29273028380004,10.3490766663382));
#56300=CARTESIAN_POINT('',(-21.5,5.96964178495622,8.0226789141349));
#56301=CARTESIAN_POINT('Ctrl Pts',(-50.,5.96964178495622,8.0226789141349));
#56302=CARTESIAN_POINT('Ctrl Pts',(-45.1666666666667,5.96964178495622,8.0226789141349));
#56303=CARTESIAN_POINT('Ctrl Pts',(-40.3333333333333,5.96964178495622,8.0226789141349));
#56304=CARTESIAN_POINT('Ctrl Pts',(-30.8333333333333,5.96964178495622,8.0226789141349));
#56305=CARTESIAN_POINT('Ctrl Pts',(-26.1666666666667,5.96964178495622,8.0226789141349));
#56306=CARTESIAN_POINT('Ctrl Pts',(-21.5,5.96964178495622,8.0226789141349));
#56307=CARTESIAN_POINT('',(-50.,3.75038736519793,6.13145585166881));
#56308=CARTESIAN_POINT('Ctrl Pts',(-21.5,5.96964178495622,8.0226789141349));
#56309=CARTESIAN_POINT('Ctrl Pts',(-21.471640009925,5.94010387156985,8.0093081760178));
#56310=CARTESIAN_POINT('Ctrl Pts',(-21.4423497933815,5.90702876507376,7.99736128679984));
#56311=CARTESIAN_POINT('Ctrl Pts',(-21.2909092331889,5.72905875838041,7.94024959050558));
#56312=CARTESIAN_POINT('Ctrl Pts',(-21.1629721875821,5.55527241504999,7.9071372002529));
#56313=CARTESIAN_POINT('Ctrl Pts',(-21.,5.37719972469147,7.83171265565699));
#56314=CARTESIAN_POINT('Origin',(-50.,0.,0.));
#56315=CARTESIAN_POINT('',(-50.,2.45543694297674,6.75507110762463));
#56316=CARTESIAN_POINT('Ctrl Pts',(-50.,2.29273028380004,10.3490766663382));
#56317=CARTESIAN_POINT('Ctrl Pts',(-21.,2.29273028380004,10.3490766663382));
#56318=CARTESIAN_POINT('Ctrl Pts',(-50.,2.30340980255016,10.3277139514246));
#56319=CARTESIAN_POINT('Ctrl Pts',(-21.,2.30340980255016,10.3277139514246));
#56320=CARTESIAN_POINT('Ctrl Pts',(-50.,2.32454914462406,10.2849661542698));
#56321=CARTESIAN_POINT('Ctrl Pts',(-21.,2.32454914462406,10.2849661542698));
#56322=CARTESIAN_POINT('Ctrl Pts',(-50.,2.35559907076766,10.2207773570791));
#56323=CARTESIAN_POINT('Ctrl Pts',(-21.,2.35559907076766,10.2207773570791));
#56324=CARTESIAN_POINT('Ctrl Pts',(-50.,2.39567905142538,10.1350579081937));
#56325=CARTESIAN_POINT('Ctrl Pts',(-21.,2.39567905142538,10.1350579081937));
#56326=CARTESIAN_POINT('Ctrl Pts',(-50.,2.44356395398246,10.0276863246448));
#56327=CARTESIAN_POINT('Ctrl Pts',(-21.,2.44356395398246,10.0276863246448));
#56328=CARTESIAN_POINT('Ctrl Pts',(-50.,2.48920597933682,9.92009931149698));
#56329=CARTESIAN_POINT('Ctrl Pts',(-21.,2.48920597933682,9.92009931149698));
#56330=CARTESIAN_POINT('Ctrl Pts',(-50.,2.53256271427195,9.81231210474723));
#56331=CARTESIAN_POINT('Ctrl Pts',(-21.,2.53256271427195,9.81231210474723));
#56332=CARTESIAN_POINT('Ctrl Pts',(-50.,2.57357611458342,9.70435110708481));
#56333=CARTESIAN_POINT('Ctrl Pts',(-21.,2.57357611458342,9.70435110708481));
#56334=CARTESIAN_POINT('Ctrl Pts',(-50.,2.61216944988784,9.59625806376705));
#56335=CARTESIAN_POINT('Ctrl Pts',(-21.,2.61216944988784,9.59625806376705));
#56336=CARTESIAN_POINT('Ctrl Pts',(-50.,2.64825750673019,9.48808598492904));
#56337=CARTESIAN_POINT('Ctrl Pts',(-21.,2.64825750673019,9.48808598492904));
#56338=CARTESIAN_POINT('Ctrl Pts',(-50.,2.68175977570501,9.37989305792331));
#56339=CARTESIAN_POINT('Ctrl Pts',(-21.,2.68175977570501,9.37989305792331));
#56340=CARTESIAN_POINT('Ctrl Pts',(-50.,2.71261433447332,9.27173688239595));
#56341=CARTESIAN_POINT('Ctrl Pts',(-21.,2.71261433447332,9.27173688239595));
#56342=CARTESIAN_POINT('Ctrl Pts',(-50.,2.74078863839312,9.16366948222194));
#56343=CARTESIAN_POINT('Ctrl Pts',(-21.,2.74078863839312,9.16366948222194));
#56344=CARTESIAN_POINT('Ctrl Pts',(-50.,2.76630007756038,9.05572969970197));
#56345=CARTESIAN_POINT('Ctrl Pts',(-21.,2.76630007756038,9.05572969970197));
#56346=CARTESIAN_POINT('Ctrl Pts',(-50.,2.78919460623265,8.94794754130566));
#56347=CARTESIAN_POINT('Ctrl Pts',(-21.,2.78919460623265,8.94794754130566));
#56348=CARTESIAN_POINT('Ctrl Pts',(-50.,2.80950303716262,8.84035511450549));
#56349=CARTESIAN_POINT('Ctrl Pts',(-21.,2.80950303716262,8.84035511450549));
#56350=CARTESIAN_POINT('Ctrl Pts',(-50.,2.82720199177778,8.73299593720093));
#56351=CARTESIAN_POINT('Ctrl Pts',(-21.,2.82720199177778,8.73299593720093));
#56352=CARTESIAN_POINT('Ctrl Pts',(-50.,2.84217845398458,8.62593402210748));
#56353=CARTESIAN_POINT('Ctrl Pts',(-21.,2.84217845398458,8.62593402210748));
#56354=CARTESIAN_POINT('Ctrl Pts',(-50.,2.85417908993455,8.51926543389428));
#56355=CARTESIAN_POINT('Ctrl Pts',(-21.,2.85417908993455,8.51926543389428));
#56356=CARTESIAN_POINT('Ctrl Pts',(-50.,2.86282492937103,8.41311873833255));
#56357=CARTESIAN_POINT('Ctrl Pts',(-21.,2.86282492937103,8.41311873833255));
#56358=CARTESIAN_POINT('Ctrl Pts',(-50.,2.86767474496505,8.30764661663281));
#56359=CARTESIAN_POINT('Ctrl Pts',(-21.,2.86767474496505,8.30764661663281));
#56360=CARTESIAN_POINT('Ctrl Pts',(-50.,2.8682745946465,8.20302084448955));
#56361=CARTESIAN_POINT('Ctrl Pts',(-21.,2.8682745946465,8.20302084448955));
#56362=CARTESIAN_POINT('Ctrl Pts',(-50.,2.86421236488386,8.099424390731));
#56363=CARTESIAN_POINT('Ctrl Pts',(-21.,2.86421236488386,8.099424390731));
#56364=CARTESIAN_POINT('Ctrl Pts',(-50.,2.85517326277626,7.9970485375799));
#56365=CARTESIAN_POINT('Ctrl Pts',(-21.,2.85517326277626,7.9970485375799));
#56366=CARTESIAN_POINT('Ctrl Pts',(-50.,2.84098400021345,7.89607078269802));
#56367=CARTESIAN_POINT('Ctrl Pts',(-21.,2.84098400021345,7.89607078269802));
#56368=CARTESIAN_POINT('Ctrl Pts',(-50.,2.82164615909785,7.79662146983088));
#56369=CARTESIAN_POINT('Ctrl Pts',(-21.,2.82164615909785,7.79662146983088));
#56370=CARTESIAN_POINT('Ctrl Pts',(-50.,2.79737835816915,7.69875126136884));
#56371=CARTESIAN_POINT('Ctrl Pts',(-21.,2.79737835816915,7.69875126136884));
#56372=CARTESIAN_POINT('Ctrl Pts',(-50.,2.76864747338962,7.60240247767684));
#56373=CARTESIAN_POINT('Ctrl Pts',(-21.,2.76864747338962,7.60240247767684));
#56374=CARTESIAN_POINT('Ctrl Pts',(-50.,2.73622951961898,7.50736587770304));
#56375=CARTESIAN_POINT('Ctrl Pts',(-21.,2.73622951961898,7.50736587770304));
#56376=CARTESIAN_POINT('Ctrl Pts',(-50.,2.70112557395893,7.41331375298832));
#56377=CARTESIAN_POINT('Ctrl Pts',(-21.,2.70112557395893,7.41331375298832));
#56378=CARTESIAN_POINT('Ctrl Pts',(-50.,2.66442452752942,7.31986152676826));
#56379=CARTESIAN_POINT('Ctrl Pts',(-21.,2.66442452752942,7.31986152676826));
#56380=CARTESIAN_POINT('Ctrl Pts',(-50.,2.62718125254576,7.22662075191781));
#56381=CARTESIAN_POINT('Ctrl Pts',(-21.,2.62718125254576,7.22662075191781));
#56382=CARTESIAN_POINT('Ctrl Pts',(-50.,2.59029498067661,7.13325283216217));
#56383=CARTESIAN_POINT('Ctrl Pts',(-21.,2.59029498067661,7.13325283216217));
#56384=CARTESIAN_POINT('Ctrl Pts',(-50.,2.55437015138428,7.03952961984441));
#56385=CARTESIAN_POINT('Ctrl Pts',(-21.,2.55437015138428,7.03952961984441));
#56386=CARTESIAN_POINT('Ctrl Pts',(-50.,2.5197596307744,6.94531805563895));
#56387=CARTESIAN_POINT('Ctrl Pts',(-21.,2.5197596307744,6.94531805563895));
#56388=CARTESIAN_POINT('Ctrl Pts',(-50.,2.49326086758344,6.8695059418988));
#56389=CARTESIAN_POINT('Ctrl Pts',(-21.,2.49326086758344,6.8695059418988));
#56390=CARTESIAN_POINT('Ctrl Pts',(-50.,2.47407975508802,6.8123887688799));
#56391=CARTESIAN_POINT('Ctrl Pts',(-21.,2.47407975508802,6.8123887688799));
#56392=CARTESIAN_POINT('Ctrl Pts',(-50.,2.46159994790965,6.77419608843537));
#56393=CARTESIAN_POINT('Ctrl Pts',(-21.,2.46159994790965,6.77419608843537));
#56394=CARTESIAN_POINT('Ctrl Pts',(-50.,2.45543694297675,6.75507110762463));
#56395=CARTESIAN_POINT('Ctrl Pts',(-21.,2.45543694297675,6.75507110762463));
#56396=CARTESIAN_POINT('',(-21.5,2.58947998462545,9.65891264114259));
#56397=CARTESIAN_POINT('Ctrl Pts',(-21.5,2.58947998462545,9.65891264114259));
#56398=CARTESIAN_POINT('Ctrl Pts',(-26.3333333333333,2.58947998462545,9.65891264114259));
#56399=CARTESIAN_POINT('Ctrl Pts',(-31.1666666666667,2.58947998462545,9.65891264114259));
#56400=CARTESIAN_POINT('Ctrl Pts',(-40.6666666666667,2.58947998462545,9.65891264114259));
#56401=CARTESIAN_POINT('Ctrl Pts',(-45.3333333333333,2.58947998462545,9.65891264114259));
#56402=CARTESIAN_POINT('Ctrl Pts',(-50.,2.58947998462545,9.65891264114259));
#56403=CARTESIAN_POINT('Ctrl Pts',(-21.,2.75760981235205,9.09096189205629));
#56404=CARTESIAN_POINT('Ctrl Pts',(-21.0595504621605,2.74206083288776,9.15790831819842));
#56405=CARTESIAN_POINT('Ctrl Pts',(-21.1201969195959,2.72465875026614,9.2263731836371));
#56406=CARTESIAN_POINT('Ctrl Pts',(-21.1820623827059,2.70512289983591,9.29649306845955));
#56407=CARTESIAN_POINT('Ctrl Pts',(-21.2426667634852,2.68598527346403,9.36518361058689));
#56408=CARTESIAN_POINT('Ctrl Pts',(-21.3044409593758,2.66479906737137,9.43546228600892));
#56409=CARTESIAN_POINT('Ctrl Pts',(-21.367500610643,2.64134946113152,9.50742323600585));
#56410=CARTESIAN_POINT('Ctrl Pts',(-21.4110415416979,2.62515816181354,9.5571102656595));
#56411=CARTESIAN_POINT('Ctrl Pts',(-21.45519531585,2.60788916582949,9.60759844441249));
#56412=CARTESIAN_POINT('Ctrl Pts',(-21.5,2.58947998461739,9.65891264116508));
#56413=CARTESIAN_POINT('Origin',(-35.75,0.,0.));
#56414=CARTESIAN_POINT('',(-21.5,6.52388598275276,7.57884632935924));
#56415=CARTESIAN_POINT('Origin',(-21.5,0.,0.));
#56416=CARTESIAN_POINT('Ctrl Pts',(-21.5,6.52388598275276,7.57884632935924));
#56417=CARTESIAN_POINT('Ctrl Pts',(-26.3333333333333,6.52388598275276,7.57884632935924));
#56418=CARTESIAN_POINT('Ctrl Pts',(-31.1666666666667,6.52388598275276,7.57884632935924));
#56419=CARTESIAN_POINT('Ctrl Pts',(-40.6666666666667,6.52388598275276,7.57884632935924));
#56420=CARTESIAN_POINT('Ctrl Pts',(-45.3333333333333,6.52388598275276,7.57884632935924));
#56421=CARTESIAN_POINT('Ctrl Pts',(-50.,6.52388598275276,7.57884632935924));
#56422=CARTESIAN_POINT('Origin',(-21.25,0.,0.));
#56423=CARTESIAN_POINT('Ctrl Pts',(-21.,6.42894112865204,6.99419158761941));
#56424=CARTESIAN_POINT('Ctrl Pts',(-21.1171767610994,6.45853087308296,7.12615087039341));
#56425=CARTESIAN_POINT('Ctrl Pts',(-21.2874825276462,6.49694802882376,7.32162583711294));
#56426=CARTESIAN_POINT('Ctrl Pts',(-21.5,6.52388598275277,7.57884632935924));
#56427=CARTESIAN_POINT('Ctrl Pts',(-50.,6.55597468860601,8.32941749958287));
#56428=CARTESIAN_POINT('Ctrl Pts',(-21.,6.55597468860601,8.32941749958287));
#56429=CARTESIAN_POINT('Ctrl Pts',(-50.,6.55632766789962,8.30553668898452));
#56430=CARTESIAN_POINT('Ctrl Pts',(-21.,6.55632766789962,8.30553668898452));
#56431=CARTESIAN_POINT('Ctrl Pts',(-50.,6.55682598292761,8.25785023779518));
#56432=CARTESIAN_POINT('Ctrl Pts',(-21.,6.55682598292761,8.25785023779518));
#56433=CARTESIAN_POINT('Ctrl Pts',(-50.,6.55695052439907,8.18654607180369));
#56434=CARTESIAN_POINT('Ctrl Pts',(-21.,6.55695052439907,8.18654607180369));
#56435=CARTESIAN_POINT('Ctrl Pts',(-50.,6.55586906420033,8.0919254651127));
#56436=CARTESIAN_POINT('Ctrl Pts',(-21.,6.55586906420033,8.0919254651127));
#56437=CARTESIAN_POINT('Ctrl Pts',(-50.,6.55242508650163,7.97441053046901));
#56438=CARTESIAN_POINT('Ctrl Pts',(-21.,6.55242508650163,7.97441053046901));
#56439=CARTESIAN_POINT('Ctrl Pts',(-50.,6.54686687486885,7.85767464841055));
#56440=CARTESIAN_POINT('Ctrl Pts',(-21.,6.54686687486885,7.85767464841055));
#56441=CARTESIAN_POINT('Ctrl Pts',(-50.,6.53916282696568,7.74174994850129));
#56442=CARTESIAN_POINT('Ctrl Pts',(-21.,6.53916282696568,7.74174994850129));
#56443=CARTESIAN_POINT('Ctrl Pts',(-50.,6.5292721024685,7.6266854031787));
#56444=CARTESIAN_POINT('Ctrl Pts',(-21.,6.5292721024685,7.6266854031787));
#56445=CARTESIAN_POINT('Ctrl Pts',(-50.,6.51714368227899,7.51255191568567));
#56446=CARTESIAN_POINT('Ctrl Pts',(-21.,6.51714368227899,7.51255191568567));
#56447=CARTESIAN_POINT('Ctrl Pts',(-50.,6.5027237919627,7.39943421923609));
#56448=CARTESIAN_POINT('Ctrl Pts',(-21.,6.5027237919627,7.39943421923609));
#56449=CARTESIAN_POINT('Ctrl Pts',(-50.,6.48596514159778,7.28741967054497));
#56450=CARTESIAN_POINT('Ctrl Pts',(-21.,6.48596514159778,7.28741967054497));
#56451=CARTESIAN_POINT('Ctrl Pts',(-50.,6.46683693263443,7.17658703219621));
#56452=CARTESIAN_POINT('Ctrl Pts',(-21.,6.46683693263443,7.17658703219621));
#56453=CARTESIAN_POINT('Ctrl Pts',(-50.,6.44533241567678,7.06699729667253));
#56454=CARTESIAN_POINT('Ctrl Pts',(-21.,6.44533241567678,7.06699729667253));
#56455=CARTESIAN_POINT('Ctrl Pts',(-50.,6.42148411170256,6.95867791439771));
#56456=CARTESIAN_POINT('Ctrl Pts',(-21.,6.42148411170256,6.95867791439771));
#56457=CARTESIAN_POINT('Ctrl Pts',(-50.,6.39534644338642,6.85163598146165));
#56458=CARTESIAN_POINT('Ctrl Pts',(-21.,6.39534644338642,6.85163598146165));
#56459=CARTESIAN_POINT('Ctrl Pts',(-50.,6.36696110296949,6.74588705654512));
#56460=CARTESIAN_POINT('Ctrl Pts',(-21.,6.36696110296949,6.74588705654512));
#56461=CARTESIAN_POINT('Ctrl Pts',(-50.,6.33632590879467,6.64148049150319));
#56462=CARTESIAN_POINT('Ctrl Pts',(-21.,6.33632590879467,6.64148049150319));
#56463=CARTESIAN_POINT('Ctrl Pts',(-50.,6.30336681095649,6.53852299564495));
#56464=CARTESIAN_POINT('Ctrl Pts',(-21.,6.30336681095649,6.53852299564495));
#56465=CARTESIAN_POINT('Ctrl Pts',(-50.,6.2678972444421,6.43721103768399));
#56466=CARTESIAN_POINT('Ctrl Pts',(-21.,6.2678972444421,6.43721103768399));
#56467=CARTESIAN_POINT('Ctrl Pts',(-50.,6.22963155144596,6.33782488040965));
#56468=CARTESIAN_POINT('Ctrl Pts',(-21.,6.22963155144596,6.33782488040965));
#56469=CARTESIAN_POINT('Ctrl Pts',(-50.,6.18823844577549,6.2406935262026));
#56470=CARTESIAN_POINT('Ctrl Pts',(-21.,6.18823844577549,6.2406935262026));
#56471=CARTESIAN_POINT('Ctrl Pts',(-50.,6.14338347043832,6.14616869769857));
#56472=CARTESIAN_POINT('Ctrl Pts',(-21.,6.14338347043832,6.14616869769857));
#56473=CARTESIAN_POINT('Ctrl Pts',(-50.,6.09477471117184,6.05459405347559));
#56474=CARTESIAN_POINT('Ctrl Pts',(-21.,6.09477471117184,6.05459405347559));
#56475=CARTESIAN_POINT('Ctrl Pts',(-50.,6.04221154361855,5.96627851638222));
#56476=CARTESIAN_POINT('Ctrl Pts',(-21.,6.04221154361855,5.96627851638222));
#56477=CARTESIAN_POINT('Ctrl Pts',(-50.,5.98561485393513,5.88145719317904));
#56478=CARTESIAN_POINT('Ctrl Pts',(-21.,5.98561485393513,5.88145719317904));
#56479=CARTESIAN_POINT('Ctrl Pts',(-50.,5.92504262139805,5.80024683316115));
#56480=CARTESIAN_POINT('Ctrl Pts',(-21.,5.92504262139805,5.80024683316115));
#56481=CARTESIAN_POINT('Ctrl Pts',(-50.,5.86071379627312,5.72259822644884));
#56482=CARTESIAN_POINT('Ctrl Pts',(-21.,5.86071379627312,5.72259822644884));
#56483=CARTESIAN_POINT('Ctrl Pts',(-50.,5.79302399301176,5.64825683559838));
#56484=CARTESIAN_POINT('Ctrl Pts',(-21.,5.79302399301176,5.64825683559838));
#56485=CARTESIAN_POINT('Ctrl Pts',(-50.,5.72258159055366,5.57669744070723));
#56486=CARTESIAN_POINT('Ctrl Pts',(-21.,5.72258159055366,5.57669744070723));
#56487=CARTESIAN_POINT('Ctrl Pts',(-50.,5.65014634083023,5.50719043557996));
#56488=CARTESIAN_POINT('Ctrl Pts',(-21.,5.65014634083023,5.50719043557996));
#56489=CARTESIAN_POINT('Ctrl Pts',(-50.,5.57653243923659,5.43891687637388));
#56490=CARTESIAN_POINT('Ctrl Pts',(-21.,5.57653243923659,5.43891687637388));
#56491=CARTESIAN_POINT('Ctrl Pts',(-50.,5.50252175190725,5.37106909242141));
#56492=CARTESIAN_POINT('Ctrl Pts',(-21.,5.50252175190725,5.37106909242141));
#56493=CARTESIAN_POINT('Ctrl Pts',(-50.,5.42877754716296,5.30295185702147));
#56494=CARTESIAN_POINT('Ctrl Pts',(-21.,5.42877754716296,5.30295185702147));
#56495=CARTESIAN_POINT('Ctrl Pts',(-50.,5.35574541658332,5.23409735978387));
#56496=CARTESIAN_POINT('Ctrl Pts',(-21.,5.35574541658332,5.23409735978387));
#56497=CARTESIAN_POINT('Ctrl Pts',(-50.,5.28368554926634,5.16423261553338));
#56498=CARTESIAN_POINT('Ctrl Pts',(-21.,5.28368554926634,5.16423261553338));
#56499=CARTESIAN_POINT('Ctrl Pts',(-50.,5.22691734521339,5.10742564369892));
#56500=CARTESIAN_POINT('Ctrl Pts',(-21.,5.22691734521339,5.10742564369892));
#56501=CARTESIAN_POINT('Ctrl Pts',(-50.,5.18485354740602,5.06428722179623));
#56502=CARTESIAN_POINT('Ctrl Pts',(-21.,5.18485354740602,5.06428722179623));
#56503=CARTESIAN_POINT('Ctrl Pts',(-50.,5.15703844666268,5.03529159113598));
#56504=CARTESIAN_POINT('Ctrl Pts',(-21.,5.15703844666268,5.03529159113598));
#56505=CARTESIAN_POINT('Ctrl Pts',(-50.,5.14318775290069,5.02073460645076));
#56506=CARTESIAN_POINT('Ctrl Pts',(-21.,5.14318775290069,5.02073460645076));
#56507=CARTESIAN_POINT('',(-50.,5.14318775290069,5.02073460645077));
#56508=CARTESIAN_POINT('Origin',(-50.,0.,0.));
#56509=CARTESIAN_POINT('',(-50.,6.03932124977421,3.89701874412038));
#56510=CARTESIAN_POINT('Ctrl Pts',(-50.,6.03932124977421,3.89701874412038));
#56511=CARTESIAN_POINT('Ctrl Pts',(-21.,6.03932124977421,3.89701874412038));
#56512=CARTESIAN_POINT('Ctrl Pts',(-50.,6.05965257770704,3.90939030583537));
#56513=CARTESIAN_POINT('Ctrl Pts',(-21.,6.05965257770704,3.90939030583537));
#56514=CARTESIAN_POINT('Ctrl Pts',(-50.,6.10023490810719,3.93427763849175));
#56515=CARTESIAN_POINT('Ctrl Pts',(-21.,6.10023490810719,3.93427763849175));
#56516=CARTESIAN_POINT('Ctrl Pts',(-50.,6.16086742147114,3.97204127711522));
#56517=CARTESIAN_POINT('Ctrl Pts',(-21.,6.16086742147114,3.97204127711522));
#56518=CARTESIAN_POINT('Ctrl Pts',(-50.,6.24122821720367,4.02325912271413));
#56519=CARTESIAN_POINT('Ctrl Pts',(-21.,6.24122821720367,4.02325912271413));
#56520=CARTESIAN_POINT('Ctrl Pts',(-50.,6.34092094513049,4.08864152493875));
#56521=CARTESIAN_POINT('Ctrl Pts',(-21.,6.34092094513049,4.08864152493875));
#56522=CARTESIAN_POINT('Ctrl Pts',(-50.,6.44000100425059,4.15511874483725));
#56523=CARTESIAN_POINT('Ctrl Pts',(-21.,6.44000100425059,4.15511874483725));
#56524=CARTESIAN_POINT('Ctrl Pts',(-50.,6.53876341785232,4.22215377357323));
#56525=CARTESIAN_POINT('Ctrl Pts',(-21.,6.53876341785232,4.22215377357323));
#56526=CARTESIAN_POINT('Ctrl Pts',(-50.,6.63770990687462,4.2888323596294));
#56527=CARTESIAN_POINT('Ctrl Pts',(-21.,6.63770990687462,4.2888323596294));
#56528=CARTESIAN_POINT('Ctrl Pts',(-50.,6.73752748880879,4.35393408054299));
#56529=CARTESIAN_POINT('Ctrl Pts',(-21.,6.73752748880879,4.35393408054299));
#56530=CARTESIAN_POINT('Ctrl Pts',(-50.,6.83906640781858,4.4160130309926));
#56531=CARTESIAN_POINT('Ctrl Pts',(-21.,6.83906640781858,4.4160130309926));
#56532=CARTESIAN_POINT('Ctrl Pts',(-50.,6.94330777957998,4.47348457408032));
#56533=CARTESIAN_POINT('Ctrl Pts',(-21.,6.94330777957998,4.47348457408032));
#56534=CARTESIAN_POINT('Ctrl Pts',(-50.,7.05136577826386,4.52468089222283));
#56535=CARTESIAN_POINT('Ctrl Pts',(-21.,7.05136577826386,4.52468089222283));
#56536=CARTESIAN_POINT('Ctrl Pts',(-50.,7.16419105444418,4.56819583049617));
#56537=CARTESIAN_POINT('Ctrl Pts',(-21.,7.16419105444418,4.56819583049617));
#56538=CARTESIAN_POINT('Ctrl Pts',(-50.,7.28216972266428,4.60333867057275));
#56539=CARTESIAN_POINT('Ctrl Pts',(-21.,7.28216972266428,4.60333867057275));
#56540=CARTESIAN_POINT('Ctrl Pts',(-50.,7.40483002515176,4.63046946729401));
#56541=CARTESIAN_POINT('Ctrl Pts',(-21.,7.40483002515176,4.63046946729401));
#56542=CARTESIAN_POINT('Ctrl Pts',(-50.,7.53031371454558,4.65160090645339));
#56543=CARTESIAN_POINT('Ctrl Pts',(-21.,7.53031371454558,4.65160090645339));
#56544=CARTESIAN_POINT('Ctrl Pts',(-50.,7.65604731918147,4.66963928443128));
#56545=CARTESIAN_POINT('Ctrl Pts',(-21.,7.65604731918147,4.66963928443128));
#56546=CARTESIAN_POINT('Ctrl Pts',(-50.,7.78000590743498,4.68695765535521));
#56547=CARTESIAN_POINT('Ctrl Pts',(-21.,7.78000590743498,4.68695765535521));
#56548=CARTESIAN_POINT('Ctrl Pts',(-50.,7.9015907237349,4.70439891524807));
#56549=CARTESIAN_POINT('Ctrl Pts',(-21.,7.9015907237349,4.70439891524807));
#56550=CARTESIAN_POINT('Ctrl Pts',(-50.,8.02313747309844,4.71958541389958));
#56551=CARTESIAN_POINT('Ctrl Pts',(-21.,8.02313747309844,4.71958541389958));
#56552=CARTESIAN_POINT('Ctrl Pts',(-50.,8.14929412649754,4.72756454905465));
#56553=CARTESIAN_POINT('Ctrl Pts',(-21.,8.14929412649754,4.72756454905465));
#56554=CARTESIAN_POINT('Ctrl Pts',(-50.,8.2843230642502,4.72372591244527));
#56555=CARTESIAN_POINT('Ctrl Pts',(-21.,8.2843230642502,4.72372591244527));
#56556=CARTESIAN_POINT('Ctrl Pts',(-50.,8.43013206622476,4.70592432223511));
#56557=CARTESIAN_POINT('Ctrl Pts',(-21.,8.43013206622476,4.70592432223511));
#56558=CARTESIAN_POINT('Ctrl Pts',(-50.,8.58364001156461,4.67732113139128));
#56559=CARTESIAN_POINT('Ctrl Pts',(-21.,8.58364001156461,4.67732113139128));
#56560=CARTESIAN_POINT('Ctrl Pts',(-50.,8.73551023481551,4.6477574323839));
#56561=CARTESIAN_POINT('Ctrl Pts',(-21.,8.73551023481551,4.6477574323839));
#56562=CARTESIAN_POINT('Ctrl Pts',(-50.,8.87281293245584,4.63091679961492));
#56563=CARTESIAN_POINT('Ctrl Pts',(-21.,8.87281293245584,4.63091679961492));
#56564=CARTESIAN_POINT('Ctrl Pts',(-50.,8.98102877679355,4.64219420602678));
#56565=CARTESIAN_POINT('Ctrl Pts',(-21.,8.98102877679355,4.64219420602678));
#56566=CARTESIAN_POINT('Ctrl Pts',(-50.,9.04624816652329,4.69635508274639));
#56567=CARTESIAN_POINT('Ctrl Pts',(-21.,9.04624816652329,4.69635508274639));
#56568=CARTESIAN_POINT('Ctrl Pts',(-50.,9.05742940904388,4.80513309368965));
#56569=CARTESIAN_POINT('Ctrl Pts',(-21.,9.05742940904388,4.80513309368965));
#56570=CARTESIAN_POINT('Ctrl Pts',(-50.,9.00617835005594,4.97746052424366));
#56571=CARTESIAN_POINT('Ctrl Pts',(-21.,9.00617835005594,4.97746052424366));
#56572=CARTESIAN_POINT('Ctrl Pts',(-50.,8.88631984769767,5.21992023813997));
#56573=CARTESIAN_POINT('Ctrl Pts',(-21.,8.88631984769767,5.21992023813997));
#56574=CARTESIAN_POINT('Ctrl Pts',(-50.,8.6935651987215,5.53709589298789));
#56575=CARTESIAN_POINT('Ctrl Pts',(-21.,8.6935651987215,5.53709589298789));
#56576=CARTESIAN_POINT('Ctrl Pts',(-50.,8.42515810469916,5.93194523247474));
#56577=CARTESIAN_POINT('Ctrl Pts',(-21.,8.42515810469916,5.93194523247474));
#56578=CARTESIAN_POINT('Ctrl Pts',(-50.,8.07954770829655,6.40614484298506));
#56579=CARTESIAN_POINT('Ctrl Pts',(-21.,8.07954770829655,6.40614484298506));
#56580=CARTESIAN_POINT('Ctrl Pts',(-50.,7.65606629865851,6.96043017782053));
#56581=CARTESIAN_POINT('Ctrl Pts',(-21.,7.65606629865851,6.96043017782053));
#56582=CARTESIAN_POINT('Ctrl Pts',(-50.,7.25490905174796,7.46802385431575));
#56583=CARTESIAN_POINT('Ctrl Pts',(-21.,7.25490905174796,7.46802385431575));
#56584=CARTESIAN_POINT('Ctrl Pts',(-50.,6.91903663131433,7.8847336425335));
#56585=CARTESIAN_POINT('Ctrl Pts',(-21.,6.91903663131433,7.8847336425335));
#56586=CARTESIAN_POINT('Ctrl Pts',(-50.,6.67958481505646,8.17852534961222));
#56587=CARTESIAN_POINT('Ctrl Pts',(-21.,6.67958481505646,8.17852534961222));
#56588=CARTESIAN_POINT('Ctrl Pts',(-50.,6.55597468860601,8.32941749958287));
#56589=CARTESIAN_POINT('Ctrl Pts',(-21.,6.55597468860601,8.32941749958287));
#56590=CARTESIAN_POINT('',(-21.5,8.85937132577942,4.63805343996351));
#56591=CARTESIAN_POINT('Ctrl Pts',(-21.5,8.85937132577942,4.63805343996351));
#56592=CARTESIAN_POINT('Ctrl Pts',(-21.4716714037526,8.82699312116116,4.63882198977594));
#56593=CARTESIAN_POINT('Ctrl Pts',(-21.4424150110737,8.79205190661356,4.64240188595715));
#56594=CARTESIAN_POINT('Ctrl Pts',(-21.2909879716439,8.6069526617269,4.66814581613095));
#56595=CARTESIAN_POINT('Ctrl Pts',(-21.1630186724939,8.43596084926503,4.71373942955312));
#56596=CARTESIAN_POINT('Ctrl Pts',(-21.,8.24274231917123,4.72304976257329));
#56597=CARTESIAN_POINT('Ctrl Pts',(-50.,8.85937132577942,4.63805343996351));
#56598=CARTESIAN_POINT('Ctrl Pts',(-45.1666666666667,8.85937132577942,4.63805343996351));
#56599=CARTESIAN_POINT('Ctrl Pts',(-40.3333333333333,8.85937132577942,4.63805343996351));
#56600=CARTESIAN_POINT('Ctrl Pts',(-30.8333333333333,8.85937132577942,4.63805343996351));
#56601=CARTESIAN_POINT('Ctrl Pts',(-26.1666666666667,8.85937132577942,4.63805343996351));
#56602=CARTESIAN_POINT('Ctrl Pts',(-21.5,8.85937132577942,4.63805343996351));
#56603=CARTESIAN_POINT('Origin',(-21.25,0.,0.));
#56604=CARTESIAN_POINT('Origin',(-21.5,0.,0.));
#56605=CARTESIAN_POINT('Origin',(-35.75,0.,0.));
#56606=CARTESIAN_POINT('Ctrl Pts',(-50.,9.52072790258051,4.66001504343333));
#56607=CARTESIAN_POINT('Ctrl Pts',(-21.,9.52072790258051,4.66001504343333));
#56608=CARTESIAN_POINT('Ctrl Pts',(-50.,9.5106844305395,4.6383460245682));
#56609=CARTESIAN_POINT('Ctrl Pts',(-21.,9.5106844305395,4.6383460245682));
#56610=CARTESIAN_POINT('Ctrl Pts',(-50.,9.49044302111884,4.59516580583826));
#56611=CARTESIAN_POINT('Ctrl Pts',(-21.,9.49044302111884,4.59516580583826));
#56612=CARTESIAN_POINT('Ctrl Pts',(-50.,9.45961751095234,4.53086893560887));
#56613=CARTESIAN_POINT('Ctrl Pts',(-21.,9.45961751095234,4.53086893560887));
#56614=CARTESIAN_POINT('Ctrl Pts',(-50.,9.41758880635275,4.44608794271298));
#56615=CARTESIAN_POINT('Ctrl Pts',(-21.,9.41758880635275,4.44608794271298));
#56616=CARTESIAN_POINT('Ctrl Pts',(-50.,9.36349807041911,4.34170493100677));
#56617=CARTESIAN_POINT('Ctrl Pts',(-21.,9.36349807041911,4.34170493100677));
#56618=CARTESIAN_POINT('Ctrl Pts',(-50.,9.30784049378005,4.23894115315102));
#56619=CARTESIAN_POINT('Ctrl Pts',(-21.,9.30784049378005,4.23894115315102));
#56620=CARTESIAN_POINT('Ctrl Pts',(-50.,9.25060154420976,4.1378392686224));
#56621=CARTESIAN_POINT('Ctrl Pts',(-21.,9.25060154420976,4.1378392686224));
#56622=CARTESIAN_POINT('Ctrl Pts',(-50.,9.19176567419237,4.03846112001482));
#56623=CARTESIAN_POINT('Ctrl Pts',(-21.,9.19176567419237,4.03846112001482));
#56624=CARTESIAN_POINT('Ctrl Pts',(-50.,9.13131768087278,3.94089272529988));
#56625=CARTESIAN_POINT('Ctrl Pts',(-21.,9.13131768087278,3.94089272529988));
#56626=CARTESIAN_POINT('Ctrl Pts',(-50.,9.06924587952332,3.84523375831808));
#56627=CARTESIAN_POINT('Ctrl Pts',(-21.,9.06924587952332,3.84523375831808));
#56628=CARTESIAN_POINT('Ctrl Pts',(-50.,9.0055455660548,3.75158344307814));
#56629=CARTESIAN_POINT('Ctrl Pts',(-21.,9.0055455660548,3.75158344307814));
#56630=CARTESIAN_POINT('Ctrl Pts',(-50.,8.94022316573707,3.66002610520606));
#56631=CARTESIAN_POINT('Ctrl Pts',(-21.,8.94022316573707,3.66002610520606));
#56632=CARTESIAN_POINT('Ctrl Pts',(-50.,8.87329906122102,3.57061962548306));
#56633=CARTESIAN_POINT('Ctrl Pts',(-21.,8.87329906122102,3.57061962548306));
#56634=CARTESIAN_POINT('Ctrl Pts',(-50.,8.80481446318767,3.48337462556297));
#56635=CARTESIAN_POINT('Ctrl Pts',(-21.,8.80481446318767,3.48337462556297));
#56636=CARTESIAN_POINT('Ctrl Pts',(-50.,8.7348214836506,3.3982738856883));
#56637=CARTESIAN_POINT('Ctrl Pts',(-21.,8.7348214836506,3.3982738856883));
#56638=CARTESIAN_POINT('Ctrl Pts',(-50.,8.66336443667969,3.31531333416059));
#56639=CARTESIAN_POINT('Ctrl Pts',(-21.,8.66336443667969,3.31531333416059));
#56640=CARTESIAN_POINT('Ctrl Pts',(-50.,8.59046276963722,3.23453838205034));
#56641=CARTESIAN_POINT('Ctrl Pts',(-21.,8.59046276963722,3.23453838205034));
#56642=CARTESIAN_POINT('Ctrl Pts',(-50.,8.51609606529771,3.15607730017284));
#56643=CARTESIAN_POINT('Ctrl Pts',(-21.,8.51609606529771,3.15607730017284));
#56644=CARTESIAN_POINT('Ctrl Pts',(-50.,8.44018147897284,3.08018804824792));
#56645=CARTESIAN_POINT('Ctrl Pts',(-21.,8.44018147897284,3.08018804824792));
#56646=CARTESIAN_POINT('Ctrl Pts',(-50.,8.36258324333989,3.00724707660037));
#56647=CARTESIAN_POINT('Ctrl Pts',(-21.,8.36258324333989,3.00724707660037));
#56648=CARTESIAN_POINT('Ctrl Pts',(-50.,8.28314562863609,2.93769454582461));
#56649=CARTESIAN_POINT('Ctrl Pts',(-21.,8.28314562863609,2.93769454582461));
#56650=CARTESIAN_POINT('Ctrl Pts',(-50.,8.201719906256,2.87199246251599));
#56651=CARTESIAN_POINT('Ctrl Pts',(-21.,8.201719906256,2.87199246251599));
#56652=CARTESIAN_POINT('Ctrl Pts',(-50.,8.11819217840571,2.81057710920625));
#56653=CARTESIAN_POINT('Ctrl Pts',(-21.,8.11819217840571,2.81057710920625));
#56654=CARTESIAN_POINT('Ctrl Pts',(-50.,8.03251572538561,2.75381386341092));
#56655=CARTESIAN_POINT('Ctrl Pts',(-21.,8.03251572538561,2.75381386341092));
#56656=CARTESIAN_POINT('Ctrl Pts',(-50.,7.94472127708621,2.70194887521209));
#56657=CARTESIAN_POINT('Ctrl Pts',(-21.,7.94472127708621,2.70194887521209));
#56658=CARTESIAN_POINT('Ctrl Pts',(-50.,7.85491172665132,2.65506217582471));
#56659=CARTESIAN_POINT('Ctrl Pts',(-21.,7.85491172665132,2.65506217582471));
#56660=CARTESIAN_POINT('Ctrl Pts',(-50.,7.76326299008741,2.61301442971916));
#56661=CARTESIAN_POINT('Ctrl Pts',(-21.,7.76326299008741,2.61301442971916));
#56662=CARTESIAN_POINT('Ctrl Pts',(-50.,7.67002106404108,2.5754046559055));
#56663=CARTESIAN_POINT('Ctrl Pts',(-21.,7.67002106404108,2.5754046559055));
#56664=CARTESIAN_POINT('Ctrl Pts',(-50.,7.57550619462173,2.54149568187359));
#56665=CARTESIAN_POINT('Ctrl Pts',(-21.,7.57550619462173,2.54149568187359));
#56666=CARTESIAN_POINT('Ctrl Pts',(-50.,7.4800863304027,2.5103005111467));
#56667=CARTESIAN_POINT('Ctrl Pts',(-21.,7.4800863304027,2.5103005111467));
#56668=CARTESIAN_POINT('Ctrl Pts',(-50.,7.3841397096708,2.4807280346756));
#56669=CARTESIAN_POINT('Ctrl Pts',(-21.,7.3841397096708,2.4807280346756));
#56670=CARTESIAN_POINT('Ctrl Pts',(-50.,7.28802033430286,2.45171132733138));
#56671=CARTESIAN_POINT('Ctrl Pts',(-21.,7.28802033430286,2.45171132733138));
#56672=CARTESIAN_POINT('Ctrl Pts',(-50.,7.19202414084635,2.42233623016115));
#56673=CARTESIAN_POINT('Ctrl Pts',(-21.,7.19202414084635,2.42233623016115));
#56674=CARTESIAN_POINT('Ctrl Pts',(-50.,7.09634961812101,2.39198792562662));
#56675=CARTESIAN_POINT('Ctrl Pts',(-21.,7.09634961812101,2.39198792562662));
#56676=CARTESIAN_POINT('Ctrl Pts',(-50.,7.00111274457534,2.36030757076476));
#56677=CARTESIAN_POINT('Ctrl Pts',(-21.,7.00111274457534,2.36030757076476));
#56678=CARTESIAN_POINT('Ctrl Pts',(-50.,6.92531873868941,2.33375705829959));
#56679=CARTESIAN_POINT('Ctrl Pts',(-21.,6.92531873868941,2.33375705829959));
#56680=CARTESIAN_POINT('Ctrl Pts',(-50.,6.86870350660446,2.31314148102898));
#56681=CARTESIAN_POINT('Ctrl Pts',(-21.,6.86870350660446,2.31314148102898));
#56682=CARTESIAN_POINT('Ctrl Pts',(-50.,6.8310622341282,2.29908584041335));
#56683=CARTESIAN_POINT('Ctrl Pts',(-21.,6.8310622341282,2.29908584041335));
#56684=CARTESIAN_POINT('Ctrl Pts',(-50.,6.8122671513043,2.29198004120026));
#56685=CARTESIAN_POINT('Ctrl Pts',(-21.,6.8122671513043,2.29198004120026));
#56686=CARTESIAN_POINT('',(-21.5,9.16615635178499,3.9976965535958));
#56687=CARTESIAN_POINT('Ctrl Pts',(-21.,8.82694180863381,3.51213586112389));
#56688=CARTESIAN_POINT('Ctrl Pts',(-21.1171767610705,8.91085623417581,3.61818855775461));
#56689=CARTESIAN_POINT('Ctrl Pts',(-21.2874825276219,9.03028230496099,3.77763683804508));
#56690=CARTESIAN_POINT('Ctrl Pts',(-21.5,9.16615635178498,3.9976965535958));
#56691=CARTESIAN_POINT('',(-50.,6.8122671513043,2.29198004120026));
#56692=CARTESIAN_POINT('Ctrl Pts',(-21.5,9.16615635178499,3.9976965535958));
#56693=CARTESIAN_POINT('Ctrl Pts',(-26.3333333333333,9.16615635178499,3.9976965535958));
#56694=CARTESIAN_POINT('Ctrl Pts',(-31.1666666666667,9.16615635178499,3.9976965535958));
#56695=CARTESIAN_POINT('Ctrl Pts',(-40.6666666666667,9.16615635178499,3.9976965535958));
#56696=CARTESIAN_POINT('Ctrl Pts',(-45.3333333333333,9.16615635178499,3.9976965535958));
#56697=CARTESIAN_POINT('Ctrl Pts',(-50.,9.16615635178499,3.9976965535958));
#56698=CARTESIAN_POINT('Origin',(-50.,0.,0.));
#56699=CARTESIAN_POINT('',(-50.,7.13209349341826,0.890729280500491));
#56700=CARTESIAN_POINT('Ctrl Pts',(-50.,7.13209349341826,0.890729280500491));
#56701=CARTESIAN_POINT('Ctrl Pts',(-21.,7.13209349341826,0.890729280500491));
#56702=CARTESIAN_POINT('Ctrl Pts',(-50.,7.15577920638447,0.893054239868309));
#56703=CARTESIAN_POINT('Ctrl Pts',(-21.,7.15577920638447,0.893054239868309));
#56704=CARTESIAN_POINT('Ctrl Pts',(-50.,7.20314083161155,0.897868938540711));
#56705=CARTESIAN_POINT('Ctrl Pts',(-21.,7.20314083161155,0.897868938540711));
#56706=CARTESIAN_POINT('Ctrl Pts',(-50.,7.27415386726379,0.90558533966873));
#56707=CARTESIAN_POINT('Ctrl Pts',(-21.,7.27415386726379,0.90558533966873));
#56708=CARTESIAN_POINT('Ctrl Pts',(-50.,7.36877903277666,0.916863781503487));
#56709=CARTESIAN_POINT('Ctrl Pts',(-21.,7.36877903277666,0.916863781503487));
#56710=CARTESIAN_POINT('Ctrl Pts',(-50.,7.4869674381447,0.932516236860827));
#56711=CARTESIAN_POINT('Ctrl Pts',(-21.,7.4869674381447,0.932516236860827));
#56712=CARTESIAN_POINT('Ctrl Pts',(-50.,7.60507887157754,0.949420915891057));
#56713=CARTESIAN_POINT('Ctrl Pts',(-21.,7.60507887157754,0.949420915891057));
#56714=CARTESIAN_POINT('Ctrl Pts',(-50.,7.72314614047142,0.966965984543333));
#56715=CARTESIAN_POINT('Ctrl Pts',(-21.,7.72314614047142,0.966965984543333));
#56716=CARTESIAN_POINT('Ctrl Pts',(-50.,7.84122460090589,0.984110042106143));
#56717=CARTESIAN_POINT('Ctrl Pts',(-21.,7.84122460090589,0.984110042106143));
#56718=CARTESIAN_POINT('Ctrl Pts',(-50.,7.95940371279084,0.999455440216893));
#56719=CARTESIAN_POINT('Ctrl Pts',(-21.,7.95940371279084,0.999455440216893));
#56720=CARTESIAN_POINT('Ctrl Pts',(-50.,8.0778221648407,1.01133055607812));
#56721=CARTESIAN_POINT('Ctrl Pts',(-21.,8.0778221648407,1.01133055607812));
#56722=CARTESIAN_POINT('Ctrl Pts',(-50.,8.19667636355292,1.01788199103989));
#56723=CARTESIAN_POINT('Ctrl Pts',(-21.,8.19667636355292,1.01788199103989));
#56724=CARTESIAN_POINT('Ctrl Pts',(-50.,8.31624650623966,1.017123671327));
#56725=CARTESIAN_POINT('Ctrl Pts',(-21.,8.31624650623966,1.017123671327));
#56726=CARTESIAN_POINT('Ctrl Pts',(-50.,8.43677899171613,1.00737622330388));
#56727=CARTESIAN_POINT('Ctrl Pts',(-21.,8.43677899171613,1.00737622330388));
#56728=CARTESIAN_POINT('Ctrl Pts',(-50.,8.55832200571467,0.987849802439111));
#56729=CARTESIAN_POINT('Ctrl Pts',(-21.,8.55832200571467,0.987849802439111));
#56730=CARTESIAN_POINT('Ctrl Pts',(-50.,8.68060673111004,0.95907349496179));
#56731=CARTESIAN_POINT('Ctrl Pts',(-21.,8.68060673111004,0.95907349496179));
#56732=CARTESIAN_POINT('Ctrl Pts',(-50.,8.80283221651881,0.923666931425907));
#56733=CARTESIAN_POINT('Ctrl Pts',(-21.,8.80283221651881,0.923666931425907));
#56734=CARTESIAN_POINT('Ctrl Pts',(-50.,8.92394083882956,0.885365181899305));
#56735=CARTESIAN_POINT('Ctrl Pts',(-21.,8.92394083882956,0.885365181899305));
#56736=CARTESIAN_POINT('Ctrl Pts',(-50.,9.04313782728701,0.847184879177382));
#56737=CARTESIAN_POINT('Ctrl Pts',(-21.,9.04313782728701,0.847184879177382));
#56738=CARTESIAN_POINT('Ctrl Pts',(-50.,9.1602494406401,0.810145236641718));
#56739=CARTESIAN_POINT('Ctrl Pts',(-21.,9.1602494406401,0.810145236641718));
#56740=CARTESIAN_POINT('Ctrl Pts',(-50.,9.27634845263042,0.771090641047727));
#56741=CARTESIAN_POINT('Ctrl Pts',(-21.,9.27634845263042,0.771090641047727));
#56742=CARTESIAN_POINT('Ctrl Pts',(-50.,9.39347368681776,0.723542272923875));
#56743=CARTESIAN_POINT('Ctrl Pts',(-21.,9.39347368681776,0.723542272923875));
#56744=CARTESIAN_POINT('Ctrl Pts',(-50.,9.51346503399365,0.661496920442432));
#56745=CARTESIAN_POINT('Ctrl Pts',(-21.,9.51346503399365,0.661496920442432));
#56746=CARTESIAN_POINT('Ctrl Pts',(-50.,9.63711058491003,0.582194086890199));
#56747=CARTESIAN_POINT('Ctrl Pts',(-21.,9.63711058491003,0.582194086890199));
#56748=CARTESIAN_POINT('Ctrl Pts',(-50.,9.76300600524289,0.489818901108929));
#56749=CARTESIAN_POINT('Ctrl Pts',(-21.,9.76300600524289,0.489818901108929));
#56750=CARTESIAN_POINT('Ctrl Pts',(-50.,9.88700914008587,0.397288908358525));
#56751=CARTESIAN_POINT('Ctrl Pts',(-21.,9.88700914008587,0.397288908358525));
#56752=CARTESIAN_POINT('Ctrl Pts',(-50.,10.0034077194239,0.322542614674784));
#56753=CARTESIAN_POINT('Ctrl Pts',(-21.,10.0034077194239,0.322542614674784));
#56754=CARTESIAN_POINT('Ctrl Pts',(-50.,10.1057999094475,0.285750111589545));
#56755=CARTESIAN_POINT('Ctrl Pts',(-21.,10.1057999094475,0.285750111589545));
#56756=CARTESIAN_POINT('Ctrl Pts',(-50.,10.1880600728826,0.306249742693306));
#56757=CARTESIAN_POINT('Ctrl Pts',(-21.,10.1880600728826,0.306249742693306));
#56758=CARTESIAN_POINT('Ctrl Pts',(-50.,10.2453310344199,0.399403984752718));
#56759=CARTESIAN_POINT('Ctrl Pts',(-21.,10.2453310344199,0.399403984752718));
#56760=CARTESIAN_POINT('Ctrl Pts',(-50.,10.2739254957461,0.576902635874919));
#56761=CARTESIAN_POINT('Ctrl Pts',(-21.,10.2739254957461,0.576902635874919));
#56762=CARTESIAN_POINT('Ctrl Pts',(-50.,10.2711360438186,0.847355944984259));
#56763=CARTESIAN_POINT('Ctrl Pts',(-21.,10.2711360438186,0.847355944984259));
#56764=CARTESIAN_POINT('Ctrl Pts',(-50.,10.23508746503,1.21675444348887));
#56765=CARTESIAN_POINT('Ctrl Pts',(-21.,10.23508746503,1.21675444348887));
#56766=CARTESIAN_POINT('Ctrl Pts',(-50.,10.1645797371964,1.68895887943845));
#56767=CARTESIAN_POINT('Ctrl Pts',(-21.,10.1645797371964,1.68895887943845));
#56768=CARTESIAN_POINT('Ctrl Pts',(-50.,10.0589430297105,2.26615269674877));
#56769=CARTESIAN_POINT('Ctrl Pts',(-21.,10.0589430297105,2.26615269674877));
#56770=CARTESIAN_POINT('Ctrl Pts',(-50.,9.91789485710769,2.94928822483092));
#56771=CARTESIAN_POINT('Ctrl Pts',(-21.,9.91789485710769,2.94928822483092));
#56772=CARTESIAN_POINT('Ctrl Pts',(-50.,9.77670130881801,3.5806699311609));
#56773=CARTESIAN_POINT('Ctrl Pts',(-21.,9.77670130881801,3.5806699311609));
#56774=CARTESIAN_POINT('Ctrl Pts',(-50.,9.65489431545908,4.10184205893951));
#56775=CARTESIAN_POINT('Ctrl Pts',(-21.,9.65489431545908,4.10184205893951));
#56776=CARTESIAN_POINT('Ctrl Pts',(-50.,9.56662712803709,4.47043349004179));
#56777=CARTESIAN_POINT('Ctrl Pts',(-21.,9.56662712803709,4.47043349004179));
#56778=CARTESIAN_POINT('Ctrl Pts',(-50.,9.52072790258051,4.66001504343333));
#56779=CARTESIAN_POINT('Ctrl Pts',(-21.,9.52072790258051,4.66001504343333));
#56780=CARTESIAN_POINT('Ctrl Pts',(-66.,13.847248627403,-2.45104298226008));
#56781=CARTESIAN_POINT('Ctrl Pts',(-50.,13.847248627403,-2.45104298226008));
#56782=CARTESIAN_POINT('Ctrl Pts',(-66.,13.8704109184829,-2.45416751351779));
#56783=CARTESIAN_POINT('Ctrl Pts',(-50.,13.8704109184829,-2.45416751351779));
#56784=CARTESIAN_POINT('Ctrl Pts',(-66.,13.9167144589915,-2.46064068498796));
#56785=CARTESIAN_POINT('Ctrl Pts',(-50.,13.9167144589915,-2.46064068498796));
#56786=CARTESIAN_POINT('Ctrl Pts',(-66.,13.9861066530346,-2.47102275853729));
#56787=CARTESIAN_POINT('Ctrl Pts',(-50.,13.9861066530346,-2.47102275853729));
#56788=CARTESIAN_POINT('Ctrl Pts',(-66.,14.0785031060049,-2.48621203480011));
#56789=CARTESIAN_POINT('Ctrl Pts',(-50.,14.0785031060049,-2.48621203480011));
#56790=CARTESIAN_POINT('Ctrl Pts',(-66.,14.1937640331043,-2.50749463728168));
#56791=CARTESIAN_POINT('Ctrl Pts',(-50.,14.1937640331043,-2.50749463728168));
#56792=CARTESIAN_POINT('Ctrl Pts',(-66.,14.3087190397278,-2.53121250086624));
#56793=CARTESIAN_POINT('Ctrl Pts',(-50.,14.3087190397278,-2.53121250086624));
#56794=CARTESIAN_POINT('Ctrl Pts',(-66.,14.423228955274,-2.55762788131115));
#56795=CARTESIAN_POINT('Ctrl Pts',(-50.,14.423228955274,-2.55762788131115));
#56796=CARTESIAN_POINT('Ctrl Pts',(-66.,14.537056384215,-2.58717382256056));
#56797=CARTESIAN_POINT('Ctrl Pts',(-50.,14.537056384215,-2.58717382256056));
#56798=CARTESIAN_POINT('Ctrl Pts',(-66.,14.6499173448672,-2.62041096375855));
#56799=CARTESIAN_POINT('Ctrl Pts',(-50.,14.6499173448672,-2.62041096375855));
#56800=CARTESIAN_POINT('Ctrl Pts',(-66.,14.7615516365331,-2.65797355871958));
#56801=CARTESIAN_POINT('Ctrl Pts',(-50.,14.7615516365331,-2.65797355871958));
#56802=CARTESIAN_POINT('Ctrl Pts',(-66.,14.8717795409674,-2.70050907188802));
#56803=CARTESIAN_POINT('Ctrl Pts',(-50.,14.8717795409674,-2.70050907188802));
#56804=CARTESIAN_POINT('Ctrl Pts',(-66.,14.9805825983482,-2.74864579544975));
#56805=CARTESIAN_POINT('Ctrl Pts',(-50.,14.9805825983482,-2.74864579544975));
#56806=CARTESIAN_POINT('Ctrl Pts',(-66.,15.0880810351184,-2.80279667637514));
#56807=CARTESIAN_POINT('Ctrl Pts',(-50.,15.0880810351184,-2.80279667637514));
#56808=CARTESIAN_POINT('Ctrl Pts',(-66.,15.1944599098748,-2.86283428974206));
#56809=CARTESIAN_POINT('Ctrl Pts',(-50.,15.1944599098748,-2.86283428974206));
#56810=CARTESIAN_POINT('Ctrl Pts',(-66.,15.299916309402,-2.9278833773088));
#56811=CARTESIAN_POINT('Ctrl Pts',(-50.,15.299916309402,-2.9278833773088));
#56812=CARTESIAN_POINT('Ctrl Pts',(-66.,15.4045879562307,-2.99587287520288));
#56813=CARTESIAN_POINT('Ctrl Pts',(-50.,15.4045879562307,-2.99587287520288));
#56814=CARTESIAN_POINT('Ctrl Pts',(-66.,15.5085273245779,-3.06389197726713));
#56815=CARTESIAN_POINT('Ctrl Pts',(-50.,15.5085273245779,-3.06389197726713));
#56816=CARTESIAN_POINT('Ctrl Pts',(-66.,15.6117260024113,-3.1296030647124));
#56817=CARTESIAN_POINT('Ctrl Pts',(-50.,15.6117260024113,-3.1296030647124));
#56818=CARTESIAN_POINT('Ctrl Pts',(-66.,15.7141266693079,-3.19226978910788));
#56819=CARTESIAN_POINT('Ctrl Pts',(-50.,15.7141266693079,-3.19226978910788));
#56820=CARTESIAN_POINT('Ctrl Pts',(-66.,15.8156387361042,-3.25420659877988));
#56821=CARTESIAN_POINT('Ctrl Pts',(-50.,15.8156387361042,-3.25420659877988));
#56822=CARTESIAN_POINT('Ctrl Pts',(-66.,15.9161557197846,-3.32129162127238));
#56823=CARTESIAN_POINT('Ctrl Pts',(-50.,15.9161557197846,-3.32129162127238));
#56824=CARTESIAN_POINT('Ctrl Pts',(-66.,16.0155897253002,-3.39971935742472));
#56825=CARTESIAN_POINT('Ctrl Pts',(-50.,16.0155897253002,-3.39971935742472));
#56826=CARTESIAN_POINT('Ctrl Pts',(-66.,16.1139042055915,-3.49322345403937));
#56827=CARTESIAN_POINT('Ctrl Pts',(-50.,16.1139042055915,-3.49322345403937));
#56828=CARTESIAN_POINT('Ctrl Pts',(-66.,16.211146002486,-3.60024269640763));
#56829=CARTESIAN_POINT('Ctrl Pts',(-50.,16.211146002486,-3.60024269640763));
#56830=CARTESIAN_POINT('Ctrl Pts',(-66.,16.3074829231181,-3.71072189651349));
#56831=CARTESIAN_POINT('Ctrl Pts',(-50.,16.3074829231181,-3.71072189651349));
#56832=CARTESIAN_POINT('Ctrl Pts',(-66.,16.4031678857067,-3.80856758682422));
#56833=CARTESIAN_POINT('Ctrl Pts',(-50.,16.4031678857067,-3.80856758682422));
#56834=CARTESIAN_POINT('Ctrl Pts',(-66.,16.4984944917342,-3.87477327683275));
#56835=CARTESIAN_POINT('Ctrl Pts',(-50.,16.4984944917342,-3.87477327683275));
#56836=CARTESIAN_POINT('Ctrl Pts',(-66.,16.5937589714353,-3.89007667331238));
#56837=CARTESIAN_POINT('Ctrl Pts',(-50.,16.5937589714353,-3.89007667331238));
#56838=CARTESIAN_POINT('Ctrl Pts',(-66.,16.68921248971,-3.83831350468403));
#56839=CARTESIAN_POINT('Ctrl Pts',(-50.,16.68921248971,-3.83831350468403));
#56840=CARTESIAN_POINT('Ctrl Pts',(-66.,16.7850480556278,-3.70731931187133));
#56841=CARTESIAN_POINT('Ctrl Pts',(-50.,16.7850480556278,-3.70731931187133));
#56842=CARTESIAN_POINT('Ctrl Pts',(-66.,16.8814129124086,-3.48803104347221));
#56843=CARTESIAN_POINT('Ctrl Pts',(-50.,16.8814129124086,-3.48803104347221));
#56844=CARTESIAN_POINT('Ctrl Pts',(-66.,16.9784132750883,-3.17413405024117));
#56845=CARTESIAN_POINT('Ctrl Pts',(-50.,16.9784132750883,-3.17413405024117));
#56846=CARTESIAN_POINT('Ctrl Pts',(-66.,17.0761219213447,-2.76151077690173));
#56847=CARTESIAN_POINT('Ctrl Pts',(-50.,17.0761219213447,-2.76151077690173));
#56848=CARTESIAN_POINT('Ctrl Pts',(-66.,17.1745842847512,-2.24779890242269));
#56849=CARTESIAN_POINT('Ctrl Pts',(-50.,17.1745842847512,-2.24779890242269));
#56850=CARTESIAN_POINT('Ctrl Pts',(-66.,17.2738249451951,-1.6319247049175));
#56851=CARTESIAN_POINT('Ctrl Pts',(-50.,17.2738249451951,-1.6319247049175));
#56852=CARTESIAN_POINT('Ctrl Pts',(-66.,17.3538479729472,-1.05731872182051));
#56853=CARTESIAN_POINT('Ctrl Pts',(-50.,17.3538479729472,-1.05731872182051));
#56854=CARTESIAN_POINT('Ctrl Pts',(-66.,17.4142204208888,-0.580381911529879));
#56855=CARTESIAN_POINT('Ctrl Pts',(-50.,17.4142204208888,-0.580381911529879));
#56856=CARTESIAN_POINT('Ctrl Pts',(-66.,17.4546263659151,-0.242014631789217));
#56857=CARTESIAN_POINT('Ctrl Pts',(-50.,17.4546263659151,-0.242014631789217));
#56858=CARTESIAN_POINT('Ctrl Pts',(-66.,17.4748687500531,-0.0677286381032094));
#56859=CARTESIAN_POINT('Ctrl Pts',(-50.,17.4748687500531,-0.0677286381032094));
#56860=CARTESIAN_POINT('',(-65.5,16.4355406675768,-3.82604599612027));
#56861=CARTESIAN_POINT('Ctrl Pts',(-66.,16.017075735697,-3.40498309495743));
#56862=CARTESIAN_POINT('Ctrl Pts',(-65.7933280154027,16.1952885331162,-3.5605803063597));
#56863=CARTESIAN_POINT('Ctrl Pts',(-65.6370761749495,16.3149639463236,-3.73942475662406));
#56864=CARTESIAN_POINT('Ctrl Pts',(-65.5,16.4355406675768,-3.82604599612027));
#56865=CARTESIAN_POINT('',(-66.,13.847248627403,-2.45104298226008));
#56866=CARTESIAN_POINT('',(-50.5,16.4355406675768,-3.82604599612027));
#56867=CARTESIAN_POINT('Ctrl Pts',(-50.5,16.4355406675768,-3.82604599612027));
#56868=CARTESIAN_POINT('Ctrl Pts',(-50.4948519989264,16.4310123161643,-3.82279286891502));
#56869=CARTESIAN_POINT('Ctrl Pts',(-50.4896830984798,16.4264908162217,-3.81941633340717));
#56870=CARTESIAN_POINT('Ctrl Pts',(-50.3487582866786,16.3038396642987,-3.72461708742528));
#56871=CARTESIAN_POINT('Ctrl Pts',(-50.1996600197157,16.1892421312326,-3.55530120583648));
#56872=CARTESIAN_POINT('Ctrl Pts',(-50.,16.017075735697,-3.40498309495743));
#56873=CARTESIAN_POINT('Ctrl Pts',(-65.5,16.4355406675768,-3.82604599612027));
#56874=CARTESIAN_POINT('Ctrl Pts',(-60.5,16.4355406675768,-3.82604599612027));
#56875=CARTESIAN_POINT('Ctrl Pts',(-55.5,16.4355406675768,-3.82604599612027));
#56876=CARTESIAN_POINT('Ctrl Pts',(-50.5,16.4355406675768,-3.82604599612027));
#56877=CARTESIAN_POINT('Origin',(-66.,0.,0.));
#56878=CARTESIAN_POINT('',(-66.,14.0217614511585,-1.06963173887292));
#56879=CARTESIAN_POINT('Ctrl Pts',(-66.,17.4748687500531,-0.0677286381032094));
#56880=CARTESIAN_POINT('Ctrl Pts',(-50.,17.4748687500531,-0.0677286381032094));
#56881=CARTESIAN_POINT('Ctrl Pts',(-66.,17.4559219893477,-0.0798814582063345));
#56882=CARTESIAN_POINT('Ctrl Pts',(-50.,17.4559219893477,-0.0798814582063345));
#56883=CARTESIAN_POINT('Ctrl Pts',(-66.,17.4179952684683,-0.104043012351033));
#56884=CARTESIAN_POINT('Ctrl Pts',(-50.,17.4179952684683,-0.104043012351033));
#56885=CARTESIAN_POINT('Ctrl Pts',(-66.,17.3610055888369,-0.139853086053525));
#56886=CARTESIAN_POINT('Ctrl Pts',(-50.,17.3610055888369,-0.139853086053525));
#56887=CARTESIAN_POINT('Ctrl Pts',(-66.,17.2848198869808,-0.186734180470151));
#56888=CARTESIAN_POINT('Ctrl Pts',(-50.,17.2848198869808,-0.186734180470151));
#56889=CARTESIAN_POINT('Ctrl Pts',(-66.,17.1892542640251,-0.24388678747065));
#56890=CARTESIAN_POINT('Ctrl Pts',(-50.,17.1892542640251,-0.24388678747065));
#56891=CARTESIAN_POINT('Ctrl Pts',(-66.,17.0933546347573,-0.299584219228362));
#56892=CARTESIAN_POINT('Ctrl Pts',(-50.,17.0933546347573,-0.299584219228362));
#56893=CARTESIAN_POINT('Ctrl Pts',(-66.,16.9971220426505,-0.353822666243593));
#56894=CARTESIAN_POINT('Ctrl Pts',(-50.,16.9971220426505,-0.353822666243593));
#56895=CARTESIAN_POINT('Ctrl Pts',(-66.,16.9005600486991,-0.406603490394105));
#56896=CARTESIAN_POINT('Ctrl Pts',(-50.,16.9005600486991,-0.406603490394105));
#56897=CARTESIAN_POINT('Ctrl Pts',(-66.,16.8036759306869,-0.457937485755119));
#56898=CARTESIAN_POINT('Ctrl Pts',(-50.,16.8036759306869,-0.457937485755119));
#56899=CARTESIAN_POINT('Ctrl Pts',(-66.,16.7064800689097,-0.507835335884597));
#56900=CARTESIAN_POINT('Ctrl Pts',(-50.,16.7064800689097,-0.507835335884597));
#56901=CARTESIAN_POINT('Ctrl Pts',(-66.,16.608985095069,-0.556296581714668));
#56902=CARTESIAN_POINT('Ctrl Pts',(-50.,16.608985095069,-0.556296581714668));
#56903=CARTESIAN_POINT('Ctrl Pts',(-66.,16.5112051709817,-0.603298348866388));
#56904=CARTESIAN_POINT('Ctrl Pts',(-50.,16.5112051709817,-0.603298348866388));
#56905=CARTESIAN_POINT('Ctrl Pts',(-66.,16.4131552634766,-0.648786238597103));
#56906=CARTESIAN_POINT('Ctrl Pts',(-50.,16.4131552634766,-0.648786238597103));
#56907=CARTESIAN_POINT('Ctrl Pts',(-66.,16.3148504473396,-0.692659157159194));
#56908=CARTESIAN_POINT('Ctrl Pts',(-50.,16.3148504473396,-0.692659157159194));
#56909=CARTESIAN_POINT('Ctrl Pts',(-66.,16.2163053509993,-0.734791658433232));
#56910=CARTESIAN_POINT('Ctrl Pts',(-50.,16.2163053509993,-0.734791658433232));
#56911=CARTESIAN_POINT('Ctrl Pts',(-66.,16.1175336986507,-0.775065535573949));
#56912=CARTESIAN_POINT('Ctrl Pts',(-50.,16.1175336986507,-0.775065535573949));
#56913=CARTESIAN_POINT('Ctrl Pts',(-66.,16.018547775909,-0.813401076758624));
#56914=CARTESIAN_POINT('Ctrl Pts',(-50.,16.018547775909,-0.813401076758624));
#56915=CARTESIAN_POINT('Ctrl Pts',(-66.,15.9193580975472,-0.849783012021725));
#56916=CARTESIAN_POINT('Ctrl Pts',(-50.,15.9193580975472,-0.849783012021725));
#56917=CARTESIAN_POINT('Ctrl Pts',(-66.,15.8199726227578,-0.884304144422378));
#56918=CARTESIAN_POINT('Ctrl Pts',(-50.,15.8199726227578,-0.884304144422378));
#56919=CARTESIAN_POINT('Ctrl Pts',(-66.,15.7203984586304,-0.917113393337539));
#56920=CARTESIAN_POINT('Ctrl Pts',(-50.,15.7203984586304,-0.917113393337539));
#56921=CARTESIAN_POINT('Ctrl Pts',(-66.,15.6206443917204,-0.948332278883351));
#56922=CARTESIAN_POINT('Ctrl Pts',(-50.,15.6206443917204,-0.948332278883351));
#56923=CARTESIAN_POINT('Ctrl Pts',(-66.,15.5207233107191,-0.977976807855906));
#56924=CARTESIAN_POINT('Ctrl Pts',(-50.,15.5207233107191,-0.977976807855906));
#56925=CARTESIAN_POINT('Ctrl Pts',(-66.,15.42065441025,-1.00588830882699));
#56926=CARTESIAN_POINT('Ctrl Pts',(-50.,15.42065441025,-1.00588830882699));
#56927=CARTESIAN_POINT('Ctrl Pts',(-66.,15.3204663197849,-1.03163045186508));
#56928=CARTESIAN_POINT('Ctrl Pts',(-50.,15.3204663197849,-1.03163045186508));
#56929=CARTESIAN_POINT('Ctrl Pts',(-66.,15.2201951366894,-1.05457808085916));
#56930=CARTESIAN_POINT('Ctrl Pts',(-50.,15.2201951366894,-1.05457808085916));
#56931=CARTESIAN_POINT('Ctrl Pts',(-66.,15.1198807137451,-1.07407094658941));
#56932=CARTESIAN_POINT('Ctrl Pts',(-50.,15.1198807137451,-1.07407094658941));
#56933=CARTESIAN_POINT('Ctrl Pts',(-66.,15.0195634762927,-1.08955145679141));
#56934=CARTESIAN_POINT('Ctrl Pts',(-50.,15.0195634762927,-1.08955145679141));
#56935=CARTESIAN_POINT('Ctrl Pts',(-66.,14.9192812134642,-1.100697501046));
#56936=CARTESIAN_POINT('Ctrl Pts',(-50.,14.9192812134642,-1.100697501046));
#56937=CARTESIAN_POINT('Ctrl Pts',(-66.,14.8190654065121,-1.10759084369408));
#56938=CARTESIAN_POINT('Ctrl Pts',(-50.,14.8190654065121,-1.10759084369408));
#56939=CARTESIAN_POINT('Ctrl Pts',(-66.,14.7189411465911,-1.11063958426619));
#56940=CARTESIAN_POINT('Ctrl Pts',(-50.,14.7189411465911,-1.11063958426619));
#56941=CARTESIAN_POINT('Ctrl Pts',(-66.,14.6189280002071,-1.11043751754959));
#56942=CARTESIAN_POINT('Ctrl Pts',(-50.,14.6189280002071,-1.11043751754959));
#56943=CARTESIAN_POINT('Ctrl Pts',(-66.,14.5190405063557,-1.10764458318629));
#56944=CARTESIAN_POINT('Ctrl Pts',(-50.,14.5190405063557,-1.10764458318629));
#56945=CARTESIAN_POINT('Ctrl Pts',(-66.,14.4192887981899,-1.10286394535002));
#56946=CARTESIAN_POINT('Ctrl Pts',(-50.,14.4192887981899,-1.10286394535002));
#56947=CARTESIAN_POINT('Ctrl Pts',(-66.,14.3196790995356,-1.09650878711472));
#56948=CARTESIAN_POINT('Ctrl Pts',(-50.,14.3196790995356,-1.09650878711472));
#56949=CARTESIAN_POINT('Ctrl Pts',(-66.,14.2202146396052,-1.08882773106131));
#56950=CARTESIAN_POINT('Ctrl Pts',(-50.,14.2202146396052,-1.08882773106131));
#56951=CARTESIAN_POINT('Ctrl Pts',(-66.,14.1407601934611,-1.08172501415579));
#56952=CARTESIAN_POINT('Ctrl Pts',(-50.,14.1407601934611,-1.08172501415579));
#56953=CARTESIAN_POINT('Ctrl Pts',(-66.,14.0812352370361,-1.07587965991017));
#56954=CARTESIAN_POINT('Ctrl Pts',(-50.,14.0812352370361,-1.07587965991017));
#56955=CARTESIAN_POINT('Ctrl Pts',(-66.,14.0415811730659,-1.0717527195609));
#56956=CARTESIAN_POINT('Ctrl Pts',(-50.,14.0415811730659,-1.0717527195609));
#56957=CARTESIAN_POINT('Ctrl Pts',(-66.,14.0217614511585,-1.06963173887291));
#56958=CARTESIAN_POINT('Ctrl Pts',(-50.,14.0217614511585,-1.06963173887291));
#56959=CARTESIAN_POINT('',(-65.5,16.8697044894034,-0.422723834437671));
#56960=CARTESIAN_POINT('Ctrl Pts',(-65.5,16.8697044894034,-0.422723834437665));
#56961=CARTESIAN_POINT('Ctrl Pts',(-65.5824813699687,16.7860826756777,-0.46728689022706));
#56962=CARTESIAN_POINT('Ctrl Pts',(-65.6660554230592,16.7012035668841,-0.510709500683481));
#56963=CARTESIAN_POINT('Ctrl Pts',(-65.7497221071122,16.6161031834905,-0.552412690850408));
#56964=CARTESIAN_POINT('Ctrl Pts',(-65.8185920154888,16.5460531310298,-0.586740511037283));
#56965=CARTESIAN_POINT('Ctrl Pts',(-65.8875246877872,16.47585467524,-0.61990802303423));
#56966=CARTESIAN_POINT('Ctrl Pts',(-65.9559623561336,16.406105057495,-0.651556799133145));
#56967=CARTESIAN_POINT('Ctrl Pts',(-65.9706662645635,16.3911192752916,-0.65835657353987));
#56968=CARTESIAN_POINT('Ctrl Pts',(-65.985347323118,16.376154254472,-0.66508604655682));
#56969=CARTESIAN_POINT('Ctrl Pts',(-66.,16.3612159786808,-0.671741541784794));
#56970=CARTESIAN_POINT('',(-50.5,16.8697044894034,-0.422723834437671));
#56971=CARTESIAN_POINT('Ctrl Pts',(-50.5,16.8697044894034,-0.42272383443767));
#56972=CARTESIAN_POINT('Ctrl Pts',(-55.5,16.8697044894034,-0.42272383443767));
#56973=CARTESIAN_POINT('Ctrl Pts',(-60.5,16.8697044894034,-0.42272383443767));
#56974=CARTESIAN_POINT('Ctrl Pts',(-65.5,16.8697044894034,-0.42272383443767));
#56975=CARTESIAN_POINT('Ctrl Pts',(-50.,16.3612159786808,-0.671741541784793));
#56976=CARTESIAN_POINT('Ctrl Pts',(-50.0723811193609,16.4350078961438,-0.638864805446282));
#56977=CARTESIAN_POINT('Ctrl Pts',(-50.1454547942982,16.50945142814,-0.604185038169576));
#56978=CARTESIAN_POINT('Ctrl Pts',(-50.2185542315269,16.5838300931957,-0.568140357464802));
#56979=CARTESIAN_POINT('Ctrl Pts',(-50.3042498183568,16.6710253383469,-0.525884627705495));
#56980=CARTESIAN_POINT('Ctrl Pts',(-50.389980810899,16.7581291023942,-0.481748382293282));
#56981=CARTESIAN_POINT('Ctrl Pts',(-50.4746729118433,16.8440226549228,-0.436353334136896));
#56982=CARTESIAN_POINT('Ctrl Pts',(-50.4831259799697,16.8525956392158,-0.431822481431791));
#56983=CARTESIAN_POINT('Ctrl Pts',(-50.491568698744,16.8611566112176,-0.427279100049654));
#56984=CARTESIAN_POINT('Ctrl Pts',(-50.5,16.8697044894034,-0.422723834437666));
#56985=CARTESIAN_POINT('Origin',(-65.75,0.,0.));
#56986=CARTESIAN_POINT('',(-65.5,16.234584558964,-4.60476809381824));
#56987=CARTESIAN_POINT('Origin',(-65.5,0.,0.));
#56988=CARTESIAN_POINT('Ctrl Pts',(-65.5,16.234584558964,-4.60476809381825));
#56989=CARTESIAN_POINT('Ctrl Pts',(-65.693336649146,16.0187500351764,-4.6571980681224));
#56990=CARTESIAN_POINT('Ctrl Pts',(-65.8613255387785,15.8327432857568,-4.69365622380825));
#56991=CARTESIAN_POINT('Ctrl Pts',(-66.,15.6801429643085,-4.71950650162129));
#56992=CARTESIAN_POINT('Origin',(-58.,0.,0.));
#56993=CARTESIAN_POINT('',(-50.5,16.234584558964,-4.60476809381824));
#56994=CARTESIAN_POINT('Origin',(-50.5,0.,0.));
#56995=CARTESIAN_POINT('Ctrl Pts',(-50.5,16.234584558964,-4.60476809381824));
#56996=CARTESIAN_POINT('Ctrl Pts',(-55.5,16.234584558964,-4.60476809381824));
#56997=CARTESIAN_POINT('Ctrl Pts',(-60.5,16.234584558964,-4.60476809381825));
#56998=CARTESIAN_POINT('Ctrl Pts',(-65.5,16.234584558964,-4.60476809381825));
#56999=CARTESIAN_POINT('Origin',(-50.25,0.,0.));
#57000=CARTESIAN_POINT('Ctrl Pts',(-50.,15.6801429643085,-4.71950650162129));
#57001=CARTESIAN_POINT('Ctrl Pts',(-50.1386744612147,15.8327432857494,-4.69365622380952));
#57002=CARTESIAN_POINT('Ctrl Pts',(-50.3066633508514,16.0187500351735,-4.65719806812311));
#57003=CARTESIAN_POINT('Ctrl Pts',(-50.5,16.234584558964,-4.60476809381824));
#57004=CARTESIAN_POINT('Ctrl Pts',(-66.,12.8026622457696,-5.81770965851216));
#57005=CARTESIAN_POINT('Ctrl Pts',(-50.,12.8026622457696,-5.81770965851216));
#57006=CARTESIAN_POINT('Ctrl Pts',(-66.,12.8243198115569,-5.82649625442995));
#57007=CARTESIAN_POINT('Ctrl Pts',(-50.,12.8243198115569,-5.82649625442995));
#57008=CARTESIAN_POINT('Ctrl Pts',(-66.,12.8675588289116,-5.84428128157946));
#57009=CARTESIAN_POINT('Ctrl Pts',(-50.,12.8675588289116,-5.84428128157946));
#57010=CARTESIAN_POINT('Ctrl Pts',(-66.,12.932189022876,-5.87159432010365));
#57011=CARTESIAN_POINT('Ctrl Pts',(-50.,12.932189022876,-5.87159432010365));
#57012=CARTESIAN_POINT('Ctrl Pts',(-66.,13.0179052519711,-5.90928446078516));
#57013=CARTESIAN_POINT('Ctrl Pts',(-50.,13.0179052519711,-5.90928446078516));
#57014=CARTESIAN_POINT('Ctrl Pts',(-66.,13.124252277086,-5.95856265812867));
#57015=CARTESIAN_POINT('Ctrl Pts',(-50.,13.124252277086,-5.95856265812867));
#57016=CARTESIAN_POINT('Ctrl Pts',(-66.,13.2296973679703,-6.01012352904084));
#57017=CARTESIAN_POINT('Ctrl Pts',(-50.,13.2296973679703,-6.01012352904084));
#57018=CARTESIAN_POINT('Ctrl Pts',(-66.,13.3340405059683,-6.06418647971103));
#57019=CARTESIAN_POINT('Ctrl Pts',(-50.,13.3340405059683,-6.06418647971103));
#57020=CARTESIAN_POINT('Ctrl Pts',(-66.,13.4369440601197,-6.12111191134452));
#57021=CARTESIAN_POINT('Ctrl Pts',(-50.,13.4369440601197,-6.12111191134452));
#57022=CARTESIAN_POINT('Ctrl Pts',(-66.,13.537993545262,-6.18137222620287));
#57023=CARTESIAN_POINT('Ctrl Pts',(-50.,13.537993545262,-6.18137222620287));
#57024=CARTESIAN_POINT('Ctrl Pts',(-66.,13.6367792028716,-6.24551704256852));
#57025=CARTESIAN_POINT('Ctrl Pts',(-50.,13.6367792028716,-6.24551704256852));
#57026=CARTESIAN_POINT('Ctrl Pts',(-66.,13.7329659430228,-6.31412878948963));
#57027=CARTESIAN_POINT('Ctrl Pts',(-50.,13.7329659430228,-6.31412878948963));
#57028=CARTESIAN_POINT('Ctrl Pts',(-66.,13.8263796359301,-6.38781142942664));
#57029=CARTESIAN_POINT('Ctrl Pts',(-50.,13.8263796359301,-6.38781142942664));
#57030=CARTESIAN_POINT('Ctrl Pts',(-66.,13.9170340351662,-6.46699483496205));
#57031=CARTESIAN_POINT('Ctrl Pts',(-50.,13.9170340351662,-6.46699483496205));
#57032=CARTESIAN_POINT('Ctrl Pts',(-66.,14.0051400746611,-6.55160160666348));
#57033=CARTESIAN_POINT('Ctrl Pts',(-50.,14.0051400746611,-6.55160160666348));
#57034=CARTESIAN_POINT('Ctrl Pts',(-66.,14.0911063172293,-6.64083299762664));
#57035=CARTESIAN_POINT('Ctrl Pts',(-50.,14.0911063172293,-6.64083299762664));
#57036=CARTESIAN_POINT('Ctrl Pts',(-66.,14.1755812112355,-6.73271726045961));
#57037=CARTESIAN_POINT('Ctrl Pts',(-50.,14.1755812112355,-6.73271726045961));
#57038=CARTESIAN_POINT('Ctrl Pts',(-66.,14.2593394703776,-6.8244480871404));
#57039=CARTESIAN_POINT('Ctrl Pts',(-50.,14.2593394703776,-6.8244480871404));
#57040=CARTESIAN_POINT('Ctrl Pts',(-66.,14.3429542890555,-6.9137592074853));
#57041=CARTESIAN_POINT('Ctrl Pts',(-50.,14.3429542890555,-6.9137592074853));
#57042=CARTESIAN_POINT('Ctrl Pts',(-66.,14.426553270081,-6.99992315179396));
#57043=CARTESIAN_POINT('Ctrl Pts',(-50.,14.426553270081,-6.99992315179396));
#57044=CARTESIAN_POINT('Ctrl Pts',(-66.,14.5094730904225,-7.08515912713373));
#57045=CARTESIAN_POINT('Ctrl Pts',(-50.,14.5094730904225,-7.08515912713373));
#57046=CARTESIAN_POINT('Ctrl Pts',(-66.,14.5901487815487,-7.17513410761352));
#57047=CARTESIAN_POINT('Ctrl Pts',(-50.,14.5901487815487,-7.17513410761352));
#57048=CARTESIAN_POINT('Ctrl Pts',(-66.,14.6669547000804,-7.27582612382816));
#57049=CARTESIAN_POINT('Ctrl Pts',(-50.,14.6669547000804,-7.27582612382816));
#57050=CARTESIAN_POINT('Ctrl Pts',(-66.,14.7389269269491,-7.39084243431597));
#57051=CARTESIAN_POINT('Ctrl Pts',(-50.,14.7389269269491,-7.39084243431597));
#57052=CARTESIAN_POINT('Ctrl Pts',(-66.,14.80649909067,-7.51868252188801));
#57053=CARTESIAN_POINT('Ctrl Pts',(-50.,14.80649909067,-7.51868252188801));
#57054=CARTESIAN_POINT('Ctrl Pts',(-66.,14.8723343499808,-7.64964883268732));
#57055=CARTESIAN_POINT('Ctrl Pts',(-50.,14.8723343499808,-7.64964883268732));
#57056=CARTESIAN_POINT('Ctrl Pts',(-66.,14.9406799598344,-7.76821640326081));
#57057=CARTESIAN_POINT('Ctrl Pts',(-50.,14.9406799598344,-7.76821640326081));
#57058=CARTESIAN_POINT('Ctrl Pts',(-66.,15.0165470196623,-7.85604888267077));
#57059=CARTESIAN_POINT('Ctrl Pts',(-50.,15.0165470196623,-7.85604888267077));
#57060=CARTESIAN_POINT('Ctrl Pts',(-66.,15.1050127906107,-7.8945628075167));
#57061=CARTESIAN_POINT('Ctrl Pts',(-50.,15.1050127906107,-7.8945628075167));
#57062=CARTESIAN_POINT('Ctrl Pts',(-66.,15.2103404376476,-7.86816419870585));
#57063=CARTESIAN_POINT('Ctrl Pts',(-50.,15.2103404376476,-7.86816419870585));
#57064=CARTESIAN_POINT('Ctrl Pts',(-66.,15.3357420840626,-7.76511876541631));
#57065=CARTESIAN_POINT('Ctrl Pts',(-50.,15.3357420840626,-7.76511876541631));
#57066=CARTESIAN_POINT('Ctrl Pts',(-66.,15.4836142363898,-7.57668480657135));
#57067=CARTESIAN_POINT('Ctrl Pts',(-50.,15.4836142363898,-7.57668480657135));
#57068=CARTESIAN_POINT('Ctrl Pts',(-66.,15.6556301621328,-7.29677247384862));
#57069=CARTESIAN_POINT('Ctrl Pts',(-50.,15.6556301621328,-7.29677247384862));
#57070=CARTESIAN_POINT('Ctrl Pts',(-66.,15.8528843468817,-6.92141167161478));
#57071=CARTESIAN_POINT('Ctrl Pts',(-50.,15.8528843468817,-6.92141167161478));
#57072=CARTESIAN_POINT('Ctrl Pts',(-66.,16.0760082821817,-6.44832559436811));
#57073=CARTESIAN_POINT('Ctrl Pts',(-50.,16.0760082821817,-6.44832559436811));
#57074=CARTESIAN_POINT('Ctrl Pts',(-66.,16.3252927994722,-5.87648036593892));
#57075=CARTESIAN_POINT('Ctrl Pts',(-50.,16.3252927994722,-5.87648036593892));
#57076=CARTESIAN_POINT('Ctrl Pts',(-66.,16.545700453756,-5.33982760416968));
#57077=CARTESIAN_POINT('Ctrl Pts',(-50.,16.545700453756,-5.33982760416968));
#57078=CARTESIAN_POINT('Ctrl Pts',(-66.,16.7227855517644,-4.89288865806624));
#57079=CARTESIAN_POINT('Ctrl Pts',(-50.,16.7227855517644,-4.89288865806624));
#57080=CARTESIAN_POINT('Ctrl Pts',(-66.,16.8460705903453,-4.57520035854192));
#57081=CARTESIAN_POINT('Ctrl Pts',(-50.,16.8460705903453,-4.57520035854192));
#57082=CARTESIAN_POINT('Ctrl Pts',(-66.,16.9090201868666,-4.41142395606429));
#57083=CARTESIAN_POINT('Ctrl Pts',(-50.,16.9090201868666,-4.41142395606429));
#57084=CARTESIAN_POINT('',(-65.5,14.967688987597,-7.79319647965878));
#57085=CARTESIAN_POINT('Ctrl Pts',(-66.,14.6670849864349,-7.28129404712485));
#57086=CARTESIAN_POINT('Ctrl Pts',(-65.793328015403,14.8010034481658,-7.47632260648893));
#57087=CARTESIAN_POINT('Ctrl Pts',(-65.6370761749494,14.8724422320436,-7.67931039448365));
#57088=CARTESIAN_POINT('Ctrl Pts',(-65.5,14.9676889875971,-7.79319647965879));
#57089=CARTESIAN_POINT('',(-66.,12.8026622457696,-5.81770965851216));
#57090=CARTESIAN_POINT('',(-50.5,14.9676889875971,-7.79319647965878));
#57091=CARTESIAN_POINT('Ctrl Pts',(-50.5,14.967688987597,-7.79319647965878));
#57092=CARTESIAN_POINT('Ctrl Pts',(-50.4506066448269,14.933368239824,-7.75215932745924));
#57093=CARTESIAN_POINT('Ctrl Pts',(-50.3985811798094,14.9019662355384,-7.699722088817));
#57094=CARTESIAN_POINT('Ctrl Pts',(-50.2410584360541,14.8108032651412,-7.53250027576706));
#57095=CARTESIAN_POINT('Ctrl Pts',(-50.1348334000372,14.7544537778951,-7.40853124289031));
#57096=CARTESIAN_POINT('Ctrl Pts',(-50.,14.6670849864349,-7.28129404712485));
#57097=CARTESIAN_POINT('Ctrl Pts',(-65.5,14.967688987597,-7.79319647965878));
#57098=CARTESIAN_POINT('Ctrl Pts',(-60.5,14.967688987597,-7.79319647965878));
#57099=CARTESIAN_POINT('Ctrl Pts',(-55.5,14.967688987597,-7.79319647965878));
#57100=CARTESIAN_POINT('Ctrl Pts',(-50.5,14.967688987597,-7.79319647965878));
#57101=CARTESIAN_POINT('Origin',(-66.,0.,0.));
#57102=CARTESIAN_POINT('',(-66.,13.3152354345065,-4.52309756402218));
#57103=CARTESIAN_POINT('Ctrl Pts',(-66.,16.9090201868666,-4.41142395606429));
#57104=CARTESIAN_POINT('Ctrl Pts',(-50.,16.9090201868666,-4.41142395606429));
#57105=CARTESIAN_POINT('Ctrl Pts',(-66.,16.8876463900293,-4.41848310519446));
#57106=CARTESIAN_POINT('Ctrl Pts',(-50.,16.8876463900293,-4.41848310519446));
#57107=CARTESIAN_POINT('Ctrl Pts',(-66.,16.8449024726547,-4.43245358774968));
#57108=CARTESIAN_POINT('Ctrl Pts',(-50.,16.8449024726547,-4.43245358774968));
#57109=CARTESIAN_POINT('Ctrl Pts',(-66.,16.7807976254172,-4.4529658651396));
#57110=CARTESIAN_POINT('Ctrl Pts',(-50.,16.7807976254172,-4.4529658651396));
#57111=CARTESIAN_POINT('Ctrl Pts',(-66.,16.6953465834,-4.47942749016865));
#57112=CARTESIAN_POINT('Ctrl Pts',(-50.,16.6953465834,-4.47942749016865));
#57113=CARTESIAN_POINT('Ctrl Pts',(-66.,16.5885700548362,-4.51101833893424));
#57114=CARTESIAN_POINT('Ctrl Pts',(-50.,16.5885700548362,-4.51101833893424));
#57115=CARTESIAN_POINT('Ctrl Pts',(-66.,16.4818319007497,-4.54111666547111));
#57116=CARTESIAN_POINT('Ctrl Pts',(-50.,16.4818319007497,-4.54111666547111));
#57117=CARTESIAN_POINT('Ctrl Pts',(-66.,16.3751340792151,-4.56971903946321));
#57118=CARTESIAN_POINT('Ctrl Pts',(-50.,16.3751340792151,-4.56971903946321));
#57119=CARTESIAN_POINT('Ctrl Pts',(-66.,16.2684797006663,-4.5968276655857));
#57120=CARTESIAN_POINT('Ctrl Pts',(-50.,16.2684797006663,-4.5968276655857));
#57121=CARTESIAN_POINT('Ctrl Pts',(-66.,16.1618731298649,-4.62245480870932));
#57122=CARTESIAN_POINT('Ctrl Pts',(-50.,16.1618731298649,-4.62245480870932));
#57123=CARTESIAN_POINT('Ctrl Pts',(-66.,16.0553217640976,-4.64661339822299));
#57124=CARTESIAN_POINT('Ctrl Pts',(-50.,16.0553217640976,-4.64661339822299));
#57125=CARTESIAN_POINT('Ctrl Pts',(-66.,15.9488379523835,-4.66930613085772));
#57126=CARTESIAN_POINT('Ctrl Pts',(-50.,15.9488379523835,-4.66930613085772));
#57127=CARTESIAN_POINT('Ctrl Pts',(-66.,15.8424411002465,-4.6905143727759));
#57128=CARTESIAN_POINT('Ctrl Pts',(-50.,15.8424411002465,-4.6905143727759));
#57129=CARTESIAN_POINT('Ctrl Pts',(-66.,15.7361592327224,-4.71018915637038));
#57130=CARTESIAN_POINT('Ctrl Pts',(-50.,15.7361592327224,-4.71018915637038));
#57131=CARTESIAN_POINT('Ctrl Pts',(-66.,15.6300320919874,-4.72823631288632));
#57132=CARTESIAN_POINT('Ctrl Pts',(-50.,15.6300320919874,-4.72823631288632));
#57133=CARTESIAN_POINT('Ctrl Pts',(-66.,15.5241050440726,-4.74453797526706));
#57134=CARTESIAN_POINT('Ctrl Pts',(-50.,15.5241050440726,-4.74453797526706));
#57135=CARTESIAN_POINT('Ctrl Pts',(-66.,15.418420778849,-4.75898306342126));
#57136=CARTESIAN_POINT('Ctrl Pts',(-50.,15.418420778849,-4.75898306342126));
#57137=CARTESIAN_POINT('Ctrl Pts',(-66.,15.3130110194811,-4.77149742512795));
#57138=CARTESIAN_POINT('Ctrl Pts',(-50.,15.3130110194811,-4.77149742512795));
#57139=CARTESIAN_POINT('Ctrl Pts',(-66.,15.2078897478867,-4.78206888507335));
#57140=CARTESIAN_POINT('Ctrl Pts',(-50.,15.2078897478867,-4.78206888507335));
#57141=CARTESIAN_POINT('Ctrl Pts',(-66.,15.1030415940234,-4.79078931010852));
#57142=CARTESIAN_POINT('Ctrl Pts',(-50.,15.1030415940234,-4.79078931010852));
#57143=CARTESIAN_POINT('Ctrl Pts',(-66.,14.9984364069554,-4.79780470849564));
#57144=CARTESIAN_POINT('Ctrl Pts',(-50.,14.9984364069554,-4.79780470849564));
#57145=CARTESIAN_POINT('Ctrl Pts',(-66.,14.8940524763685,-4.80323496770043));
#57146=CARTESIAN_POINT('Ctrl Pts',(-50.,14.8940524763685,-4.80323496770043));
#57147=CARTESIAN_POINT('Ctrl Pts',(-66.,14.7898983053036,-4.80709879692323));
#57148=CARTESIAN_POINT('Ctrl Pts',(-50.,14.7898983053036,-4.80709879692323));
#57149=CARTESIAN_POINT('Ctrl Pts',(-66.,14.6860319453295,-4.80924728319928));
#57150=CARTESIAN_POINT('Ctrl Pts',(-50.,14.6860319453295,-4.80924728319928));
#57151=CARTESIAN_POINT('Ctrl Pts',(-66.,14.5825896373118,-4.80926492456431));
#57152=CARTESIAN_POINT('Ctrl Pts',(-50.,14.5825896373118,-4.80926492456431));
#57153=CARTESIAN_POINT('Ctrl Pts',(-66.,14.4797618145538,-4.80655518238588));
#57154=CARTESIAN_POINT('Ctrl Pts',(-50.,14.4797618145538,-4.80655518238588));
#57155=CARTESIAN_POINT('Ctrl Pts',(-66.,14.3777512750926,-4.80048846137132));
#57156=CARTESIAN_POINT('Ctrl Pts',(-50.,14.3777512750926,-4.80048846137132));
#57157=CARTESIAN_POINT('Ctrl Pts',(-66.,14.27673584179,-4.79053474041595));
#57158=CARTESIAN_POINT('Ctrl Pts',(-50.,14.27673584179,-4.79053474041595));
#57159=CARTESIAN_POINT('Ctrl Pts',(-66.,14.1768322221664,-4.77639142656668));
#57160=CARTESIAN_POINT('Ctrl Pts',(-50.,14.1768322221664,-4.77639142656668));
#57161=CARTESIAN_POINT('Ctrl Pts',(-66.,14.0780505744683,-4.75814554445644));
#57162=CARTESIAN_POINT('Ctrl Pts',(-50.,14.0780505744683,-4.75814554445644));
#57163=CARTESIAN_POINT('Ctrl Pts',(-66.,13.9803137113395,-4.73619861233502));
#57164=CARTESIAN_POINT('Ctrl Pts',(-50.,13.9803137113395,-4.73619861233502));
#57165=CARTESIAN_POINT('Ctrl Pts',(-66.,13.8834929138094,-4.71113063582666));
#57166=CARTESIAN_POINT('Ctrl Pts',(-50.,13.8834929138094,-4.71113063582666));
#57167=CARTESIAN_POINT('Ctrl Pts',(-66.,13.7874381437893,-4.68358443705714));
#57168=CARTESIAN_POINT('Ctrl Pts',(-50.,13.7874381437893,-4.68358443705714));
#57169=CARTESIAN_POINT('Ctrl Pts',(-66.,13.6920092152502,-4.65414675070122));
#57170=CARTESIAN_POINT('Ctrl Pts',(-50.,13.6920092152502,-4.65414675070122));
#57171=CARTESIAN_POINT('Ctrl Pts',(-66.,13.5971094020329,-4.62321932672933));
#57172=CARTESIAN_POINT('Ctrl Pts',(-50.,13.5971094020329,-4.62321932672933));
#57173=CARTESIAN_POINT('Ctrl Pts',(-66.,13.5026800019769,-4.59104377985933));
#57174=CARTESIAN_POINT('Ctrl Pts',(-50.,13.5026800019769,-4.59104377985933));
#57175=CARTESIAN_POINT('Ctrl Pts',(-66.,13.4274881372306,-4.56440469062003));
#57176=CARTESIAN_POINT('Ctrl Pts',(-50.,13.4274881372306,-4.56440469062003));
#57177=CARTESIAN_POINT('Ctrl Pts',(-66.,13.3712869472582,-4.54393972423008));
#57178=CARTESIAN_POINT('Ctrl Pts',(-50.,13.3712869472582,-4.54393972423008));
#57179=CARTESIAN_POINT('Ctrl Pts',(-66.,13.3339050169562,-4.53008087460641));
#57180=CARTESIAN_POINT('Ctrl Pts',(-50.,13.3339050169562,-4.53008087460641));
#57181=CARTESIAN_POINT('Ctrl Pts',(-66.,13.3152354345065,-4.52309756402217));
#57182=CARTESIAN_POINT('Ctrl Pts',(-50.,13.3152354345065,-4.52309756402217));
#57183=CARTESIAN_POINT('Origin',(-65.75,0.,0.));
#57184=CARTESIAN_POINT('',(-65.5,14.5793859740595,-8.49747783871179));
#57185=CARTESIAN_POINT('Origin',(-65.5,0.,0.));
#57186=CARTESIAN_POINT('Ctrl Pts',(-65.5,14.5793859740595,-8.49747783871179));
#57187=CARTESIAN_POINT('Ctrl Pts',(-65.6931595476758,14.3574969269134,-8.49458741572547));
#57188=CARTESIAN_POINT('Ctrl Pts',(-65.8611256967112,14.1682859702542,-8.48365813109589));
#57189=CARTESIAN_POINT('Ctrl Pts',(-66.,14.0138288999568,-8.47072751083015));
#57190=CARTESIAN_POINT('Origin',(-58.,0.,0.));
#57191=CARTESIAN_POINT('',(-50.5,14.5793859740595,-8.49747783871179));
#57192=CARTESIAN_POINT('Origin',(-50.5,0.,0.));
#57193=CARTESIAN_POINT('Ctrl Pts',(-50.5,14.5793859740595,-8.49747783871179));
#57194=CARTESIAN_POINT('Ctrl Pts',(-55.5,14.5793859740595,-8.49747783871179));
#57195=CARTESIAN_POINT('Ctrl Pts',(-60.5,14.5793859740595,-8.49747783871179));
#57196=CARTESIAN_POINT('Ctrl Pts',(-65.5,14.5793859740595,-8.49747783871179));
#57197=CARTESIAN_POINT('Origin',(-50.25,0.,0.));
#57198=CARTESIAN_POINT('Ctrl Pts',(-50.,14.0138288999568,-8.47072751083015));
#57199=CARTESIAN_POINT('Ctrl Pts',(-50.1388743032911,14.1682859702568,-8.48365813109611));
#57200=CARTESIAN_POINT('Ctrl Pts',(-50.3068404523263,14.3574969269158,-8.49458741572551));
#57201=CARTESIAN_POINT('Ctrl Pts',(-50.5,14.5793859740595,-8.49747783871179));
#57202=CARTESIAN_POINT('Ctrl Pts',(-66.,10.9536375103364,-8.81882824088046));
#57203=CARTESIAN_POINT('Ctrl Pts',(-50.,10.9536375103364,-8.81882824088046));
#57204=CARTESIAN_POINT('Ctrl Pts',(-66.,10.9724295263217,-8.83272480732197));
#57205=CARTESIAN_POINT('Ctrl Pts',(-50.,10.9724295263217,-8.83272480732197));
#57206=CARTESIAN_POINT('Ctrl Pts',(-66.,11.0098871540402,-8.86070419148627));
#57207=CARTESIAN_POINT('Ctrl Pts',(-50.,11.0098871540402,-8.86070419148627));
#57208=CARTESIAN_POINT('Ctrl Pts',(-66.,11.0656943951459,-8.90323201632451));
#57209=CARTESIAN_POINT('Ctrl Pts',(-50.,11.0656943951459,-8.90323201632451));
#57210=CARTESIAN_POINT('Ctrl Pts',(-66.,11.1393445344495,-8.96105481127105));
#57211=CARTESIAN_POINT('Ctrl Pts',(-50.,11.1393445344495,-8.96105481127105));
#57212=CARTESIAN_POINT('Ctrl Pts',(-66.,11.2300954828748,-9.03523227310488));
#57213=CARTESIAN_POINT('Ctrl Pts',(-50.,11.2300954828748,-9.03523227310488));
#57214=CARTESIAN_POINT('Ctrl Pts',(-66.,11.3194051551598,-9.11139639219764));
#57215=CARTESIAN_POINT('Ctrl Pts',(-50.,11.3194051551598,-9.11139639219764));
#57216=CARTESIAN_POINT('Ctrl Pts',(-66.,11.407025252502,-9.18970993907287));
#57217=CARTESIAN_POINT('Ctrl Pts',(-50.,11.407025252502,-9.18970993907287));
#57218=CARTESIAN_POINT('Ctrl Pts',(-66.,11.4925391231036,-9.27043802686381));
#57219=CARTESIAN_POINT('Ctrl Pts',(-50.,11.4925391231036,-9.27043802686381));
#57220=CARTESIAN_POINT('Ctrl Pts',(-66.,11.5754278219505,-9.35393513817802));
#57221=CARTESIAN_POINT('Ctrl Pts',(-50.,11.5754278219505,-9.35393513817802));
#57222=CARTESIAN_POINT('Ctrl Pts',(-66.,11.655157779328,-9.44063172122792));
#57223=CARTESIAN_POINT('Ctrl Pts',(-50.,11.655157779328,-9.44063172122792));
#57224=CARTESIAN_POINT('Ctrl Pts',(-66.,11.7312595885623,-9.53100857350628));
#57225=CARTESIAN_POINT('Ctrl Pts',(-50.,11.7312595885623,-9.53100857350628));
#57226=CARTESIAN_POINT('Ctrl Pts',(-66.,11.8034143911192,-9.62560737856555));
#57227=CARTESIAN_POINT('Ctrl Pts',(-50.,11.8034143911192,-9.62560737856555));
#57228=CARTESIAN_POINT('Ctrl Pts',(-66.,11.8715286035136,-9.724847924125));
#57229=CARTESIAN_POINT('Ctrl Pts',(-50.,11.8715286035136,-9.724847924125));
#57230=CARTESIAN_POINT('Ctrl Pts',(-66.,11.9358257812543,-9.82870769953299));
#57231=CARTESIAN_POINT('Ctrl Pts',(-50.,11.9358257812543,-9.82870769953299));
#57232=CARTESIAN_POINT('Ctrl Pts',(-66.,11.9969002916812,-9.93651465742827));
#57233=CARTESIAN_POINT('Ctrl Pts',(-50.,11.9969002916812,-9.93651465742827));
#57234=CARTESIAN_POINT('Ctrl Pts',(-66.,12.0558705645975,-10.0465202590396));
#57235=CARTESIAN_POINT('Ctrl Pts',(-50.,12.0558705645975,-10.0465202590396));
#57236=CARTESIAN_POINT('Ctrl Pts',(-66.,12.1141848750712,-10.1561990251342));
#57237=CARTESIAN_POINT('Ctrl Pts',(-50.,12.1141848750712,-10.1561990251342));
#57238=CARTESIAN_POINT('Ctrl Pts',(-66.,12.1729620080223,-10.2634984322242));
#57239=CARTESIAN_POINT('Ctrl Pts',(-50.,12.1729620080223,-10.2634984322242));
#57240=CARTESIAN_POINT('Ctrl Pts',(-66.,12.2325064717433,-10.3677455989363));
#57241=CARTESIAN_POINT('Ctrl Pts',(-50.,12.2325064717433,-10.3677455989363));
#57242=CARTESIAN_POINT('Ctrl Pts',(-66.,12.2916238883603,-10.4709250501372));
#57243=CARTESIAN_POINT('Ctrl Pts',(-50.,12.2916238883603,-10.4709250501372));
#57244=CARTESIAN_POINT('Ctrl Pts',(-66.,12.3473891365543,-10.5781365296759));
#57245=CARTESIAN_POINT('Ctrl Pts',(-50.,12.3473891365543,-10.5781365296759));
#57246=CARTESIAN_POINT('Ctrl Pts',(-66.,12.3967409697684,-10.6947659762548));
#57247=CARTESIAN_POINT('Ctrl Pts',(-50.,12.3967409697684,-10.6947659762548));
#57248=CARTESIAN_POINT('Ctrl Pts',(-66.,12.437848663505,-10.8240676028274));
#57249=CARTESIAN_POINT('Ctrl Pts',(-50.,12.437848663505,-10.8240676028274));
#57250=CARTESIAN_POINT('Ctrl Pts',(-66.,12.4715053864926,-10.9646958727381));
#57251=CARTESIAN_POINT('Ctrl Pts',(-50.,12.4715053864926,-10.9646958727381));
#57252=CARTESIAN_POINT('Ctrl Pts',(-66.,12.5027023130146,-11.107920199263));
#57253=CARTESIAN_POINT('Ctrl Pts',(-50.,12.5027023130146,-11.107920199263));
#57254=CARTESIAN_POINT('Ctrl Pts',(-66.,12.5394141641085,-11.239759613579));
#57255=CARTESIAN_POINT('Ctrl Pts',(-50.,12.5394141641085,-11.239759613579));
#57256=CARTESIAN_POINT('Ctrl Pts',(-66.,12.5910546713482,-11.3437000446838));
#57257=CARTESIAN_POINT('Ctrl Pts',(-50.,12.5910546713482,-11.3437000446838));
#57258=CARTESIAN_POINT('Ctrl Pts',(-66.,12.6671631038009,-11.4030045263537));
#57259=CARTESIAN_POINT('Ctrl Pts',(-50.,12.6671631038009,-11.4030045263537));
#57260=CARTESIAN_POINT('Ctrl Pts',(-66.,12.7757467561686,-11.4036291990392));
#57261=CARTESIAN_POINT('Ctrl Pts',(-50.,12.7757467561686,-11.4036291990392));
#57262=CARTESIAN_POINT('Ctrl Pts',(-66.,12.9228350364417,-11.335007248821));
#57263=CARTESIAN_POINT('Ctrl Pts',(-50.,12.9228350364417,-11.335007248821));
#57264=CARTESIAN_POINT('Ctrl Pts',(-66.,13.1129231331489,-11.1892675981761));
#57265=CARTESIAN_POINT('Ctrl Pts',(-50.,13.1129231331489,-11.1892675981761));
#57266=CARTESIAN_POINT('Ctrl Pts',(-66.,13.3491462287103,-10.9609278472722));
#57267=CARTESIAN_POINT('Ctrl Pts',(-50.,13.3491462287103,-10.9609278472722));
#57268=CARTESIAN_POINT('Ctrl Pts',(-66.,13.6335517460739,-10.6464148158287));
#57269=CARTESIAN_POINT('Ctrl Pts',(-50.,13.6335517460739,-10.6464148158287));
#57270=CARTESIAN_POINT('Ctrl Pts',(-66.,13.9673175558199,-10.2436802739367));
#57271=CARTESIAN_POINT('Ctrl Pts',(-50.,13.9673175558199,-10.2436802739367));
#57272=CARTESIAN_POINT('Ctrl Pts',(-66.,14.3509824669314,-9.75179515338539));
#57273=CARTESIAN_POINT('Ctrl Pts',(-50.,14.3509824669314,-9.75179515338539));
#57274=CARTESIAN_POINT('Ctrl Pts',(-66.,14.6979257242257,-9.28681547963666));
#57275=CARTESIAN_POINT('Ctrl Pts',(-50.,14.6979257242257,-9.28681547963666));
#57276=CARTESIAN_POINT('Ctrl Pts',(-66.,14.9805965643194,-8.89795721543056));
#57277=CARTESIAN_POINT('Ctrl Pts',(-50.,14.9805965643194,-8.89795721543056));
#57278=CARTESIAN_POINT('Ctrl Pts',(-66.,15.1790142440703,-8.62090942035752));
#57279=CARTESIAN_POINT('Ctrl Pts',(-50.,15.1790142440703,-8.62090942035752));
#57280=CARTESIAN_POINT('Ctrl Pts',(-66.,15.2807156983131,-8.47793328278342));
#57281=CARTESIAN_POINT('Ctrl Pts',(-50.,15.2807156983131,-8.47793328278342));
#57282=CARTESIAN_POINT('',(-65.5,12.5593623612171,-11.2706717670086));
#57283=CARTESIAN_POINT('Ctrl Pts',(-66.,12.3955073457098,-10.7000945155851));
#57284=CARTESIAN_POINT('Ctrl Pts',(-65.7933280154029,12.4767168822844,-10.9223000612616));
#57285=CARTESIAN_POINT('Ctrl Pts',(-65.6370761749496,12.4954302753076,-11.1366767177294));
#57286=CARTESIAN_POINT('Ctrl Pts',(-65.5,12.5593623612171,-11.2706717670086));
#57287=CARTESIAN_POINT('',(-66.,10.9536375103364,-8.81882824088046));
#57288=CARTESIAN_POINT('',(-50.5,12.5593623612171,-11.2706717670086));
#57289=CARTESIAN_POINT('Ctrl Pts',(-50.5,12.5593623612171,-11.2706717670086));
#57290=CARTESIAN_POINT('Ctrl Pts',(-50.4518618349124,12.5369108060359,-11.2236156261038));
#57291=CARTESIAN_POINT('Ctrl Pts',(-50.4012423593889,12.5198465875944,-11.1667793509398));
#57292=CARTESIAN_POINT('Ctrl Pts',(-50.2441129793807,12.4729367680423,-10.982980939431));
#57293=CARTESIAN_POINT('Ctrl Pts',(-50.1366827452944,12.449215362424,-10.847050398657));
#57294=CARTESIAN_POINT('Ctrl Pts',(-50.,12.3955073457098,-10.7000945155851));
#57295=CARTESIAN_POINT('Ctrl Pts',(-65.5,12.5593623612171,-11.2706717670086));
#57296=CARTESIAN_POINT('Ctrl Pts',(-60.5,12.5593623612171,-11.2706717670086));
#57297=CARTESIAN_POINT('Ctrl Pts',(-55.5,12.5593623612171,-11.2706717670086));
#57298=CARTESIAN_POINT('Ctrl Pts',(-50.5,12.5593623612171,-11.2706717670086));
#57299=CARTESIAN_POINT('Origin',(-66.,0.,0.));
#57300=CARTESIAN_POINT('',(-66.,11.7720642054939,-7.6923605344347));
#57301=CARTESIAN_POINT('Ctrl Pts',(-66.,15.2807156983131,-8.47793328278342));
#57302=CARTESIAN_POINT('Ctrl Pts',(-50.,15.2807156983131,-8.47793328278342));
#57303=CARTESIAN_POINT('Ctrl Pts',(-66.,15.2582578596065,-8.47945520863905));
#57304=CARTESIAN_POINT('Ctrl Pts',(-50.,15.2582578596065,-8.47945520863905));
#57305=CARTESIAN_POINT('Ctrl Pts',(-66.,15.2133825032665,-8.482356802806));
#57306=CARTESIAN_POINT('Ctrl Pts',(-50.,15.2133825032665,-8.482356802806));
#57307=CARTESIAN_POINT('Ctrl Pts',(-66.,15.1461904317359,-8.48628242205606));
#57308=CARTESIAN_POINT('Ctrl Pts',(-50.,15.1461904317359,-8.48628242205606));
#57309=CARTESIAN_POINT('Ctrl Pts',(-66.,15.0568432527945,-8.49066189647792));
#57310=CARTESIAN_POINT('Ctrl Pts',(-50.,15.0568432527945,-8.49066189647792));
#57311=CARTESIAN_POINT('Ctrl Pts',(-66.,14.9455649806088,-8.49470601779764));
#57312=CARTESIAN_POINT('Ctrl Pts',(-50.,14.9455649806088,-8.49470601779764));
#57313=CARTESIAN_POINT('Ctrl Pts',(-66.,14.8346950524804,-8.49731405056346));
#57314=CARTESIAN_POINT('Ctrl Pts',(-50.,14.8346950524804,-8.49731405056346));
#57315=CARTESIAN_POINT('Ctrl Pts',(-66.,14.7242362180521,-8.49848315918232));
#57316=CARTESIAN_POINT('Ctrl Pts',(-50.,14.7242362180521,-8.49848315918232));
#57317=CARTESIAN_POINT('Ctrl Pts',(-66.,14.6141909417575,-8.49821625259896));
#57318=CARTESIAN_POINT('Ctrl Pts',(-50.,14.6141909417575,-8.49821625259896));
#57319=CARTESIAN_POINT('Ctrl Pts',(-66.,14.5045604010818,-8.49652629583269));
#57320=CARTESIAN_POINT('Ctrl Pts',(-50.,14.5045604010818,-8.49652629583269));
#57321=CARTESIAN_POINT('Ctrl Pts',(-66.,14.3953485455042,-8.49342765170233));
#57322=CARTESIAN_POINT('Ctrl Pts',(-50.,14.3953485455042,-8.49342765170233));
#57323=CARTESIAN_POINT('Ctrl Pts',(-66.,14.2865666654267,-8.48892600329226));
#57324=CARTESIAN_POINT('Ctrl Pts',(-50.,14.2865666654267,-8.48892600329226));
#57325=CARTESIAN_POINT('Ctrl Pts',(-66.,14.1782381907602,-8.48300812813872));
#57326=CARTESIAN_POINT('Ctrl Pts',(-50.,14.1782381907602,-8.48300812813872));
#57327=CARTESIAN_POINT('Ctrl Pts',(-66.,14.0704024438309,-8.47563356658493));
#57328=CARTESIAN_POINT('Ctrl Pts',(-50.,14.0704024438309,-8.47563356658493));
#57329=CARTESIAN_POINT('Ctrl Pts',(-66.,13.9631213370587,-8.46672099183801));
#57330=CARTESIAN_POINT('Ctrl Pts',(-50.,13.9631213370587,-8.46672099183801));
#57331=CARTESIAN_POINT('Ctrl Pts',(-66.,13.8564681235622,-8.45616752192477));
#57332=CARTESIAN_POINT('Ctrl Pts',(-50.,13.8564681235622,-8.45616752192477));
#57333=CARTESIAN_POINT('Ctrl Pts',(-66.,13.7505117765273,-8.44387618307839));
#57334=CARTESIAN_POINT('Ctrl Pts',(-50.,13.7505117765273,-8.44387618307839));
#57335=CARTESIAN_POINT('Ctrl Pts',(-66.,13.6453014633841,-8.42978304193647));
#57336=CARTESIAN_POINT('Ctrl Pts',(-50.,13.6453014633841,-8.42978304193647));
#57337=CARTESIAN_POINT('Ctrl Pts',(-66.,13.5408537546603,-8.41387978285669));
#57338=CARTESIAN_POINT('Ctrl Pts',(-50.,13.5408537546603,-8.41387978285669));
#57339=CARTESIAN_POINT('Ctrl Pts',(-66.,13.4371309168349,-8.39625156414993));
#57340=CARTESIAN_POINT('Ctrl Pts',(-50.,13.4371309168349,-8.39625156414993));
#57341=CARTESIAN_POINT('Ctrl Pts',(-66.,13.3340674354409,-8.37703230872753));
#57342=CARTESIAN_POINT('Ctrl Pts',(-50.,13.3340674354409,-8.37703230872753));
#57343=CARTESIAN_POINT('Ctrl Pts',(-66.,13.231612467433,-8.35633273843435));
#57344=CARTESIAN_POINT('Ctrl Pts',(-50.,13.231612467433,-8.35633273843435));
#57345=CARTESIAN_POINT('Ctrl Pts',(-66.,13.1297695959248,-8.33417308930716));
#57346=CARTESIAN_POINT('Ctrl Pts',(-50.,13.1297695959248,-8.33417308930716));
#57347=CARTESIAN_POINT('Ctrl Pts',(-66.,13.0286320818366,-8.31042356359388));
#57348=CARTESIAN_POINT('Ctrl Pts',(-50.,13.0286320818366,-8.31042356359388));
#57349=CARTESIAN_POINT('Ctrl Pts',(-66.,12.9284352169133,-8.284715594814));
#57350=CARTESIAN_POINT('Ctrl Pts',(-50.,12.9284352169133,-8.284715594814));
#57351=CARTESIAN_POINT('Ctrl Pts',(-66.,12.829511804771,-8.25651874452987));
#57352=CARTESIAN_POINT('Ctrl Pts',(-50.,12.829511804771,-8.25651874452987));
#57353=CARTESIAN_POINT('Ctrl Pts',(-66.,12.7322148461558,-8.22527363116368));
#57354=CARTESIAN_POINT('Ctrl Pts',(-50.,12.7322148461558,-8.22527363116368));
#57355=CARTESIAN_POINT('Ctrl Pts',(-66.,12.636848388186,-8.19051110794578));
#57356=CARTESIAN_POINT('Ctrl Pts',(-50.,12.636848388186,-8.19051110794578));
#57357=CARTESIAN_POINT('Ctrl Pts',(-66.,12.5436007236081,-8.15196711241727));
#57358=CARTESIAN_POINT('Ctrl Pts',(-50.,12.5436007236081,-8.15196711241727));
#57359=CARTESIAN_POINT('Ctrl Pts',(-66.,12.4524600493824,-8.10972846142537));
#57360=CARTESIAN_POINT('Ctrl Pts',(-50.,12.4524600493824,-8.10972846142537));
#57361=CARTESIAN_POINT('Ctrl Pts',(-66.,12.3632517496072,-8.06416486307078));
#57362=CARTESIAN_POINT('Ctrl Pts',(-50.,12.3632517496072,-8.06416486307078));
#57363=CARTESIAN_POINT('Ctrl Pts',(-66.,12.2757069077219,-8.01580608992824));
#57364=CARTESIAN_POINT('Ctrl Pts',(-50.,12.2757069077219,-8.01580608992824));
#57365=CARTESIAN_POINT('Ctrl Pts',(-66.,12.1895203359981,-7.96523745572904));
#57366=CARTESIAN_POINT('Ctrl Pts',(-50.,12.1895203359981,-7.96523745572904));
#57367=CARTESIAN_POINT('Ctrl Pts',(-66.,12.1044103376288,-7.91299239895144));
#57368=CARTESIAN_POINT('Ctrl Pts',(-50.,12.1044103376288,-7.91299239895144));
#57369=CARTESIAN_POINT('Ctrl Pts',(-66.,12.0201833141302,-7.85943599303422));
#57370=CARTESIAN_POINT('Ctrl Pts',(-50.,12.0201833141302,-7.85943599303422));
#57371=CARTESIAN_POINT('Ctrl Pts',(-66.,11.936722320441,-7.80478766329085));
#57372=CARTESIAN_POINT('Ctrl Pts',(-50.,11.936722320441,-7.80478766329085));
#57373=CARTESIAN_POINT('Ctrl Pts',(-66.,11.870517618491,-7.7602860336664));
#57374=CARTESIAN_POINT('Ctrl Pts',(-50.,11.870517618491,-7.7602860336664));
#57375=CARTESIAN_POINT('Ctrl Pts',(-66.,11.8211715224307,-7.72648734423527));
#57376=CARTESIAN_POINT('Ctrl Pts',(-50.,11.8211715224307,-7.72648734423527));
#57377=CARTESIAN_POINT('Ctrl Pts',(-66.,11.7884105699588,-7.70376738782835));
#57378=CARTESIAN_POINT('Ctrl Pts',(-50.,11.7884105699588,-7.70376738782835));
#57379=CARTESIAN_POINT('Ctrl Pts',(-66.,11.7720642054939,-7.69236053443469));
#57380=CARTESIAN_POINT('Ctrl Pts',(-50.,11.7720642054939,-7.69236053443469));
#57381=CARTESIAN_POINT('Origin',(-65.75,0.,0.));
#57382=CARTESIAN_POINT('',(-65.5,12.0081109491739,-11.8562597994617));
#57383=CARTESIAN_POINT('Origin',(-65.5,0.,0.));
#57384=CARTESIAN_POINT('Ctrl Pts',(-65.5,12.0081109491739,-11.8562597994617));
#57385=CARTESIAN_POINT('Ctrl Pts',(-65.6931595476832,11.7939117734275,-11.7982786223285));
#57386=CARTESIAN_POINT('Ctrl Pts',(-65.8611256967229,11.6133632294635,-11.7406378498091));
#57387=CARTESIAN_POINT('Ctrl Pts',(-66.,11.4669744265634,-11.689701557377));
#57388=CARTESIAN_POINT('Origin',(-58.,0.,0.));
#57389=CARTESIAN_POINT('',(-50.5,12.0081109491739,-11.8562597994617));
#57390=CARTESIAN_POINT('Origin',(-50.5,0.,0.));
#57391=CARTESIAN_POINT('Ctrl Pts',(-50.5,12.0081109491739,-11.8562597994617));
#57392=CARTESIAN_POINT('Ctrl Pts',(-55.5,12.0081109491739,-11.8562597994617));
#57393=CARTESIAN_POINT('Ctrl Pts',(-60.5,12.0081109491739,-11.8562597994617));
#57394=CARTESIAN_POINT('Ctrl Pts',(-65.5,12.0081109491739,-11.8562597994617));
#57395=CARTESIAN_POINT('Origin',(-50.25,0.,0.));
#57396=CARTESIAN_POINT('Ctrl Pts',(-50.,11.4669744265634,-11.689701557377));
#57397=CARTESIAN_POINT('Ctrl Pts',(-50.1388743032958,11.6133632294832,-11.740637849816));
#57398=CARTESIAN_POINT('Ctrl Pts',(-50.3068404523301,11.7939117734422,-11.7982786223325));
#57399=CARTESIAN_POINT('Ctrl Pts',(-50.5,12.0081109491739,-11.8562597994617));
#57400=CARTESIAN_POINT('Ctrl Pts',(-66.,8.41635544546801,-11.2658274114927));
#57401=CARTESIAN_POINT('Ctrl Pts',(-50.,8.41635544546801,-11.2658274114927));
#57402=CARTESIAN_POINT('Ctrl Pts',(-66.,8.43110114017464,-11.2839607760805));
#57403=CARTESIAN_POINT('Ctrl Pts',(-50.,8.43110114017464,-11.2839607760805));
#57404=CARTESIAN_POINT('Ctrl Pts',(-66.,8.46042377774785,-11.3203764696515));
#57405=CARTESIAN_POINT('Ctrl Pts',(-50.,8.46042377774785,-11.3203764696515));
#57406=CARTESIAN_POINT('Ctrl Pts',(-66.,8.50390149179148,-11.3754469011628));
#57407=CARTESIAN_POINT('Ctrl Pts',(-50.,8.50390149179148,-11.3754469011628));
#57408=CARTESIAN_POINT('Ctrl Pts',(-66.,8.56085783218497,-11.4497691315105));
#57409=CARTESIAN_POINT('Ctrl Pts',(-50.,8.56085783218497,-11.4497691315105));
#57410=CARTESIAN_POINT('Ctrl Pts',(-66.,8.63031048807256,-11.544185015102));
#57411=CARTESIAN_POINT('Ctrl Pts',(-50.,8.63031048807256,-11.544185015102));
#57412=CARTESIAN_POINT('Ctrl Pts',(-66.,8.69787308659046,-11.6401667106607));
#57413=CARTESIAN_POINT('Ctrl Pts',(-50.,8.69787308659046,-11.6401667106607));
#57414=CARTESIAN_POINT('Ctrl Pts',(-66.,8.76326465031677,-11.7378101255738));
#57415=CARTESIAN_POINT('Ctrl Pts',(-50.,8.76326465031677,-11.7378101255738));
#57416=CARTESIAN_POINT('Ctrl Pts',(-66.,8.8260156863806,-11.8372684268691));
#57417=CARTESIAN_POINT('Ctrl Pts',(-50.,8.8260156863806,-11.8372684268691));
#57418=CARTESIAN_POINT('Ctrl Pts',(-66.,8.88553539714026,-11.9387559040544));
#57419=CARTESIAN_POINT('Ctrl Pts',(-50.,8.88553539714026,-11.9387559040544));
#57420=CARTESIAN_POINT('Ctrl Pts',(-66.,8.94119992783734,-12.0425567886278));
#57421=CARTESIAN_POINT('Ctrl Pts',(-50.,8.94119992783734,-12.0425567886278));
#57422=CARTESIAN_POINT('Ctrl Pts',(-66.,8.99243504959771,-12.149020036252));
#57423=CARTESIAN_POINT('Ctrl Pts',(-50.,8.99243504959771,-12.149020036252));
#57424=CARTESIAN_POINT('Ctrl Pts',(-66.,9.03879721019277,-12.2585910156016));
#57425=CARTESIAN_POINT('Ctrl Pts',(-50.,9.03879721019277,-12.2585910156016));
#57426=CARTESIAN_POINT('Ctrl Pts',(-66.,9.08009136927418,-12.3716530527263));
#57427=CARTESIAN_POINT('Ctrl Pts',(-50.,9.08009136927418,-12.3716530527263));
#57428=CARTESIAN_POINT('Ctrl Pts',(-66.,9.11653965711474,-12.4882399401825));
#57429=CARTESIAN_POINT('Ctrl Pts',(-50.,9.11653965711474,-12.4882399401825));
#57430=CARTESIAN_POINT('Ctrl Pts',(-66.,9.14888489929381,-12.6078485573591));
#57431=CARTESIAN_POINT('Ctrl Pts',(-50.,9.14888489929381,-12.6078485573591));
#57432=CARTESIAN_POINT('Ctrl Pts',(-66.,9.17864523199547,-12.7290634412273));
#57433=CARTESIAN_POINT('Ctrl Pts',(-50.,9.17864523199547,-12.7290634412273));
#57434=CARTESIAN_POINT('Ctrl Pts',(-66.,9.20785149120868,-12.8497986264917));
#57435=CARTESIAN_POINT('Ctrl Pts',(-50.,9.20785149120868,-12.8497986264917));
#57436=CARTESIAN_POINT('Ctrl Pts',(-66.,9.23809775500251,-12.9683443039596));
#57437=CARTESIAN_POINT('Ctrl Pts',(-50.,9.23809775500251,-12.9683443039596));
#57438=CARTESIAN_POINT('Ctrl Pts',(-66.,9.26984630377419,-13.0841244601964));
#57439=CARTESIAN_POINT('Ctrl Pts',(-50.,9.26984630377419,-13.0841244601964));
#57440=CARTESIAN_POINT('Ctrl Pts',(-66.,9.30144675196197,-13.1987642428721));
#57441=CARTESIAN_POINT('Ctrl Pts',(-50.,9.30144675196197,-13.1987642428721));
#57442=CARTESIAN_POINT('Ctrl Pts',(-66.,9.32879762158958,-13.316475729914));
#57443=CARTESIAN_POINT('Ctrl Pts',(-50.,9.32879762158958,-13.316475729914));
#57444=CARTESIAN_POINT('Ctrl Pts',(-66.,9.34759441230173,-13.4417143497954));
#57445=CARTESIAN_POINT('Ctrl Pts',(-50.,9.34759441230173,-13.4417143497954));
#57446=CARTESIAN_POINT('Ctrl Pts',(-66.,9.35525462532529,-13.5771767957172));
#57447=CARTESIAN_POINT('Ctrl Pts',(-50.,9.35525462532529,-13.5771767957172));
#57448=CARTESIAN_POINT('Ctrl Pts',(-66.,9.35288113189361,-13.7217570565735));
#57449=CARTESIAN_POINT('Ctrl Pts',(-50.,9.35288113189361,-13.7217570565735));
#57450=CARTESIAN_POINT('Ctrl Pts',(-66.,9.34747950799902,-13.8682400876461));
#57451=CARTESIAN_POINT('Ctrl Pts',(-50.,9.34747950799902,-13.8682400876461));
#57452=CARTESIAN_POINT('Ctrl Pts',(-66.,9.35025085971223,-14.0050673904318));
#57453=CARTESIAN_POINT('Ctrl Pts',(-50.,9.35025085971223,-14.0050673904318));
#57454=CARTESIAN_POINT('Ctrl Pts',(-66.,9.37442005137349,-14.118584813679));
#57455=CARTESIAN_POINT('Ctrl Pts',(-50.,9.37442005137349,-14.118584813679));
#57456=CARTESIAN_POINT('Ctrl Pts',(-66.,9.43338897261223,-14.1949535334828));
#57457=CARTESIAN_POINT('Ctrl Pts',(-50.,9.43338897261223,-14.1949535334828));
#57458=CARTESIAN_POINT('Ctrl Pts',(-66.,9.53840592008975,-14.2225622371825));
#57459=CARTESIAN_POINT('Ctrl Pts',(-50.,9.53840592008975,-14.2225622371825));
#57460=CARTESIAN_POINT('Ctrl Pts',(-66.,9.69793873661838,-14.1926755395417));
#57461=CARTESIAN_POINT('Ctrl Pts',(-50.,9.69793873661838,-14.1926755395417));
#57462=CARTESIAN_POINT('Ctrl Pts',(-66.,9.9182988434943,-14.0987875553398));
#57463=CARTESIAN_POINT('Ctrl Pts',(-50.,9.9182988434943,-14.0987875553398));
#57464=CARTESIAN_POINT('Ctrl Pts',(-66.,10.2038863430123,-13.9363678125788));
#57465=CARTESIAN_POINT('Ctrl Pts',(-50.,10.2038863430123,-13.9363678125788));
#57466=CARTESIAN_POINT('Ctrl Pts',(-66.,10.5575729483643,-13.7024645623894));
#57467=CARTESIAN_POINT('Ctrl Pts',(-50.,10.5575729483643,-13.7024645623894));
#57468=CARTESIAN_POINT('Ctrl Pts',(-66.,10.9810088992253,-13.3953868482732));
#57469=CARTESIAN_POINT('Ctrl Pts',(-50.,10.9810088992253,-13.3953868482732));
#57470=CARTESIAN_POINT('Ctrl Pts',(-66.,11.4749471267718,-13.0143687867509));
#57471=CARTESIAN_POINT('Ctrl Pts',(-50.,11.4749471267718,-13.0143687867509));
#57472=CARTESIAN_POINT('Ctrl Pts',(-66.,11.9266262662527,-12.6502785839999));
#57473=CARTESIAN_POINT('Ctrl Pts',(-50.,11.9266262662527,-12.6502785839999));
#57474=CARTESIAN_POINT('Ctrl Pts',(-66.,12.2971215999581,-12.3439343965519));
#57475=CARTESIAN_POINT('Ctrl Pts',(-50.,12.2971215999581,-12.3439343965519));
#57476=CARTESIAN_POINT('Ctrl Pts',(-66.,12.558204608331,-12.1249350378051));
#57477=CARTESIAN_POINT('Ctrl Pts',(-50.,12.558204608331,-12.1249350378051));
#57478=CARTESIAN_POINT('Ctrl Pts',(-66.,12.6922676438934,-12.0117428816877));
#57479=CARTESIAN_POINT('Ctrl Pts',(-50.,12.6922676438934,-12.0117428816877));
#57480=CARTESIAN_POINT('',(-65.5,9.3618848075781,-14.039969296606));
#57481=CARTESIAN_POINT('Ctrl Pts',(-66.,9.34507439096662,-13.4465686934362));
#57482=CARTESIAN_POINT('Ctrl Pts',(-65.7933280154029,9.36847230853418,-13.6819892337753));
#57483=CARTESIAN_POINT('Ctrl Pts',(-65.6370761749495,9.33328447939624,-13.8942846849687));
#57484=CARTESIAN_POINT('Ctrl Pts',(-65.5,9.3618848075781,-14.039969296606));
#57485=CARTESIAN_POINT('',(-66.,8.41635544546801,-11.2658274114927));
#57486=CARTESIAN_POINT('',(-50.5,9.3618848075781,-14.039969296606));
#57487=CARTESIAN_POINT('Ctrl Pts',(-50.5,9.3618848075781,-14.039969296606));
#57488=CARTESIAN_POINT('Ctrl Pts',(-50.4518618349121,9.35184099566044,-13.9888080361729));
#57489=CARTESIAN_POINT('Ctrl Pts',(-50.4012423593883,9.34944748787756,-13.9295136785486));
#57490=CARTESIAN_POINT('Ctrl Pts',(-50.2441129793799,9.34972023278718,-13.7398236343874));
#57491=CARTESIAN_POINT('Ctrl Pts',(-50.1366827452941,9.36054862959424,-13.6022643278246));
#57492=CARTESIAN_POINT('Ctrl Pts',(-50.,9.34507439096662,-13.4465686934362));
#57493=CARTESIAN_POINT('Ctrl Pts',(-65.5,9.3618848075781,-14.039969296606));
#57494=CARTESIAN_POINT('Ctrl Pts',(-60.5,9.3618848075781,-14.039969296606));
#57495=CARTESIAN_POINT('Ctrl Pts',(-55.5,9.3618848075781,-14.039969296606));
#57496=CARTESIAN_POINT('Ctrl Pts',(-50.5,9.3618848075781,-14.039969296606));
#57497=CARTESIAN_POINT('Origin',(-66.,0.,0.));
#57498=CARTESIAN_POINT('',(-66.,9.48921088782657,-10.3782842019456));
#57499=CARTESIAN_POINT('Ctrl Pts',(-66.,12.6922676438934,-12.0117428816877));
#57500=CARTESIAN_POINT('Ctrl Pts',(-50.,12.6922676438934,-12.0117428816877));
#57501=CARTESIAN_POINT('Ctrl Pts',(-66.,12.6701368719175,-12.00763195607));
#57502=CARTESIAN_POINT('Ctrl Pts',(-50.,12.6701368719175,-12.00763195607));
#57503=CARTESIAN_POINT('Ctrl Pts',(-66.,12.625949760291,-11.9992823440159));
#57504=CARTESIAN_POINT('Ctrl Pts',(-50.,12.625949760291,-11.9992823440159));
#57505=CARTESIAN_POINT('Ctrl Pts',(-66.,12.5598923894368,-11.9863746440312));
#57506=CARTESIAN_POINT('Ctrl Pts',(-50.,12.5598923894368,-11.9863746440312));
#57507=CARTESIAN_POINT('Ctrl Pts',(-66.,12.4722630854199,-11.9683967893614));
#57508=CARTESIAN_POINT('Ctrl Pts',(-50.,12.4722630854199,-11.9683967893614));
#57509=CARTESIAN_POINT('Ctrl Pts',(-66.,12.3634750927067,-11.9446400762195));
#57510=CARTESIAN_POINT('Ctrl Pts',(-50.,12.3634750927067,-11.9446400762195));
#57511=CARTESIAN_POINT('Ctrl Pts',(-66.,12.2554397558718,-11.9195939429239));
#57512=CARTESIAN_POINT('Ctrl Pts',(-50.,12.2554397558718,-11.9195939429239));
#57513=CARTESIAN_POINT('Ctrl Pts',(-66.,12.1481604433561,-11.8932563267753));
#57514=CARTESIAN_POINT('Ctrl Pts',(-50.,12.1481604433561,-11.8932563267753));
#57515=CARTESIAN_POINT('Ctrl Pts',(-66.,12.0416388187435,-11.8656306582083));
#57516=CARTESIAN_POINT('Ctrl Pts',(-50.,12.0416388187435,-11.8656306582083));
#57517=CARTESIAN_POINT('Ctrl Pts',(-66.,11.9358727982571,-11.836729787751));
#57518=CARTESIAN_POINT('Ctrl Pts',(-50.,11.9358727982571,-11.836729787751));
#57519=CARTESIAN_POINT('Ctrl Pts',(-66.,11.8308626354082,-11.8065686091834));
#57520=CARTESIAN_POINT('Ctrl Pts',(-50.,11.8308626354082,-11.8065686091834));
#57521=CARTESIAN_POINT('Ctrl Pts',(-66.,11.7266178525644,-11.775155434854));
#57522=CARTESIAN_POINT('Ctrl Pts',(-50.,11.7266178525644,-11.775155434854));
#57523=CARTESIAN_POINT('Ctrl Pts',(-66.,11.6231644318358,-11.7424832844891));
#57524=CARTESIAN_POINT('Ctrl Pts',(-50.,11.6231644318358,-11.7424832844891));
#57525=CARTESIAN_POINT('Ctrl Pts',(-66.,11.520550522073,-11.7085227486112));
#57526=CARTESIAN_POINT('Ctrl Pts',(-50.,11.520550522073,-11.7085227486112));
#57527=CARTESIAN_POINT('Ctrl Pts',(-66.,11.4188563157544,-11.6732104524509));
#57528=CARTESIAN_POINT('Ctrl Pts',(-50.,11.4188563157544,-11.6732104524509));
#57529=CARTESIAN_POINT('Ctrl Pts',(-66.,11.3181783503234,-11.6364649635713));
#57530=CARTESIAN_POINT('Ctrl Pts',(-50.,11.3181783503234,-11.6364649635713));
#57531=CARTESIAN_POINT('Ctrl Pts',(-66.,11.2186075484415,-11.5982095077484));
#57532=CARTESIAN_POINT('Ctrl Pts',(-50.,11.2186075484415,-11.5982095077484));
#57533=CARTESIAN_POINT('Ctrl Pts',(-66.,11.1202074324343,-11.5583943876468));
#57534=CARTESIAN_POINT('Ctrl Pts',(-50.,11.1202074324343,-11.5583943876468));
#57535=CARTESIAN_POINT('Ctrl Pts',(-66.,11.0229961202521,-11.5170156697979));
#57536=CARTESIAN_POINT('Ctrl Pts',(-50.,11.0229961202521,-11.5170156697979));
#57537=CARTESIAN_POINT('Ctrl Pts',(-66.,10.926915885831,-11.4741464531626));
#57538=CARTESIAN_POINT('Ctrl Pts',(-50.,10.926915885831,-11.4741464531626));
#57539=CARTESIAN_POINT('Ctrl Pts',(-66.,10.8318699676878,-11.4299001604323));
#57540=CARTESIAN_POINT('Ctrl Pts',(-50.,10.8318699676878,-11.4299001604323));
#57541=CARTESIAN_POINT('Ctrl Pts',(-66.,10.737781584702,-11.3843713907704));
#57542=CARTESIAN_POINT('Ctrl Pts',(-50.,10.737781584702,-11.3843713907704));
#57543=CARTESIAN_POINT('Ctrl Pts',(-66.,10.6446491749193,-11.3375806355454));
#57544=CARTESIAN_POINT('Ctrl Pts',(-50.,10.6446491749193,-11.3375806355454));
#57545=CARTESIAN_POINT('Ctrl Pts',(-66.,10.5525953486849,-11.289425367888));
#57546=CARTESIAN_POINT('Ctrl Pts',(-50.,10.5525953486849,-11.289425367888));
#57547=CARTESIAN_POINT('Ctrl Pts',(-66.,10.4619396643774,-11.2396071151889));
#57548=CARTESIAN_POINT('Ctrl Pts',(-50.,10.4619396643774,-11.2396071151889));
#57549=CARTESIAN_POINT('Ctrl Pts',(-66.,10.3731363846505,-11.1876948686032));
#57550=CARTESIAN_POINT('Ctrl Pts',(-50.,10.3731363846505,-11.1876948686032));
#57551=CARTESIAN_POINT('Ctrl Pts',(-66.,10.2866665326243,-11.1332346082697));
#57552=CARTESIAN_POINT('Ctrl Pts',(-50.,10.2866665326243,-11.1332346082697));
#57553=CARTESIAN_POINT('Ctrl Pts',(-66.,10.2029412752749,-11.0758475399707));
#57554=CARTESIAN_POINT('Ctrl Pts',(-50.,10.2029412752749,-11.0758475399707));
#57555=CARTESIAN_POINT('Ctrl Pts',(-66.,10.1222086594491,-11.0153247237569));
#57556=CARTESIAN_POINT('Ctrl Pts',(-50.,10.1222086594491,-11.0153247237569));
#57557=CARTESIAN_POINT('Ctrl Pts',(-66.,10.0444356624493,-10.951747313668));
#57558=CARTESIAN_POINT('Ctrl Pts',(-50.,10.0444356624493,-10.951747313668));
#57559=CARTESIAN_POINT('Ctrl Pts',(-66.,9.9693612115878,-10.885429977536));
#57560=CARTESIAN_POINT('Ctrl Pts',(-50.,9.9693612115878,-10.885429977536));
#57561=CARTESIAN_POINT('Ctrl Pts',(-66.,9.89659308973021,-10.816818967327));
#57562=CARTESIAN_POINT('Ctrl Pts',(-50.,9.89659308973021,-10.816818967327));
#57563=CARTESIAN_POINT('Ctrl Pts',(-66.,9.82569013557624,-10.7464053109633));
#57564=CARTESIAN_POINT('Ctrl Pts',(-50.,9.82569013557624,-10.7464053109633));
#57565=CARTESIAN_POINT('Ctrl Pts',(-66.,9.75624684158698,-10.6746356328252));
#57566=CARTESIAN_POINT('Ctrl Pts',(-50.,9.75624684158698,-10.6746356328252));
#57567=CARTESIAN_POINT('Ctrl Pts',(-66.,9.68798490145875,-10.6018153909131));
#57568=CARTESIAN_POINT('Ctrl Pts',(-50.,9.68798490145875,-10.6018153909131));
#57569=CARTESIAN_POINT('Ctrl Pts',(-66.,9.62073647531797,-10.5281280338367));
#57570=CARTESIAN_POINT('Ctrl Pts',(-50.,9.62073647531797,-10.5281280338367));
#57571=CARTESIAN_POINT('Ctrl Pts',(-66.,9.56767882107163,-10.4685600648819));
#57572=CARTESIAN_POINT('Ctrl Pts',(-50.,9.56767882107163,-10.4685600648819));
#57573=CARTESIAN_POINT('Ctrl Pts',(-66.,9.52828841562115,-10.4235513483695));
#57574=CARTESIAN_POINT('Ctrl Pts',(-50.,9.52828841562115,-10.4235513483695));
#57575=CARTESIAN_POINT('Ctrl Pts',(-66.,9.50220693210954,-10.3933978635985));
#57576=CARTESIAN_POINT('Ctrl Pts',(-50.,9.50220693210954,-10.3933978635985));
#57577=CARTESIAN_POINT('Ctrl Pts',(-66.,9.48921088782658,-10.3782842019456));
#57578=CARTESIAN_POINT('Ctrl Pts',(-50.,9.48921088782658,-10.3782842019456));
#57579=CARTESIAN_POINT('Origin',(-65.75,0.,0.));
#57580=CARTESIAN_POINT('',(-65.5,8.6823221506088,-14.470069352738));
#57581=CARTESIAN_POINT('Origin',(-65.5,0.,0.));
#57582=CARTESIAN_POINT('Ctrl Pts',(-65.5,8.68232215060881,-14.470069352738));
#57583=CARTESIAN_POINT('Ctrl Pts',(-65.6931595476828,8.4892717682525,-14.3606405920574));
#57584=CARTESIAN_POINT('Ctrl Pts',(-65.8611256967192,8.32873016601974,-14.2599101133766));
#57585=CARTESIAN_POINT('Ctrl Pts',(-66.,8.19960777736701,-14.1741686633588));
#57586=CARTESIAN_POINT('Origin',(-58.,0.,0.));
#57587=CARTESIAN_POINT('',(-50.5,8.68232215060881,-14.470069352738));
#57588=CARTESIAN_POINT('Origin',(-50.5,0.,0.));
#57589=CARTESIAN_POINT('Ctrl Pts',(-50.5,8.6823221506088,-14.470069352738));
#57590=CARTESIAN_POINT('Ctrl Pts',(-55.5,8.6823221506088,-14.470069352738));
#57591=CARTESIAN_POINT('Ctrl Pts',(-60.5,8.68232215060881,-14.470069352738));
#57592=CARTESIAN_POINT('Ctrl Pts',(-65.5,8.68232215060881,-14.470069352738));
#57593=CARTESIAN_POINT('Origin',(-50.25,0.,0.));
#57594=CARTESIAN_POINT('Ctrl Pts',(-50.,8.199607777367,-14.1741686633588));
#57595=CARTESIAN_POINT('Ctrl Pts',(-50.1388743032879,8.32873016602638,-14.259910113381));
#57596=CARTESIAN_POINT('Ctrl Pts',(-50.3068404523237,8.48927176825896,-14.3606405920611));
#57597=CARTESIAN_POINT('Ctrl Pts',(-50.5,8.6823221506088,-14.470069352738));
#57598=CARTESIAN_POINT('Ctrl Pts',(-66.,5.35024281477071,-13.004953213026));
#57599=CARTESIAN_POINT('Ctrl Pts',(-50.,5.35024281477071,-13.004953213026));
#57600=CARTESIAN_POINT('Ctrl Pts',(-66.,5.36001566196946,-13.026183989773));
#57601=CARTESIAN_POINT('Ctrl Pts',(-50.,5.36001566196946,-13.026183989773));
#57602=CARTESIAN_POINT('Ctrl Pts',(-66.,5.37936086023753,-13.0687478607962));
#57603=CARTESIAN_POINT('Ctrl Pts',(-50.,5.37936086023753,-13.0687478607962));
#57604=CARTESIAN_POINT('Ctrl Pts',(-66.,5.40777718254589,-13.1329006212338));
#57605=CARTESIAN_POINT('Ctrl Pts',(-50.,5.40777718254589,-13.1329006212338));
#57606=CARTESIAN_POINT('Ctrl Pts',(-66.,5.44446094769152,-13.2190523479119));
#57607=CARTESIAN_POINT('Ctrl Pts',(-50.,5.44446094769152,-13.2190523479119));
#57608=CARTESIAN_POINT('Ctrl Pts',(-66.,5.48825134524296,-13.3277741560577));
#57609=CARTESIAN_POINT('Ctrl Pts',(-50.,5.48825134524296,-13.3277741560577));
#57610=CARTESIAN_POINT('Ctrl Pts',(-66.,5.52982166345111,-13.4375425451545));
#57611=CARTESIAN_POINT('Ctrl Pts',(-50.,5.52982166345111,-13.4375425451545));
#57612=CARTESIAN_POINT('Ctrl Pts',(-66.,5.56887590111916,-13.548380533239));
#57613=CARTESIAN_POINT('Ctrl Pts',(-50.,5.56887590111916,-13.548380533239));
#57614=CARTESIAN_POINT('Ctrl Pts',(-66.,5.60492122426722,-13.6603197171863));
#57615=CARTESIAN_POINT('Ctrl Pts',(-50.,5.60492122426722,-13.6603197171863));
#57616=CARTESIAN_POINT('Ctrl Pts',(-66.,5.63733210461441,-13.7734207288063));
#57617=CARTESIAN_POINT('Ctrl Pts',(-50.,5.63733210461441,-13.7734207288063));
#57618=CARTESIAN_POINT('Ctrl Pts',(-66.,5.66543360144756,-13.8878037235725));
#57619=CARTESIAN_POINT('Ctrl Pts',(-50.,5.66543360144756,-13.8878037235725));
#57620=CARTESIAN_POINT('Ctrl Pts',(-66.,5.68858274460417,-14.0036638891498));
#57621=CARTESIAN_POINT('Ctrl Pts',(-50.,5.68858274460417,-14.0036638891498));
#57622=CARTESIAN_POINT('Ctrl Pts',(-66.,5.7062391581791,-14.1213222951832));
#57623=CARTESIAN_POINT('Ctrl Pts',(-50.,5.7062391581791,-14.1213222951832));
#57624=CARTESIAN_POINT('Ctrl Pts',(-66.,5.71811860006313,-14.2411017202677));
#57625=CARTESIAN_POINT('Ctrl Pts',(-50.,5.71811860006313,-14.2411017202677));
#57626=CARTESIAN_POINT('Ctrl Pts',(-66.,5.7244278180311,-14.3630901368566));
#57627=CARTESIAN_POINT('Ctrl Pts',(-50.,5.7244278180311,-14.3630901368566));
#57628=CARTESIAN_POINT('Ctrl Pts',(-66.,5.72601142143879,-14.4869849640075));
#57629=CARTESIAN_POINT('Ctrl Pts',(-50.,5.72601142143879,-14.4869849640075));
#57630=CARTESIAN_POINT('Ctrl Pts',(-66.,5.72469186277131,-14.611792753182));
#57631=CARTESIAN_POINT('Ctrl Pts',(-50.,5.72469186277131,-14.611792753182));
#57632=CARTESIAN_POINT('Ctrl Pts',(-66.,5.72295493404455,-14.7359981218931));
#57633=CARTESIAN_POINT('Ctrl Pts',(-50.,5.72295493404455,-14.7359981218931));
#57634=CARTESIAN_POINT('Ctrl Pts',(-66.,5.72276984468895,-14.8583414088431));
#57635=CARTESIAN_POINT('Ctrl Pts',(-50.,5.72276984468895,-14.8583414088431));
#57636=CARTESIAN_POINT('Ctrl Pts',(-66.,5.72472760042901,-14.9783796615786));
#57637=CARTESIAN_POINT('Ctrl Pts',(-50.,5.72472760042901,-14.9783796615786));
#57638=CARTESIAN_POINT('Ctrl Pts',(-66.,5.72682550780959,-15.0972765365679));
#57639=CARTESIAN_POINT('Ctrl Pts',(-50.,5.72682550780959,-15.0972765365679));
#57640=CARTESIAN_POINT('Ctrl Pts',(-66.,5.72404344314264,-15.2180917854697));
#57641=CARTESIAN_POINT('Ctrl Pts',(-50.,5.72404344314264,-15.2180917854697));
#57642=CARTESIAN_POINT('Ctrl Pts',(-66.,5.7111041198627,-15.3440703755711));
#57643=CARTESIAN_POINT('Ctrl Pts',(-50.,5.7111041198627,-15.3440703755711));
#57644=CARTESIAN_POINT('Ctrl Pts',(-66.,5.68483553281663,-15.4771820371687));
#57645=CARTESIAN_POINT('Ctrl Pts',(-50.,5.68483553281663,-15.4771820371687));
#57646=CARTESIAN_POINT('Ctrl Pts',(-66.,5.64658095828703,-15.616629779452));
#57647=CARTESIAN_POINT('Ctrl Pts',(-50.,5.64658095828703,-15.616629779452));
#57648=CARTESIAN_POINT('Ctrl Pts',(-66.,5.60492018787097,-15.7571674475031));
#57649=CARTESIAN_POINT('Ctrl Pts',(-50.,5.60492018787097,-15.7571674475031));
#57650=CARTESIAN_POINT('Ctrl Pts',(-66.,5.57357690598309,-15.8903852761089));
#57651=CARTESIAN_POINT('Ctrl Pts',(-50.,5.57357690598309,-15.8903852761089));
#57652=CARTESIAN_POINT('Ctrl Pts',(-66.,5.5687561428657,-16.0063469743079));
#57653=CARTESIAN_POINT('Ctrl Pts',(-50.,5.5687561428657,-16.0063469743079));
#57654=CARTESIAN_POINT('Ctrl Pts',(-66.,5.60688031869652,-16.0949814047159));
#57655=CARTESIAN_POINT('Ctrl Pts',(-50.,5.60688031869652,-16.0949814047159));
#57656=CARTESIAN_POINT('Ctrl Pts',(-66.,5.70173196024853,-16.1478393830386));
#57657=CARTESIAN_POINT('Ctrl Pts',(-50.,5.70173196024853,-16.1478393830386));
#57658=CARTESIAN_POINT('Ctrl Pts',(-66.,5.8636852794496,-16.1585658291036));
#57659=CARTESIAN_POINT('Ctrl Pts',(-50.,5.8636852794496,-16.1585658291036));
#57660=CARTESIAN_POINT('Ctrl Pts',(-66.,6.10047136055145,-16.1224288386879));
#57661=CARTESIAN_POINT('Ctrl Pts',(-50.,6.10047136055145,-16.1224288386879));
#57662=CARTESIAN_POINT('Ctrl Pts',(-66.,6.41747875111399,-16.0361345338456));
#57663=CARTESIAN_POINT('Ctrl Pts',(-50.,6.41747875111399,-16.0361345338456));
#57664=CARTESIAN_POINT('Ctrl Pts',(-66.,6.8182230142718,-15.8975380663557));
#57665=CARTESIAN_POINT('Ctrl Pts',(-50.,6.8182230142718,-15.8975380663557));
#57666=CARTESIAN_POINT('Ctrl Pts',(-66.,7.30472306816663,-15.705412002146));
#57667=CARTESIAN_POINT('Ctrl Pts',(-50.,7.30472306816663,-15.705412002146));
#57668=CARTESIAN_POINT('Ctrl Pts',(-66.,7.87789865673363,-15.4592017657445));
#57669=CARTESIAN_POINT('Ctrl Pts',(-50.,7.87789865673363,-15.4592017657445));
#57670=CARTESIAN_POINT('Ctrl Pts',(-66.,8.40593301690788,-15.2188781604602));
#57671=CARTESIAN_POINT('Ctrl Pts',(-50.,8.40593301690788,-15.2188781604602));
#57672=CARTESIAN_POINT('Ctrl Pts',(-66.,8.84097325982172,-15.0142967817227));
#57673=CARTESIAN_POINT('Ctrl Pts',(-50.,8.84097325982172,-15.0142967817227));
#57674=CARTESIAN_POINT('Ctrl Pts',(-66.,9.14831679120446,-14.8671063944355));
#57675=CARTESIAN_POINT('Ctrl Pts',(-50.,9.14831679120446,-14.8671063944355));
#57676=CARTESIAN_POINT('Ctrl Pts',(-66.,9.30631773451278,-14.7908104992354));
#57677=CARTESIAN_POINT('Ctrl Pts',(-50.,9.30631773451278,-14.7908104992354));
#57678=CARTESIAN_POINT('',(-65.5,5.57616560087513,-15.9270839199025));
#57679=CARTESIAN_POINT('Ctrl Pts',(-66.,5.70745604345954,-15.3481455072584));
#57680=CARTESIAN_POINT('Ctrl Pts',(-65.7933280154029,5.67157216480773,-15.5819887038945));
#57681=CARTESIAN_POINT('Ctrl Pts',(-65.6370761749494,5.58469409422519,-15.7788636458467));
#57682=CARTESIAN_POINT('Ctrl Pts',(-65.5,5.57616560087513,-15.9270839199025));
#57683=CARTESIAN_POINT('',(-66.,5.35024281477071,-13.004953213026));
#57684=CARTESIAN_POINT('',(-50.5,5.57616560087513,-15.9270839199025));
#57685=CARTESIAN_POINT('Ctrl Pts',(-50.5,5.57616560087513,-15.9270839199025));
#57686=CARTESIAN_POINT('Ctrl Pts',(-50.4518618349118,5.57916062186248,-15.8750321900921));
#57687=CARTESIAN_POINT('Ctrl Pts',(-50.4012423593877,5.59158821763518,-15.8170054325664));
#57688=CARTESIAN_POINT('Ctrl Pts',(-50.2441129793791,5.63902638944085,-15.6333426788586));
#57689=CARTESIAN_POINT('Ctrl Pts',(-50.1366827452935,5.68372420067752,-15.5027979636459));
#57690=CARTESIAN_POINT('Ctrl Pts',(-50.,5.70745604345953,-15.3481455072584));
#57691=CARTESIAN_POINT('Ctrl Pts',(-65.5,5.57616560087513,-15.9270839199025));
#57692=CARTESIAN_POINT('Ctrl Pts',(-60.5,5.57616560087513,-15.9270839199025));
#57693=CARTESIAN_POINT('Ctrl Pts',(-55.5,5.57616560087513,-15.9270839199025));
#57694=CARTESIAN_POINT('Ctrl Pts',(-50.5,5.57616560087513,-15.9270839199025));
#57695=CARTESIAN_POINT('Origin',(-66.,0.,0.));
#57696=CARTESIAN_POINT('',(-66.,6.61011555120063,-12.4121021043889));
#57697=CARTESIAN_POINT('Ctrl Pts',(-66.,9.30631773451278,-14.7908104992354));
#57698=CARTESIAN_POINT('Ctrl Pts',(-50.,9.30631773451278,-14.7908104992354));
#57699=CARTESIAN_POINT('Ctrl Pts',(-66.,9.28590458706215,-14.7813250267199));
#57700=CARTESIAN_POINT('Ctrl Pts',(-50.,9.28590458706215,-14.7813250267199));
#57701=CARTESIAN_POINT('Ctrl Pts',(-66.,9.24518215888137,-14.7622488452778));
#57702=CARTESIAN_POINT('Ctrl Pts',(-50.,9.24518215888137,-14.7622488452778));
#57703=CARTESIAN_POINT('Ctrl Pts',(-66.,9.18441011625632,-14.7333188643196));
#57704=CARTESIAN_POINT('Ctrl Pts',(-50.,9.18441011625632,-14.7333188643196));
#57705=CARTESIAN_POINT('Ctrl Pts',(-66.,9.10400475861348,-14.6941132952849));
#57706=CARTESIAN_POINT('Ctrl Pts',(-50.,9.10400475861348,-14.6941132952849));
#57707=CARTESIAN_POINT('Ctrl Pts',(-66.,9.00454259504917,-14.6440484693391));
#57708=CARTESIAN_POINT('Ctrl Pts',(-50.,9.00454259504917,-14.6440484693391));
#57709=CARTESIAN_POINT('Ctrl Pts',(-66.,8.90613010704717,-14.5929219106503));
#57710=CARTESIAN_POINT('Ctrl Pts',(-50.,8.90613010704717,-14.5929219106503));
#57711=CARTESIAN_POINT('Ctrl Pts',(-66.,8.80877107019522,-14.5407324590199));
#57712=CARTESIAN_POINT('Ctrl Pts',(-50.,8.80877107019522,-14.5407324590199));
#57713=CARTESIAN_POINT('Ctrl Pts',(-66.,8.71246624269817,-14.4874838508255));
#57714=CARTESIAN_POINT('Ctrl Pts',(-50.,8.71246624269817,-14.4874838508255));
#57715=CARTESIAN_POINT('Ctrl Pts',(-66.,8.61721041044846,-14.433188014658));
#57716=CARTESIAN_POINT('Ctrl Pts',(-50.,8.61721041044846,-14.433188014658));
#57717=CARTESIAN_POINT('Ctrl Pts',(-66.,8.52300011506032,-14.3778594394275));
#57718=CARTESIAN_POINT('Ctrl Pts',(-50.,8.52300011506032,-14.3778594394275));
#57719=CARTESIAN_POINT('Ctrl Pts',(-66.,8.42984251254175,-14.3215085444515));
#57720=CARTESIAN_POINT('Ctrl Pts',(-50.,8.42984251254175,-14.3215085444515));
#57721=CARTESIAN_POINT('Ctrl Pts',(-66.,8.33776450465061,-14.2641350302423));
#57722=CARTESIAN_POINT('Ctrl Pts',(-50.,8.33776450465061,-14.2641350302423));
#57723=CARTESIAN_POINT('Ctrl Pts',(-66.,8.24682004139236,-14.2057223854076));
#57724=CARTESIAN_POINT('Ctrl Pts',(-50.,8.24682004139236,-14.2057223854076));
#57725=CARTESIAN_POINT('Ctrl Pts',(-66.,8.15710255651542,-14.1462291692713));
#57726=CARTESIAN_POINT('Ctrl Pts',(-50.,8.15710255651542,-14.1462291692713));
#57727=CARTESIAN_POINT('Ctrl Pts',(-66.,8.06872580598559,-14.0856005156321));
#57728=CARTESIAN_POINT('Ctrl Pts',(-50.,8.06872580598559,-14.0856005156321));
#57729=CARTESIAN_POINT('Ctrl Pts',(-66.,7.98179694893469,-14.0237846738158));
#57730=CARTESIAN_POINT('Ctrl Pts',(-50.,7.98179694893469,-14.0237846738158));
#57731=CARTESIAN_POINT('Ctrl Pts',(-66.,7.89638987124254,-13.9607493051802));
#57732=CARTESIAN_POINT('Ctrl Pts',(-50.,7.89638987124254,-13.9607493051802));
#57733=CARTESIAN_POINT('Ctrl Pts',(-66.,7.81252309986449,-13.8964951055849));
#57734=CARTESIAN_POINT('Ctrl Pts',(-50.,7.81252309986449,-13.8964951055849));
#57735=CARTESIAN_POINT('Ctrl Pts',(-66.,7.7301225433348,-13.8310785215643));
#57736=CARTESIAN_POINT('Ctrl Pts',(-50.,7.7301225433348,-13.8310785215643));
#57737=CARTESIAN_POINT('Ctrl Pts',(-66.,7.6490662730339,-13.7645853488249));
#57738=CARTESIAN_POINT('Ctrl Pts',(-50.,7.6490662730339,-13.7645853488249));
#57739=CARTESIAN_POINT('Ctrl Pts',(-66.,7.56925639420599,-13.6970881198352));
#57740=CARTESIAN_POINT('Ctrl Pts',(-50.,7.56925639420599,-13.6970881198352));
#57741=CARTESIAN_POINT('Ctrl Pts',(-66.,7.49068629797234,-13.6286062937474));
#57742=CARTESIAN_POINT('Ctrl Pts',(-50.,7.49068629797234,-13.6286062937474));
#57743=CARTESIAN_POINT('Ctrl Pts',(-66.,7.41350024004436,-13.5590710567155));
#57744=CARTESIAN_POINT('Ctrl Pts',(-50.,7.41350024004436,-13.5590710567155));
#57745=CARTESIAN_POINT('Ctrl Pts',(-66.,7.33808196640605,-13.4882727841331));
#57746=CARTESIAN_POINT('Ctrl Pts',(-50.,7.33808196640605,-13.4882727841331));
#57747=CARTESIAN_POINT('Ctrl Pts',(-66.,7.26497865575545,-13.4159069786186));
#57748=CARTESIAN_POINT('Ctrl Pts',(-50.,7.26497865575545,-13.4159069786186));
#57749=CARTESIAN_POINT('Ctrl Pts',(-66.,7.19476912913493,-13.3416535097654));
#57750=CARTESIAN_POINT('Ctrl Pts',(-50.,7.19476912913493,-13.3416535097654));
#57751=CARTESIAN_POINT('Ctrl Pts',(-66.,7.12794583824513,-13.2652477369413));
#57752=CARTESIAN_POINT('Ctrl Pts',(-50.,7.12794583824513,-13.2652477369413));
#57753=CARTESIAN_POINT('Ctrl Pts',(-66.,7.06480099833745,-13.1865489711723));
#57754=CARTESIAN_POINT('Ctrl Pts',(-50.,7.06480099833745,-13.1865489711723));
#57755=CARTESIAN_POINT('Ctrl Pts',(-66.,7.00528244199424,-13.1056276044837));
#57756=CARTESIAN_POINT('Ctrl Pts',(-50.,7.00528244199424,-13.1056276044837));
#57757=CARTESIAN_POINT('Ctrl Pts',(-66.,6.94905904389849,-13.0227234927017));
#57758=CARTESIAN_POINT('Ctrl Pts',(-50.,6.94905904389849,-13.0227234927017));
#57759=CARTESIAN_POINT('Ctrl Pts',(-66.,6.89563993078743,-12.9381713275312));
#57760=CARTESIAN_POINT('Ctrl Pts',(-50.,6.89563993078743,-12.9381713275312));
#57761=CARTESIAN_POINT('Ctrl Pts',(-66.,6.84447568757558,-12.8523369979956));
#57762=CARTESIAN_POINT('Ctrl Pts',(-50.,6.84447568757558,-12.8523369979956));
#57763=CARTESIAN_POINT('Ctrl Pts',(-66.,6.79506247552229,-12.7655522513249));
#57764=CARTESIAN_POINT('Ctrl Pts',(-50.,6.79506247552229,-12.7655522513249));
#57765=CARTESIAN_POINT('Ctrl Pts',(-66.,6.74705476751256,-12.6780437370314));
#57766=CARTESIAN_POINT('Ctrl Pts',(-50.,6.74705476751256,-12.6780437370314));
#57767=CARTESIAN_POINT('Ctrl Pts',(-66.,6.70024437485702,-12.5899474002701));
#57768=CARTESIAN_POINT('Ctrl Pts',(-50.,6.70024437485702,-12.5899474002701));
#57769=CARTESIAN_POINT('Ctrl Pts',(-66.,6.66366757586302,-12.5190559665502));
#57770=CARTESIAN_POINT('Ctrl Pts',(-50.,6.66366757586302,-12.5190559665502));
#57771=CARTESIAN_POINT('Ctrl Pts',(-66.,6.63670790506457,-12.4656652861453));
#57772=CARTESIAN_POINT('Ctrl Pts',(-50.,6.63670790506457,-12.4656652861453));
#57773=CARTESIAN_POINT('Ctrl Pts',(-66.,6.6189446860433,-12.4299729273552));
#57774=CARTESIAN_POINT('Ctrl Pts',(-50.,6.6189446860433,-12.4299729273552));
#57775=CARTESIAN_POINT('Ctrl Pts',(-66.,6.61011555120064,-12.4121021043889));
#57776=CARTESIAN_POINT('Ctrl Pts',(-50.,6.61011555120064,-12.4121021043889));
#57777=CARTESIAN_POINT('Origin',(-65.75,0.,0.));
#57778=CARTESIAN_POINT('',(-65.5,4.81099111997379,-16.1746712313893));
#57779=CARTESIAN_POINT('Origin',(-65.5,0.,0.));
#57780=CARTESIAN_POINT('Ctrl Pts',(-65.5,4.81099111997379,-16.1746712313893));
#57781=CARTESIAN_POINT('Ctrl Pts',(-65.6931595476677,4.65121959653276,-16.0206706986577));
#57782=CARTESIAN_POINT('Ctrl Pts',(-65.8611256967025,4.52077235532675,-15.8831797802523));
#57783=CARTESIAN_POINT('Ctrl Pts',(-66.,4.41702961547072,-15.7680206232759));
#57784=CARTESIAN_POINT('Origin',(-58.,0.,0.));
#57785=CARTESIAN_POINT('',(-50.5,4.81099111997379,-16.1746712313893));
#57786=CARTESIAN_POINT('Origin',(-50.5,0.,0.));
#57787=CARTESIAN_POINT('Ctrl Pts',(-50.5,4.81099111997379,-16.1746712313893));
#57788=CARTESIAN_POINT('Ctrl Pts',(-55.5,4.81099111997379,-16.1746712313893));
#57789=CARTESIAN_POINT('Ctrl Pts',(-60.5,4.81099111997379,-16.1746712313893));
#57790=CARTESIAN_POINT('Ctrl Pts',(-65.5,4.81099111997379,-16.1746712313893));
#57791=CARTESIAN_POINT('Origin',(-50.25,0.,0.));
#57792=CARTESIAN_POINT('Ctrl Pts',(-50.,4.41702961547073,-15.7680206232759));
#57793=CARTESIAN_POINT('Ctrl Pts',(-50.1388743032811,4.52077235531448,-15.8831797802387));
#57794=CARTESIAN_POINT('Ctrl Pts',(-50.3068404523174,4.65121959652049,-16.0206706986458));
#57795=CARTESIAN_POINT('Ctrl Pts',(-50.5,4.81099111997378,-16.1746712313893));
#57796=CARTESIAN_POINT('Ctrl Pts',(-66.,1.94795475120472,-13.9269299753125));
#57797=CARTESIAN_POINT('Ctrl Pts',(-50.,1.94795475120472,-13.9269299753125));
#57798=CARTESIAN_POINT('Ctrl Pts',(-66.,1.95214068696407,-13.9499241564345));
#57799=CARTESIAN_POINT('Ctrl Pts',(-50.,1.95214068696407,-13.9499241564345));
#57800=CARTESIAN_POINT('Ctrl Pts',(-66.,1.96029291597316,-13.9959617603545));
#57801=CARTESIAN_POINT('Ctrl Pts',(-50.,1.96029291597316,-13.9959617603545));
#57802=CARTESIAN_POINT('Ctrl Pts',(-66.,1.9718623445077,-14.0651658958429));
#57803=CARTESIAN_POINT('Ctrl Pts',(-50.,1.9718623445077,-14.0651658958429));
#57804=CARTESIAN_POINT('Ctrl Pts',(-66.,1.98596855852791,-14.1577338890203));
#57805=CARTESIAN_POINT('Ctrl Pts',(-50.,1.98596855852791,-14.1577338890203));
#57806=CARTESIAN_POINT('Ctrl Pts',(-66.,2.00134518601523,-14.2739302306637));
#57807=CARTESIAN_POINT('Ctrl Pts',(-50.,2.00134518601523,-14.2739302306637));
#57808=CARTESIAN_POINT('Ctrl Pts',(-66.,2.01431120793567,-14.3905881617116));
#57809=CARTESIAN_POINT('Ctrl Pts',(-50.,2.01431120793567,-14.3905881617116));
#57810=CARTESIAN_POINT('Ctrl Pts',(-66.,2.02457419816135,-14.5076563645426));
#57811=CARTESIAN_POINT('Ctrl Pts',(-50.,2.02457419816135,-14.5076563645426));
#57812=CARTESIAN_POINT('Ctrl Pts',(-66.,2.03164894817481,-14.625042880531));
#57813=CARTESIAN_POINT('Ctrl Pts',(-50.,2.03164894817481,-14.625042880531));
#57814=CARTESIAN_POINT('Ctrl Pts',(-66.,2.03491450329845,-14.7426508740692));
#57815=CARTESIAN_POINT('Ctrl Pts',(-50.,2.03491450329845,-14.7426508740692));
#57816=CARTESIAN_POINT('Ctrl Pts',(-66.,2.03368724587156,-14.8604288747958));
#57817=CARTESIAN_POINT('Ctrl Pts',(-50.,2.03368724587156,-14.8604288747958));
#57818=CARTESIAN_POINT('Ctrl Pts',(-66.,2.02729586462329,-14.9784060380191));
#57819=CARTESIAN_POINT('Ctrl Pts',(-50.,2.02729586462329,-14.9784060380191));
#57820=CARTESIAN_POINT('Ctrl Pts',(-66.,2.01513711377743,-15.096758960368));
#57821=CARTESIAN_POINT('Ctrl Pts',(-50.,2.01513711377743,-15.096758960368));
#57822=CARTESIAN_POINT('Ctrl Pts',(-66.,1.99685540944097,-15.2157295916163));
#57823=CARTESIAN_POINT('Ctrl Pts',(-50.,1.99685540944097,-15.2157295916163));
#57824=CARTESIAN_POINT('Ctrl Pts',(-66.,1.97262912616775,-15.3354545564815));
#57825=CARTESIAN_POINT('Ctrl Pts',(-50.,1.97262912616775,-15.3354545564815));
#57826=CARTESIAN_POINT('Ctrl Pts',(-66.,1.94335158717786,-15.4558508259636));
#57827=CARTESIAN_POINT('Ctrl Pts',(-50.,1.94335158717786,-15.4558508259636));
#57828=CARTESIAN_POINT('Ctrl Pts',(-66.,1.91103504986532,-15.5764093880396));
#57829=CARTESIAN_POINT('Ctrl Pts',(-50.,1.91103504986532,-15.5764093880396));
#57830=CARTESIAN_POINT('Ctrl Pts',(-66.,1.87846407081847,-15.6962806600859));
#57831=CARTESIAN_POINT('Ctrl Pts',(-50.,1.87846407081847,-15.6962806600859));
#57832=CARTESIAN_POINT('Ctrl Pts',(-66.,1.84785925815835,-15.8147342778518));
#57833=CARTESIAN_POINT('Ctrl Pts',(-50.,1.84785925815835,-15.8147342778518));
#57834=CARTESIAN_POINT('Ctrl Pts',(-66.,1.81990320787353,-15.9314881821968));
#57835=CARTESIAN_POINT('Ctrl Pts',(-50.,1.81990320787353,-15.9314881821968));
#57836=CARTESIAN_POINT('Ctrl Pts',(-66.,1.79236675521062,-16.047171421572));
#57837=CARTESIAN_POINT('Ctrl Pts',(-50.,1.79236675521062,-16.047171421572));
#57838=CARTESIAN_POINT('Ctrl Pts',(-66.,1.75962656360386,-16.1634991659178));
#57839=CARTESIAN_POINT('Ctrl Pts',(-50.,1.75962656360386,-16.1634991659178));
#57840=CARTESIAN_POINT('Ctrl Pts',(-66.,1.71576415160101,-16.2823020281062));
#57841=CARTESIAN_POINT('Ctrl Pts',(-50.,1.71576415160101,-16.2823020281062));
#57842=CARTESIAN_POINT('Ctrl Pts',(-66.,1.65721731641851,-16.404699010131));
#57843=CARTESIAN_POINT('Ctrl Pts',(-50.,1.65721731641851,-16.404699010131));
#57844=CARTESIAN_POINT('Ctrl Pts',(-66.,1.58548533639917,-16.5302522193407));
#57845=CARTESIAN_POINT('Ctrl Pts',(-50.,1.58548533639917,-16.5302522193407));
#57846=CARTESIAN_POINT('Ctrl Pts',(-66.,1.51018311888448,-16.6560140258254));
#57847=CARTESIAN_POINT('Ctrl Pts',(-50.,1.51018311888448,-16.6560140258254));
#57848=CARTESIAN_POINT('Ctrl Pts',(-66.,1.44669461706905,-16.777251814139));
#57849=CARTESIAN_POINT('Ctrl Pts',(-50.,1.44669461706905,-16.777251814139));
#57850=CARTESIAN_POINT('Ctrl Pts',(-66.,1.4131868054492,-16.8883714873147));
#57851=CARTESIAN_POINT('Ctrl Pts',(-50.,1.4131868054492,-16.8883714873147));
#57852=CARTESIAN_POINT('Ctrl Pts',(-66.,1.42807075369374,-16.9837024010898));
#57853=CARTESIAN_POINT('Ctrl Pts',(-50.,1.42807075369374,-16.9837024010898));
#57854=CARTESIAN_POINT('Ctrl Pts',(-66.,1.5067972118416,-17.0584883928594));
#57855=CARTESIAN_POINT('Ctrl Pts',(-50.,1.5067972118416,-17.0584883928594));
#57856=CARTESIAN_POINT('Ctrl Pts',(-66.,1.66099491104707,-17.1091540005748));
#57857=CARTESIAN_POINT('Ctrl Pts',(-50.,1.66099491104707,-17.1091540005748));
#57858=CARTESIAN_POINT('Ctrl Pts',(-66.,1.89932882606092,-17.1330386239557));
#57859=CARTESIAN_POINT('Ctrl Pts',(-50.,1.89932882606092,-17.1330386239557));
#57860=CARTESIAN_POINT('Ctrl Pts',(-66.,2.22783736744731,-17.1282919455736));
#57861=CARTESIAN_POINT('Ctrl Pts',(-50.,2.22783736744731,-17.1282919455736));
#57862=CARTESIAN_POINT('Ctrl Pts',(-66.,2.65045905252241,-17.0937107865576));
#57863=CARTESIAN_POINT('Ctrl Pts',(-50.,2.65045905252241,-17.0937107865576));
#57864=CARTESIAN_POINT('Ctrl Pts',(-66.,3.16945462184284,-17.028608359459));
#57865=CARTESIAN_POINT('Ctrl Pts',(-50.,3.16945462184284,-17.028608359459));
#57866=CARTESIAN_POINT('Ctrl Pts',(-66.,3.78585284120834,-16.9326762428294));
#57867=CARTESIAN_POINT('Ctrl Pts',(-50.,3.78585284120834,-16.9326762428294));
#57868=CARTESIAN_POINT('Ctrl Pts',(-66.,4.35706408125165,-16.8312196509802));
#57869=CARTESIAN_POINT('Ctrl Pts',(-50.,4.35706408125165,-16.8312196509802));
#57870=CARTESIAN_POINT('Ctrl Pts',(-66.,4.82931405494557,-16.741255681377));
#57871=CARTESIAN_POINT('Ctrl Pts',(-50.,4.82931405494557,-16.741255681377));
#57872=CARTESIAN_POINT('Ctrl Pts',(-66.,5.1636065849309,-16.675122778911));
#57873=CARTESIAN_POINT('Ctrl Pts',(-50.,5.1636065849309,-16.675122778911));
#57874=CARTESIAN_POINT('Ctrl Pts',(-66.,5.33561765563024,-16.6405170963203));
#57875=CARTESIAN_POINT('Ctrl Pts',(-50.,5.33561765563024,-16.6405170963203));
#57876=CARTESIAN_POINT('',(-65.5,1.44007540176665,-16.8134412847943));
#57877=CARTESIAN_POINT('Ctrl Pts',(-66.,1.71121724218688,-16.2853418923289));
#57878=CARTESIAN_POINT('Ctrl Pts',(-65.793328015403,1.61830628338315,-16.5029145172019));
#57879=CARTESIAN_POINT('Ctrl Pts',(-65.6370761749494,1.48519684004577,-16.671998573255));
#57880=CARTESIAN_POINT('Ctrl Pts',(-65.5,1.44007540176665,-16.8134412847943));
#57881=CARTESIAN_POINT('',(-66.,1.94795475120472,-13.9269299753125));
#57882=CARTESIAN_POINT('',(-50.5,1.44007540176665,-16.8134412847943));
#57883=CARTESIAN_POINT('Ctrl Pts',(-50.5,1.44007540176665,-16.8134412847943));
#57884=CARTESIAN_POINT('Ctrl Pts',(-50.4518618349121,1.45592106747543,-16.763769687224));
#57885=CARTESIAN_POINT('Ctrl Pts',(-50.4012423593882,1.48238889525558,-16.7106565643805));
#57886=CARTESIAN_POINT('Ctrl Pts',(-50.2441129793797,1.57401177915707,-16.5445613074064));
#57887=CARTESIAN_POINT('Ctrl Pts',(-50.1366827452939,1.64977047695671,-16.4292337881098));
#57888=CARTESIAN_POINT('Ctrl Pts',(-50.,1.71121724218688,-16.2853418923289));
#57889=CARTESIAN_POINT('Ctrl Pts',(-65.5,1.44007540176665,-16.8134412847943));
#57890=CARTESIAN_POINT('Ctrl Pts',(-60.5,1.44007540176665,-16.8134412847943));
#57891=CARTESIAN_POINT('Ctrl Pts',(-55.5,1.44007540176665,-16.8134412847943));
#57892=CARTESIAN_POINT('Ctrl Pts',(-50.5,1.44007540176665,-16.8134412847943));
#57893=CARTESIAN_POINT('Origin',(-66.,0.,0.));
#57894=CARTESIAN_POINT('',(-66.,3.31568234418831,-13.6660219830951));
#57895=CARTESIAN_POINT('Ctrl Pts',(-66.,5.33561765563024,-16.6405170963203));
#57896=CARTESIAN_POINT('Ctrl Pts',(-50.,5.33561765563024,-16.6405170963203));
#57897=CARTESIAN_POINT('Ctrl Pts',(-66.,5.3182047658335,-16.6262530840302));
#57898=CARTESIAN_POINT('Ctrl Pts',(-50.,5.3182047658335,-16.6262530840302));
#57899=CARTESIAN_POINT('Ctrl Pts',(-66.,5.28350576102771,-16.5976489598374));
#57900=CARTESIAN_POINT('Ctrl Pts',(-50.,5.28350576102771,-16.5976489598374));
#57901=CARTESIAN_POINT('Ctrl Pts',(-66.,5.23183757757387,-16.5545144750063));
#57902=CARTESIAN_POINT('Ctrl Pts',(-50.,5.23183757757387,-16.5545144750063));
#57903=CARTESIAN_POINT('Ctrl Pts',(-66.,5.16370833063597,-16.4965446216971));
#57904=CARTESIAN_POINT('Ctrl Pts',(-50.,5.16370833063597,-16.4965446216971));
#57905=CARTESIAN_POINT('Ctrl Pts',(-66.,5.07982156975354,-16.4233174400873));
#57906=CARTESIAN_POINT('Ctrl Pts',(-50.,5.07982156975354,-16.4233174400873));
#57907=CARTESIAN_POINT('Ctrl Pts',(-66.,4.99721554914146,-16.349322925718));
#57908=CARTESIAN_POINT('Ctrl Pts',(-50.,4.99721554914146,-16.349322925718));
#57909=CARTESIAN_POINT('Ctrl Pts',(-66.,4.91589421430013,-16.2745608937911));
#57910=CARTESIAN_POINT('Ctrl Pts',(-50.,4.91589421430013,-16.2745608937911));
#57911=CARTESIAN_POINT('Ctrl Pts',(-66.,4.83585737041464,-16.1990351518568));
#57912=CARTESIAN_POINT('Ctrl Pts',(-50.,4.83585737041464,-16.1990351518568));
#57913=CARTESIAN_POINT('Ctrl Pts',(-66.,4.7570970006683,-16.1227559570515));
#57914=CARTESIAN_POINT('Ctrl Pts',(-50.,4.7570970006683,-16.1227559570515));
#57915=CARTESIAN_POINT('Ctrl Pts',(-66.,4.67960615208147,-16.0457364830242));
#57916=CARTESIAN_POINT('Ctrl Pts',(-50.,4.67960615208147,-16.0457364830242));
#57917=CARTESIAN_POINT('Ctrl Pts',(-66.,4.60338916466408,-15.967988601377));
#57918=CARTESIAN_POINT('Ctrl Pts',(-50.,4.60338916466408,-15.967988601377));
#57919=CARTESIAN_POINT('Ctrl Pts',(-66.,4.52847216948537,-15.8895187122264));
#57920=CARTESIAN_POINT('Ctrl Pts',(-50.,4.52847216948537,-15.8895187122264));
#57921=CARTESIAN_POINT('Ctrl Pts',(-66.,4.45491152782849,-15.8103242397366));
#57922=CARTESIAN_POINT('Ctrl Pts',(-50.,4.45491152782849,-15.8103242397366));
#57923=CARTESIAN_POINT('Ctrl Pts',(-66.,4.38280804392589,-15.7303882811948));
#57924=CARTESIAN_POINT('Ctrl Pts',(-50.,4.38280804392589,-15.7303882811948));
#57925=CARTESIAN_POINT('Ctrl Pts',(-66.,4.31228554455994,-15.6496859840807));
#57926=CARTESIAN_POINT('Ctrl Pts',(-50.,4.31228554455994,-15.6496859840807));
#57927=CARTESIAN_POINT('Ctrl Pts',(-66.,4.24346069213056,-15.5681938729551));
#57928=CARTESIAN_POINT('Ctrl Pts',(-50.,4.24346069213056,-15.5681938729551));
#57929=CARTESIAN_POINT('Ctrl Pts',(-66.,4.17641309355012,-15.4858989998248));
#57930=CARTESIAN_POINT('Ctrl Pts',(-50.,4.17641309355012,-15.4858989998248));
#57931=CARTESIAN_POINT('Ctrl Pts',(-66.,4.11116052066234,-15.4028066461541));
#57932=CARTESIAN_POINT('Ctrl Pts',(-50.,4.11116052066234,-15.4028066461541));
#57933=CARTESIAN_POINT('Ctrl Pts',(-66.,4.04761717203886,-15.3189530593075));
#57934=CARTESIAN_POINT('Ctrl Pts',(-50.,4.04761717203886,-15.3189530593075));
#57935=CARTESIAN_POINT('Ctrl Pts',(-66.,3.98564361314731,-15.2343910171469));
#57936=CARTESIAN_POINT('Ctrl Pts',(-50.,3.98564361314731,-15.2343910171469));
#57937=CARTESIAN_POINT('Ctrl Pts',(-66.,3.92512698668427,-15.1491664279643));
#57938=CARTESIAN_POINT('Ctrl Pts',(-50.,3.92512698668427,-15.1491664279643));
#57939=CARTESIAN_POINT('Ctrl Pts',(-66.,3.8660560521067,-15.0632964960055));
#57940=CARTESIAN_POINT('Ctrl Pts',(-50.,3.8660560521067,-15.0632964960055));
#57941=CARTESIAN_POINT('Ctrl Pts',(-66.,3.80858764637521,-14.9767504442745));
#57942=CARTESIAN_POINT('Ctrl Pts',(-50.,3.80858764637521,-14.9767504442745));
#57943=CARTESIAN_POINT('Ctrl Pts',(-66.,3.75314559090774,-14.8894206676529));
#57944=CARTESIAN_POINT('Ctrl Pts',(-50.,3.75314559090774,-14.8894206676529));
#57945=CARTESIAN_POINT('Ctrl Pts',(-66.,3.7003355991968,-14.801148312913));
#57946=CARTESIAN_POINT('Ctrl Pts',(-50.,3.7003355991968,-14.801148312913));
#57947=CARTESIAN_POINT('Ctrl Pts',(-66.,3.65079792075207,-14.7117672540732));
#57948=CARTESIAN_POINT('Ctrl Pts',(-50.,3.65079792075207,-14.7117672540732));
#57949=CARTESIAN_POINT('Ctrl Pts',(-66.,3.60507534944737,-14.6211436324314));
#57950=CARTESIAN_POINT('Ctrl Pts',(-50.,3.60507534944737,-14.6211436324314));
#57951=CARTESIAN_POINT('Ctrl Pts',(-66.,3.56348590797974,-14.5292138499942));
#57952=CARTESIAN_POINT('Ctrl Pts',(-50.,3.56348590797974,-14.5292138499942));
#57953=CARTESIAN_POINT('Ctrl Pts',(-66.,3.52596156208203,-14.436033113783));
#57954=CARTESIAN_POINT('Ctrl Pts',(-50.,3.52596156208203,-14.436033113783));
#57955=CARTESIAN_POINT('Ctrl Pts',(-66.,3.49212193962963,-14.3417513965941));
#57956=CARTESIAN_POINT('Ctrl Pts',(-50.,3.49212193962963,-14.3417513965941));
#57957=CARTESIAN_POINT('Ctrl Pts',(-66.,3.46140835460361,-14.246570799961));
#57958=CARTESIAN_POINT('Ctrl Pts',(-50.,3.46140835460361,-14.246570799961));
#57959=CARTESIAN_POINT('Ctrl Pts',(-66.,3.43319765990381,-14.1507090838548));
#57960=CARTESIAN_POINT('Ctrl Pts',(-50.,3.43319765990381,-14.1507090838548));
#57961=CARTESIAN_POINT('Ctrl Pts',(-66.,3.40691934362888,-14.0543622734568));
#57962=CARTESIAN_POINT('Ctrl Pts',(-50.,3.40691934362888,-14.0543622734568));
#57963=CARTESIAN_POINT('Ctrl Pts',(-66.,3.38218236859189,-13.9576639685687));
#57964=CARTESIAN_POINT('Ctrl Pts',(-50.,3.38218236859189,-13.9576639685687));
#57965=CARTESIAN_POINT('Ctrl Pts',(-66.,3.35875127854871,-13.860694068957));
#57966=CARTESIAN_POINT('Ctrl Pts',(-50.,3.35875127854871,-13.860694068957));
#57967=CARTESIAN_POINT('Ctrl Pts',(-66.,3.34095358960791,-13.7829335399729));
#57968=CARTESIAN_POINT('Ctrl Pts',(-50.,3.34095358960791,-13.7829335399729));
#57969=CARTESIAN_POINT('Ctrl Pts',(-66.,3.3281186287285,-13.7245156284827));
#57970=CARTESIAN_POINT('Ctrl Pts',(-50.,3.3281186287285,-13.7245156284827));
#57971=CARTESIAN_POINT('Ctrl Pts',(-66.,3.31978980257722,-13.6855270778435));
#57972=CARTESIAN_POINT('Ctrl Pts',(-50.,3.31978980257722,-13.6855270778435));
#57973=CARTESIAN_POINT('Ctrl Pts',(-66.,3.31568234418832,-13.6660219830951));
#57974=CARTESIAN_POINT('Ctrl Pts',(-50.,3.31568234418832,-13.6660219830951));
#57975=CARTESIAN_POINT('Origin',(-65.75,0.,0.));
#57976=CARTESIAN_POINT('',(-65.5,0.637367823683143,-16.8629590302928));
#57977=CARTESIAN_POINT('Origin',(-65.5,0.,0.));
#57978=CARTESIAN_POINT('Ctrl Pts',(-65.5,0.637367823683148,-16.8629590302928));
#57979=CARTESIAN_POINT('Ctrl Pts',(-65.5824396971602,0.587667004731077,
-16.7823408476978));
#57980=CARTESIAN_POINT('Ctrl Pts',(-65.6660036204853,0.539005134923334,
-16.7003659612199));
#57981=CARTESIAN_POINT('Ctrl Pts',(-65.7496756578578,0.492037124098817,
-16.6180469545161));
#57982=CARTESIAN_POINT('Ctrl Pts',(-65.8190041635689,0.45312063408684,-16.5498395353398));
#57983=CARTESIAN_POINT('Ctrl Pts',(-65.8884068934103,0.415362256265888,
-16.4813977166555));
#57984=CARTESIAN_POINT('Ctrl Pts',(-65.9573058363633,0.379170886061448,
-16.4133154040527));
#57985=CARTESIAN_POINT('Ctrl Pts',(-65.9715604948122,0.371683171461654,
-16.3992297001077));
#57986=CARTESIAN_POINT('Ctrl Pts',(-65.9857935889606,0.364262713372718,
-16.385159414606));
#57987=CARTESIAN_POINT('Ctrl Pts',(-66.,0.35691323813583,-16.3711098567093));
#57988=CARTESIAN_POINT('Origin',(-58.,0.,0.));
#57989=CARTESIAN_POINT('',(-50.5,0.637367823683145,-16.8629590302928));
#57990=CARTESIAN_POINT('Origin',(-50.5,0.,0.));
#57991=CARTESIAN_POINT('Ctrl Pts',(-50.5,0.637367823683145,-16.8629590302928));
#57992=CARTESIAN_POINT('Ctrl Pts',(-55.5,0.637367823683145,-16.8629590302928));
#57993=CARTESIAN_POINT('Ctrl Pts',(-60.5,0.637367823683144,-16.8629590302928));
#57994=CARTESIAN_POINT('Ctrl Pts',(-65.5,0.637367823683144,-16.8629590302928));
#57995=CARTESIAN_POINT('Origin',(-50.25,0.,0.));
#57996=CARTESIAN_POINT('Ctrl Pts',(-50.,0.356913238135828,-16.3711098567093));
#57997=CARTESIAN_POINT('Ctrl Pts',(-50.0728233300466,0.394587303694001,
-16.4431291435567));
#57998=CARTESIAN_POINT('Ctrl Pts',(-50.1463478065558,0.434124407382829,
-16.5156921628394));
#57999=CARTESIAN_POINT('Ctrl Pts',(-50.2198839404944,0.47502746617852,-16.5880885420746));
#58000=CARTESIAN_POINT('Ctrl Pts',(-50.3051443233005,0.52245191269314,-16.6720274531483));
#58001=CARTESIAN_POINT('Ctrl Pts',(-50.3904203770725,0.571717341873418,
-16.7557397783304));
#58002=CARTESIAN_POINT('Ctrl Pts',(-50.4746374523709,0.622131372875589,
-16.8381489075303));
#58003=CARTESIAN_POINT('Ctrl Pts',(-50.4831026982763,0.627198838921015,
-16.8464324241576));
#58004=CARTESIAN_POINT('Ctrl Pts',(-50.4915572446203,0.632277898913462,
-16.8547028185617));
#58005=CARTESIAN_POINT('Ctrl Pts',(-50.5,0.637367823683148,-16.8629590302928));
#58006=CARTESIAN_POINT('Ctrl Pts',(-66.,-1.57673047345591,-13.9738265075847));
#58007=CARTESIAN_POINT('Ctrl Pts',(-50.,-1.57673047345591,-13.9738265075847));
#58008=CARTESIAN_POINT('Ctrl Pts',(-66.,-1.57839446687451,-13.997139284115));
#58009=CARTESIAN_POINT('Ctrl Pts',(-50.,-1.57839446687451,-13.997139284115));
#58010=CARTESIAN_POINT('Ctrl Pts',(-66.,-1.58194744165485,-14.0437579089631));
#58011=CARTESIAN_POINT('Ctrl Pts',(-50.,-1.58194744165485,-14.0437579089631));
#58012=CARTESIAN_POINT('Ctrl Pts',(-66.,-1.58795185663835,-14.1136650691543));
#58013=CARTESIAN_POINT('Ctrl Pts',(-50.,-1.58795185663835,-14.1136650691543));
#58014=CARTESIAN_POINT('Ctrl Pts',(-66.,-1.59730953904946,-14.2068329413785));
#58015=CARTESIAN_POINT('Ctrl Pts',(-50.,-1.59730953904946,-14.2068329413785));
#58016=CARTESIAN_POINT('Ctrl Pts',(-66.,-1.61131285168258,-14.3232027730338));
#58017=CARTESIAN_POINT('Ctrl Pts',(-50.,-1.61131285168258,-14.3232027730338));
#58018=CARTESIAN_POINT('Ctrl Pts',(-66.,-1.6277658288928,-14.4394201991873));
#58019=CARTESIAN_POINT('Ctrl Pts',(-50.,-1.6277658288928,-14.4394201991873));
#58020=CARTESIAN_POINT('Ctrl Pts',(-66.,-1.64693894753001,-14.5553627910342));
#58021=CARTESIAN_POINT('Ctrl Pts',(-50.,-1.64693894753001,-14.5553627910342));
#58022=CARTESIAN_POINT('Ctrl Pts',(-66.,-1.6692793032136,-14.6708208125467));
#58023=CARTESIAN_POINT('Ctrl Pts',(-50.,-1.6692793032136,-14.6708208125467));
#58024=CARTESIAN_POINT('Ctrl Pts',(-66.,-1.69536426015181,-14.7855460452371));
#58025=CARTESIAN_POINT('Ctrl Pts',(-50.,-1.69536426015181,-14.7855460452371));
#58026=CARTESIAN_POINT('Ctrl Pts',(-66.,-1.72584315874106,-14.8993186269813));
#58027=CARTESIAN_POINT('Ctrl Pts',(-50.,-1.72584315874106,-14.8993186269813));
#58028=CARTESIAN_POINT('Ctrl Pts',(-66.,-1.76137347040452,-15.0119998487957));
#58029=CARTESIAN_POINT('Ctrl Pts',(-50.,-1.76137347040452,-15.0119998487957));
#58030=CARTESIAN_POINT('Ctrl Pts',(-66.,-1.80258340663877,-15.1236107380773));
#58031=CARTESIAN_POINT('Ctrl Pts',(-50.,-1.80258340663877,-15.1236107380773));
#58032=CARTESIAN_POINT('Ctrl Pts',(-66.,-1.84987755047685,-15.2342972131845));
#58033=CARTESIAN_POINT('Ctrl Pts',(-50.,-1.84987755047685,-15.2342972131845));
#58034=CARTESIAN_POINT('Ctrl Pts',(-66.,-1.90311710851519,-15.3442359664661));
#58035=CARTESIAN_POINT('Ctrl Pts',(-50.,-1.90311710851519,-15.3442359664661));
#58036=CARTESIAN_POINT('Ctrl Pts',(-66.,-1.96141617445265,-15.4535687378813));
#58037=CARTESIAN_POINT('Ctrl Pts',(-50.,-1.96141617445265,-15.4535687378813));
#58038=CARTESIAN_POINT('Ctrl Pts',(-66.,-2.02269912351901,-15.5623029350202));
#58039=CARTESIAN_POINT('Ctrl Pts',(-50.,-2.02269912351901,-15.5623029350202));
#58040=CARTESIAN_POINT('Ctrl Pts',(-66.,-2.08405759848474,-15.6703081575233));
#58041=CARTESIAN_POINT('Ctrl Pts',(-50.,-2.08405759848474,-15.6703081575233));
#58042=CARTESIAN_POINT('Ctrl Pts',(-66.,-2.14315912151332,-15.777429229659));
#58043=CARTESIAN_POINT('Ctrl Pts',(-50.,-2.14315912151332,-15.777429229659));
#58044=CARTESIAN_POINT('Ctrl Pts',(-66.,-2.19927239636847,-15.8835627084126));
#58045=CARTESIAN_POINT('Ctrl Pts',(-50.,-2.19927239636847,-15.8835627084126));
#58046=CARTESIAN_POINT('Ctrl Pts',(-66.,-2.25471299248206,-15.9887635087906));
#58047=CARTESIAN_POINT('Ctrl Pts',(-50.,-2.25471299248206,-15.9887635087906));
#58048=CARTESIAN_POINT('Ctrl Pts',(-66.,-2.31535412437999,-16.0932944485795));
#58049=CARTESIAN_POINT('Ctrl Pts',(-50.,-2.31535412437999,-16.0932944485795));
#58050=CARTESIAN_POINT('Ctrl Pts',(-66.,-2.38738358844493,-16.1974567620974));
#58051=CARTESIAN_POINT('Ctrl Pts',(-50.,-2.38738358844493,-16.1974567620974));
#58052=CARTESIAN_POINT('Ctrl Pts',(-66.,-2.47452995878914,-16.3014484120242));
#58053=CARTESIAN_POINT('Ctrl Pts',(-50.,-2.47452995878914,-16.3014484120242));
#58054=CARTESIAN_POINT('Ctrl Pts',(-66.,-2.57523216018184,-16.4052181182732));
#58055=CARTESIAN_POINT('Ctrl Pts',(-50.,-2.57523216018184,-16.4052181182732));
#58056=CARTESIAN_POINT('Ctrl Pts',(-66.,-2.67944430952652,-16.5083019863704));
#58057=CARTESIAN_POINT('Ctrl Pts',(-50.,-2.67944430952652,-16.5083019863704));
#58058=CARTESIAN_POINT('Ctrl Pts',(-66.,-2.77108881520607,-16.6099419182707));
#58059=CARTESIAN_POINT('Ctrl Pts',(-50.,-2.77108881520607,-16.6099419182707));
#58060=CARTESIAN_POINT('Ctrl Pts',(-66.,-2.83117825629119,-16.7092375086879));
#58061=CARTESIAN_POINT('Ctrl Pts',(-50.,-2.83117825629119,-16.7092375086879));
#58062=CARTESIAN_POINT('Ctrl Pts',(-66.,-2.84046974884046,-16.805274913915));
#58063=CARTESIAN_POINT('Ctrl Pts',(-50.,-2.84046974884046,-16.805274913915));
#58064=CARTESIAN_POINT('Ctrl Pts',(-66.,-2.78281514699786,-16.8972898402251));
#58065=CARTESIAN_POINT('Ctrl Pts',(-50.,-2.78281514699786,-16.8972898402251));
#58066=CARTESIAN_POINT('Ctrl Pts',(-66.,-2.64606187632854,-16.984711103123));
#58067=CARTESIAN_POINT('Ctrl Pts',(-50.,-2.64606187632854,-16.984711103123));
#58068=CARTESIAN_POINT('Ctrl Pts',(-66.,-2.42115552381383,-17.067116581572));
#58069=CARTESIAN_POINT('Ctrl Pts',(-50.,-2.42115552381383,-17.067116581572));
#58070=CARTESIAN_POINT('Ctrl Pts',(-66.,-2.10178723142879,-17.1442157809099));
#58071=CARTESIAN_POINT('Ctrl Pts',(-50.,-2.10178723142879,-17.1442157809099));
#58072=CARTESIAN_POINT('Ctrl Pts',(-66.,-1.68384299920352,-17.2158227917694));
#58073=CARTESIAN_POINT('Ctrl Pts',(-50.,-1.68384299920352,-17.2158227917694));
#58074=CARTESIAN_POINT('Ctrl Pts',(-66.,-1.16496231481007,-17.2818346267064));
#58075=CARTESIAN_POINT('Ctrl Pts',(-50.,-1.16496231481007,-17.2818346267064));
#58076=CARTESIAN_POINT('Ctrl Pts',(-66.,-0.544072031722875,-17.3422083975502));
#58077=CARTESIAN_POINT('Ctrl Pts',(-50.,-0.544072031722875,-17.3422083975502));
#58078=CARTESIAN_POINT('Ctrl Pts',(-66.,0.0344247852095814,-17.3859937099332));
#58079=CARTESIAN_POINT('Ctrl Pts',(-50.,0.0344247852095814,-17.3859937099332));
#58080=CARTESIAN_POINT('Ctrl Pts',(-66.,0.51421128702247,-17.4162999165388));
#58081=CARTESIAN_POINT('Ctrl Pts',(-50.,0.51421128702247,-17.4162999165388));
#58082=CARTESIAN_POINT('Ctrl Pts',(-66.,0.854447986509492,-17.4353798723759));
#58083=CARTESIAN_POINT('Ctrl Pts',(-50.,0.854447986509492,-17.4353798723759));
#58084=CARTESIAN_POINT('Ctrl Pts',(-66.,1.02966109641534,-17.4446388047024));
#58085=CARTESIAN_POINT('Ctrl Pts',(-50.,1.02966109641534,-17.4446388047024));
#58086=CARTESIAN_POINT('',(-65.5,-2.7865000310617,-16.643348298251));
#58087=CARTESIAN_POINT('Ctrl Pts',(-66.,-2.39254363182917,-16.1992703530064));
#58088=CARTESIAN_POINT('Ctrl Pts',(-65.8407752276778,-2.50356161005854,
-16.3438256470978));
#58089=CARTESIAN_POINT('Ctrl Pts',(-65.7187076779594,-2.62552396821496,
-16.448224027428));
#58090=CARTESIAN_POINT('Ctrl Pts',(-65.5661348005199,-2.74402943200492,
-16.5833869839835));
#58091=CARTESIAN_POINT('Ctrl Pts',(-65.532379579053,-2.76786749699358,-16.6136375795362));
#58092=CARTESIAN_POINT('Ctrl Pts',(-65.5,-2.7865000310617,-16.643348298251));
#58093=CARTESIAN_POINT('',(-66.,-1.57673047345591,-13.9738265075847));
#58094=CARTESIAN_POINT('',(-50.5,-2.7865000310617,-16.643348298251));
#58095=CARTESIAN_POINT('Ctrl Pts',(-50.5,-2.78650003106167,-16.6433482982509));
#58096=CARTESIAN_POINT('Ctrl Pts',(-50.4645575966417,-2.76610413878685,
-16.6108257966901));
#58097=CARTESIAN_POINT('Ctrl Pts',(-50.4275078925308,-2.7394921488981,-16.5776894595399));
#58098=CARTESIAN_POINT('Ctrl Pts',(-50.3892199354571,-2.70928763483811,
-16.5438395577443));
#58099=CARTESIAN_POINT('Ctrl Pts',(-50.3627387584052,-2.68839722579765,
-16.5204278818245));
#58100=CARTESIAN_POINT('Ctrl Pts',(-50.3356652570434,-2.66578887888934,
-16.4966747434728));
#58101=CARTESIAN_POINT('Ctrl Pts',(-50.3081215291836,-2.64231600067803,
-16.4725441298628));
#58102=CARTESIAN_POINT('Ctrl Pts',(-50.287625293614,-2.62484902439342,-16.454587710038));
#58103=CARTESIAN_POINT('Ctrl Pts',(-50.2671206064011,-2.60711322773141,
-16.4366340223856));
#58104=CARTESIAN_POINT('Ctrl Pts',(-50.2463806710782,-2.58922579273126,
-16.4184483377371));
#58105=CARTESIAN_POINT('Ctrl Pts',(-50.2161613181612,-2.56316270706432,
-16.3919506841102));
#58106=CARTESIAN_POINT('Ctrl Pts',(-50.1854425271455,-2.53676748651398,
-16.3649610373556));
#58107=CARTESIAN_POINT('Ctrl Pts',(-50.153522730352,-2.51032301522503,-16.3367318371129));
#58108=CARTESIAN_POINT('Ctrl Pts',(-50.1248133742721,-2.486538285407,-16.3113418834469));
#58109=CARTESIAN_POINT('Ctrl Pts',(-50.0951324534083,-2.46271628719235,
-16.2849492581259));
#58110=CARTESIAN_POINT('Ctrl Pts',(-50.0639695102777,-2.43910032977209,
-16.2569947639715));
#58111=CARTESIAN_POINT('Ctrl Pts',(-50.0433448280462,-2.42347049611539,
-16.2384935410138));
#58112=CARTESIAN_POINT('Ctrl Pts',(-50.0220709849552,-2.40793241896019,
-16.2193079242621));
#58113=CARTESIAN_POINT('Ctrl Pts',(-50.,-2.39254363182917,-16.1992703530065));
#58114=CARTESIAN_POINT('Ctrl Pts',(-65.5,-2.7865000310617,-16.643348298251));
#58115=CARTESIAN_POINT('Ctrl Pts',(-60.5,-2.7865000310617,-16.643348298251));
#58116=CARTESIAN_POINT('Ctrl Pts',(-55.5,-2.7865000310617,-16.643348298251));
#58117=CARTESIAN_POINT('Ctrl Pts',(-50.5,-2.7865000310617,-16.643348298251));
#58118=CARTESIAN_POINT('Origin',(-66.,0.,0.));
#58119=CARTESIAN_POINT('',(-66.,-0.187087378736044,-14.0612554404903));
#58120=CARTESIAN_POINT('Ctrl Pts',(-66.,1.02966109641534,-17.4446388047024));
#58121=CARTESIAN_POINT('Ctrl Pts',(-50.,1.02966109641534,-17.4446388047024));
#58122=CARTESIAN_POINT('Ctrl Pts',(-66.,1.01634258017856,-17.4264925129894));
#58123=CARTESIAN_POINT('Ctrl Pts',(-50.,1.01634258017856,-17.4264925129894));
#58124=CARTESIAN_POINT('Ctrl Pts',(-66.,0.989847264833719,-17.3901577483675));
#58125=CARTESIAN_POINT('Ctrl Pts',(-50.,0.989847264833719,-17.3901577483675));
#58126=CARTESIAN_POINT('Ctrl Pts',(-66.,0.950529442539783,-17.335529057983));
#58127=CARTESIAN_POINT('Ctrl Pts',(-50.,0.950529442539783,-17.335529057983));
#58128=CARTESIAN_POINT('Ctrl Pts',(-66.,0.898957117453771,-17.262437379481));
#58129=CARTESIAN_POINT('Ctrl Pts',(-50.,0.898957117453771,-17.262437379481));
#58130=CARTESIAN_POINT('Ctrl Pts',(-66.,0.835916672953383,-17.1706489753383));
#58131=CARTESIAN_POINT('Ctrl Pts',(-50.,0.835916672953383,-17.1706489753383));
#58132=CARTESIAN_POINT('Ctrl Pts',(-66.,0.774307559809985,-17.0784358527592));
#58133=CARTESIAN_POINT('Ctrl Pts',(-50.,0.774307559809985,-17.0784358527592));
#58134=CARTESIAN_POINT('Ctrl Pts',(-66.,0.714133645526303,-16.9857988139572));
#58135=CARTESIAN_POINT('Ctrl Pts',(-50.,0.714133645526303,-16.9857988139572));
#58136=CARTESIAN_POINT('Ctrl Pts',(-66.,0.655393794508624,-16.892741498413));
#58137=CARTESIAN_POINT('Ctrl Pts',(-50.,0.655393794508624,-16.892741498413));
#58138=CARTESIAN_POINT('Ctrl Pts',(-66.,0.598077690957197,-16.7992718473149));
#58139=CARTESIAN_POINT('Ctrl Pts',(-50.,0.598077690957197,-16.7992718473149));
#58140=CARTESIAN_POINT('Ctrl Pts',(-66.,0.542175324179779,-16.7054008913016));
#58141=CARTESIAN_POINT('Ctrl Pts',(-50.,0.542175324179779,-16.7054008913016));
#58142=CARTESIAN_POINT('Ctrl Pts',(-66.,0.487687945489481,-16.6111412083239));
#58143=CARTESIAN_POINT('Ctrl Pts',(-50.,0.487687945489481,-16.6111412083239));
#58144=CARTESIAN_POINT('Ctrl Pts',(-66.,0.434639273355722,-16.5165054959593));
#58145=CARTESIAN_POINT('Ctrl Pts',(-50.,0.434639273355722,-16.5165054959593));
#58146=CARTESIAN_POINT('Ctrl Pts',(-66.,0.383084538952625,-16.4215052757778));
#58147=CARTESIAN_POINT('Ctrl Pts',(-50.,0.383084538952625,-16.4215052757778));
#58148=CARTESIAN_POINT('Ctrl Pts',(-66.,0.333125583096024,-16.3261492450896));
#58149=CARTESIAN_POINT('Ctrl Pts',(-50.,0.333125583096024,-16.3261492450896));
#58150=CARTESIAN_POINT('Ctrl Pts',(-66.,0.284888522892723,-16.2304441266305));
#58151=CARTESIAN_POINT('Ctrl Pts',(-50.,0.284888522892723,-16.2304441266305));
#58152=CARTESIAN_POINT('Ctrl Pts',(-66.,0.238492193683111,-16.1343961952447));
#58153=CARTESIAN_POINT('Ctrl Pts',(-50.,0.238492193683111,-16.1343961952447));
#58154=CARTESIAN_POINT('Ctrl Pts',(-66.,0.194016921417006,-16.0380127071578));
#58155=CARTESIAN_POINT('Ctrl Pts',(-50.,0.194016921417006,-16.0380127071578));
#58156=CARTESIAN_POINT('Ctrl Pts',(-66.,0.151478606156202,-15.9413031975852));
#58157=CARTESIAN_POINT('Ctrl Pts',(-50.,0.151478606156202,-15.9413031975852));
#58158=CARTESIAN_POINT('Ctrl Pts',(-66.,0.110785127729046,-15.844281437166));
#58159=CARTESIAN_POINT('Ctrl Pts',(-50.,0.110785127729046,-15.844281437166));
#58160=CARTESIAN_POINT('Ctrl Pts',(-66.,0.0717883068748032,-15.7469638696907));
#58161=CARTESIAN_POINT('Ctrl Pts',(-50.,0.0717883068748032,-15.7469638696907));
#58162=CARTESIAN_POINT('Ctrl Pts',(-66.,0.0343674149818962,-15.6493668946876));
#58163=CARTESIAN_POINT('Ctrl Pts',(-50.,0.0343674149818962,-15.6493668946876));
#58164=CARTESIAN_POINT('Ctrl Pts',(-66.,-0.00149271387238248,-15.5515043804903));
#58165=CARTESIAN_POINT('Ctrl Pts',(-50.,-0.00149271387238248,-15.5515043804903));
#58166=CARTESIAN_POINT('Ctrl Pts',(-66.,-0.0356325161212601,-15.4533855207845));
#58167=CARTESIAN_POINT('Ctrl Pts',(-50.,-0.0356325161212601,-15.4533855207845));
#58168=CARTESIAN_POINT('Ctrl Pts',(-66.,-0.0676147251712506,-15.3550114911653));
#58169=CARTESIAN_POINT('Ctrl Pts',(-50.,-0.0676147251712506,-15.3550114911653));
#58170=CARTESIAN_POINT('Ctrl Pts',(-66.,-0.0968131519417803,-15.2563790638913));
#58171=CARTESIAN_POINT('Ctrl Pts',(-50.,-0.0968131519417803,-15.2563790638913));
#58172=CARTESIAN_POINT('Ctrl Pts',(-66.,-0.122566347687195,-15.1574865557124));
#58173=CARTESIAN_POINT('Ctrl Pts',(-50.,-0.122566347687195,-15.1574865557124));
#58174=CARTESIAN_POINT('Ctrl Pts',(-66.,-0.144315282095873,-15.058339300691));
#58175=CARTESIAN_POINT('Ctrl Pts',(-50.,-0.144315282095873,-15.058339300691));
#58176=CARTESIAN_POINT('Ctrl Pts',(-66.,-0.161736107560775,-14.9589547879103));
#58177=CARTESIAN_POINT('Ctrl Pts',(-50.,-0.161736107560775,-14.9589547879103));
#58178=CARTESIAN_POINT('Ctrl Pts',(-66.,-0.174908450355344,-14.8593695705273));
#58179=CARTESIAN_POINT('Ctrl Pts',(-50.,-0.174908450355344,-14.8593695705273));
#58180=CARTESIAN_POINT('Ctrl Pts',(-66.,-0.184238029232279,-14.7596343149665));
#58181=CARTESIAN_POINT('Ctrl Pts',(-50.,-0.184238029232279,-14.7596343149665));
#58182=CARTESIAN_POINT('Ctrl Pts',(-66.,-0.190316238669402,-14.6598058338069));
#58183=CARTESIAN_POINT('Ctrl Pts',(-50.,-0.190316238669402,-14.6598058338069));
#58184=CARTESIAN_POINT('Ctrl Pts',(-66.,-0.19380080315749,-14.5599400753078));
#58185=CARTESIAN_POINT('Ctrl Pts',(-50.,-0.19380080315749,-14.5599400753078));
#58186=CARTESIAN_POINT('Ctrl Pts',(-66.,-0.195293060397626,-14.4600850256186));
#58187=CARTESIAN_POINT('Ctrl Pts',(-50.,-0.195293060397626,-14.4600850256186));
#58188=CARTESIAN_POINT('Ctrl Pts',(-66.,-0.195204987344071,-14.3602728402636));
#58189=CARTESIAN_POINT('Ctrl Pts',(-50.,-0.195204987344071,-14.3602728402636));
#58190=CARTESIAN_POINT('Ctrl Pts',(-66.,-0.193784513213942,-14.2605223532243));
#58191=CARTESIAN_POINT('Ctrl Pts',(-50.,-0.193784513213942,-14.2605223532243));
#58192=CARTESIAN_POINT('Ctrl Pts',(-66.,-0.191684797850075,-14.1807787089954));
#58193=CARTESIAN_POINT('Ctrl Pts',(-50.,-0.191684797850075,-14.1807787089954));
#58194=CARTESIAN_POINT('Ctrl Pts',(-66.,-0.189588581014708,-14.1210041786448));
#58195=CARTESIAN_POINT('Ctrl Pts',(-50.,-0.189588581014708,-14.1210041786448));
#58196=CARTESIAN_POINT('Ctrl Pts',(-66.,-0.187959683517641,-14.0811692301831));
#58197=CARTESIAN_POINT('Ctrl Pts',(-50.,-0.187959683517641,-14.0811692301831));
#58198=CARTESIAN_POINT('Ctrl Pts',(-66.,-0.187087378736032,-14.0612554404903));
#58199=CARTESIAN_POINT('Ctrl Pts',(-50.,-0.187087378736032,-14.0612554404903));
#58200=CARTESIAN_POINT('Origin',(-65.75,0.,0.));
#58201=CARTESIAN_POINT('',(-65.5,-3.57630363704438,-16.4916850956979));
#58202=CARTESIAN_POINT('Origin',(-65.5,0.,0.));
#58203=CARTESIAN_POINT('Ctrl Pts',(-65.5,-3.57630363704438,-16.4916850956979));
#58204=CARTESIAN_POINT('Ctrl Pts',(-65.6677203872149,-3.63345385098673,
-16.3076730899736));
#58205=CARTESIAN_POINT('Ctrl Pts',(-65.8346640232699,-3.68344582376579,
-16.1251870335913));
#58206=CARTESIAN_POINT('Ctrl Pts',(-66.,-3.72562931058621,-15.9455420491152));
#58207=CARTESIAN_POINT('Origin',(-58.,0.,0.));
#58208=CARTESIAN_POINT('',(-50.5,-3.57630363704438,-16.4916850956979));
#58209=CARTESIAN_POINT('Origin',(-50.5,0.,0.));
#58210=CARTESIAN_POINT('Ctrl Pts',(-50.5,-3.57630363704438,-16.4916850956979));
#58211=CARTESIAN_POINT('Ctrl Pts',(-55.5,-3.57630363704438,-16.4916850956979));
#58212=CARTESIAN_POINT('Ctrl Pts',(-60.5,-3.57630363704438,-16.4916850956979));
#58213=CARTESIAN_POINT('Ctrl Pts',(-65.5,-3.57630363704438,-16.4916850956979));
#58214=CARTESIAN_POINT('Origin',(-50.25,0.,0.));
#58215=CARTESIAN_POINT('Ctrl Pts',(-50.,-3.7256293105862,-15.9455420491152));
#58216=CARTESIAN_POINT('Ctrl Pts',(-50.1653359767302,-3.68344582376579,
-16.1251870335914));
#58217=CARTESIAN_POINT('Ctrl Pts',(-50.3322796127843,-3.633453850987,-16.3076730899727));
#58218=CARTESIAN_POINT('Ctrl Pts',(-50.5,-3.57630363704438,-16.4916850956979));
#58219=CARTESIAN_POINT('Ctrl Pts',(-66.,-5.00234392366024,-13.1426961282463));
#58220=CARTESIAN_POINT('Ctrl Pts',(-50.,-5.00234392366024,-13.1426961282463));
#58221=CARTESIAN_POINT('Ctrl Pts',(-66.,-5.00975329143057,-13.1648626726972));
#58222=CARTESIAN_POINT('Ctrl Pts',(-50.,-5.00975329143057,-13.1648626726972));
#58223=CARTESIAN_POINT('Ctrl Pts',(-66.,-5.02478822352796,-13.2091330988228));
#58224=CARTESIAN_POINT('Ctrl Pts',(-50.,-5.02478822352796,-13.2091330988228));
#58225=CARTESIAN_POINT('Ctrl Pts',(-66.,-5.04798920255339,-13.2753507597416));
#58226=CARTESIAN_POINT('Ctrl Pts',(-50.,-5.04798920255339,-13.2753507597416));
#58227=CARTESIAN_POINT('Ctrl Pts',(-66.,-5.08022280379478,-13.3632644309532));
#58228=CARTESIAN_POINT('Ctrl Pts',(-50.,-5.08022280379478,-13.3632644309532));
#58229=CARTESIAN_POINT('Ctrl Pts',(-66.,-5.12272617691501,-13.4724958081193));
#58230=CARTESIAN_POINT('Ctrl Pts',(-50.,-5.12272617691501,-13.4724958081193));
#58231=CARTESIAN_POINT('Ctrl Pts',(-66.,-5.16756435218796,-13.5809703610753));
#58232=CARTESIAN_POINT('Ctrl Pts',(-50.,-5.16756435218796,-13.5809703610753));
#58233=CARTESIAN_POINT('Ctrl Pts',(-66.,-5.21496886213029,-13.6885022424853));
#58234=CARTESIAN_POINT('Ctrl Pts',(-50.,-5.21496886213029,-13.6885022424853));
#58235=CARTESIAN_POINT('Ctrl Pts',(-66.,-5.26532059680125,-13.7947771174053));
#58236=CARTESIAN_POINT('Ctrl Pts',(-50.,-5.26532059680125,-13.7947771174053));
#58237=CARTESIAN_POINT('Ctrl Pts',(-66.,-5.31911705202313,-13.8994109809482));
#58238=CARTESIAN_POINT('Ctrl Pts',(-50.,-5.31911705202313,-13.8994109809482));
#58239=CARTESIAN_POINT('Ctrl Pts',(-66.,-5.37693249048282,-14.0020293939727));
#58240=CARTESIAN_POINT('Ctrl Pts',(-50.,-5.37693249048282,-14.0020293939727));
#58241=CARTESIAN_POINT('Ctrl Pts',(-66.,-5.43936923240832,-14.102334498799));
#58242=CARTESIAN_POINT('Ctrl Pts',(-50.,-5.43936923240832,-14.102334498799));
#58243=CARTESIAN_POINT('Ctrl Pts',(-66.,-5.50704098217782,-14.2001904323636));
#58244=CARTESIAN_POINT('Ctrl Pts',(-50.,-5.50704098217782,-14.2001904323636));
#58245=CARTESIAN_POINT('Ctrl Pts',(-66.,-5.58037590052447,-14.2956379130225));
#58246=CARTESIAN_POINT('Ctrl Pts',(-50.,-5.58037590052447,-14.2956379130225));
#58247=CARTESIAN_POINT('Ctrl Pts',(-66.,-5.65928349609497,-14.3888825985252));
#58248=CARTESIAN_POINT('Ctrl Pts',(-50.,-5.65928349609497,-14.3888825985252));
#58249=CARTESIAN_POINT('Ctrl Pts',(-66.,-5.7429409442582,-14.4802820917477));
#58250=CARTESIAN_POINT('Ctrl Pts',(-50.,-5.7429409442582,-14.4802820917477));
#58251=CARTESIAN_POINT('Ctrl Pts',(-66.,-5.8293396720056,-14.5703597544468));
#58252=CARTESIAN_POINT('Ctrl Pts',(-50.,-5.8293396720056,-14.5703597544468));
#58253=CARTESIAN_POINT('Ctrl Pts',(-66.,-5.91563026424745,-14.6597125620614));
#58254=CARTESIAN_POINT('Ctrl Pts',(-50.,-5.91563026424745,-14.6597125620614));
#58255=CARTESIAN_POINT('Ctrl Pts',(-66.,-5.99951493159239,-14.7487702776409));
#58256=CARTESIAN_POINT('Ctrl Pts',(-50.,-5.99951493159239,-14.7487702776409));
#58257=CARTESIAN_POINT('Ctrl Pts',(-66.,-6.08025962758854,-14.8376145740015));
#58258=CARTESIAN_POINT('Ctrl Pts',(-50.,-6.08025962758854,-14.8376145740015));
#58259=CARTESIAN_POINT('Ctrl Pts',(-66.,-6.16012083060275,-14.925722782193));
#58260=CARTESIAN_POINT('Ctrl Pts',(-50.,-6.16012083060275,-14.925722782193));
#58261=CARTESIAN_POINT('Ctrl Pts',(-66.,-6.2448525974522,-15.0118888540403));
#58262=CARTESIAN_POINT('Ctrl Pts',(-50.,-6.2448525974522,-15.0118888540403));
#58263=CARTESIAN_POINT('Ctrl Pts',(-66.,-6.34052323744621,-15.094865717647));
#58264=CARTESIAN_POINT('Ctrl Pts',(-50.,-6.34052323744621,-15.094865717647));
#58265=CARTESIAN_POINT('Ctrl Pts',(-66.,-6.45079341600148,-15.1739178576564));
#58266=CARTESIAN_POINT('Ctrl Pts',(-50.,-6.45079341600148,-15.1739178576564));
#58267=CARTESIAN_POINT('Ctrl Pts',(-66.,-6.57413834909723,-15.2493838286629));
#58268=CARTESIAN_POINT('Ctrl Pts',(-50.,-6.57413834909723,-15.2493838286629));
#58269=CARTESIAN_POINT('Ctrl Pts',(-66.,-6.70071239766311,-15.323312619824));
#58270=CARTESIAN_POINT('Ctrl Pts',(-50.,-6.70071239766311,-15.323312619824));
#58271=CARTESIAN_POINT('Ctrl Pts',(-66.,-6.81475454587001,-15.3989682845842));
#58272=CARTESIAN_POINT('Ctrl Pts',(-50.,-6.81475454587001,-15.3989682845842));
#58273=CARTESIAN_POINT('Ctrl Pts',(-66.,-6.89764997584352,-15.4802006851134));
#58274=CARTESIAN_POINT('Ctrl Pts',(-50.,-6.89764997584352,-15.4802006851134));
#58275=CARTESIAN_POINT('Ctrl Pts',(-66.,-6.93053309053802,-15.5709101984212));
#58276=CARTESIAN_POINT('Ctrl Pts',(-50.,-6.93053309053802,-15.5709101984212));
#58277=CARTESIAN_POINT('Ctrl Pts',(-66.,-6.89757299567323,-15.6743724230443));
#58278=CARTESIAN_POINT('Ctrl Pts',(-50.,-6.89757299567323,-15.6743724230443));
#58279=CARTESIAN_POINT('Ctrl Pts',(-66.,-6.78685686447956,-15.7930563416641));
#58280=CARTESIAN_POINT('Ctrl Pts',(-50.,-6.78685686447956,-15.7930563416641));
#58281=CARTESIAN_POINT('Ctrl Pts',(-66.,-6.58950976774019,-15.928804835904));
#58282=CARTESIAN_POINT('Ctrl Pts',(-50.,-6.58950976774019,-15.928804835904));
#58283=CARTESIAN_POINT('Ctrl Pts',(-66.,-6.29934880872149,-16.0829054867165));
#58284=CARTESIAN_POINT('Ctrl Pts',(-50.,-6.29934880872149,-16.0829054867165));
#58285=CARTESIAN_POINT('Ctrl Pts',(-66.,-5.91234300254812,-16.2562013356071));
#58286=CARTESIAN_POINT('Ctrl Pts',(-50.,-5.91234300254812,-16.2562013356071));
#58287=CARTESIAN_POINT('Ctrl Pts',(-66.,-5.42618038479175,-16.4491796662161));
#58288=CARTESIAN_POINT('Ctrl Pts',(-50.,-5.42618038479175,-16.4491796662161));
#58289=CARTESIAN_POINT('Ctrl Pts',(-66.,-4.83981085794396,-16.6620658184719));
#58290=CARTESIAN_POINT('Ctrl Pts',(-50.,-4.83981085794396,-16.6620658184719));
#58291=CARTESIAN_POINT('Ctrl Pts',(-66.,-4.29037754669269,-16.8483418428791));
#58292=CARTESIAN_POINT('Ctrl Pts',(-50.,-4.29037754669269,-16.8483418428791));
#58293=CARTESIAN_POINT('Ctrl Pts',(-66.,-3.83320126720106,-16.997013975274));
#58294=CARTESIAN_POINT('Ctrl Pts',(-50.,-3.83320126720106,-16.997013975274));
#58295=CARTESIAN_POINT('Ctrl Pts',(-66.,-3.50839872134417,-17.1001079256176));
#58296=CARTESIAN_POINT('Ctrl Pts',(-50.,-3.50839872134417,-17.1001079256176));
#58297=CARTESIAN_POINT('Ctrl Pts',(-66.,-3.34099285631593,-17.1526497000914));
#58298=CARTESIAN_POINT('Ctrl Pts',(-50.,-3.34099285631593,-17.1526497000914));
#58299=CARTESIAN_POINT('',(-65.5,-6.83798941890817,-15.4274925281751));
#58300=CARTESIAN_POINT('Ctrl Pts',(-66.,-6.34597219029741,-15.0953390806557));
#58301=CARTESIAN_POINT('Ctrl Pts',(-65.793328015403,-6.53220709556297,-15.2412392294586));
#58302=CARTESIAN_POINT('Ctrl Pts',(-65.6370761749492,-6.73030865517213,
-15.3252827538815));
#58303=CARTESIAN_POINT('Ctrl Pts',(-65.5,-6.83798941890817,-15.4274925281751));
#58304=CARTESIAN_POINT('',(-66.,-5.00234392366024,-13.1426961282463));
#58305=CARTESIAN_POINT('',(-50.5,-6.83798941890817,-15.4274925281751));
#58306=CARTESIAN_POINT('Ctrl Pts',(-50.5,-6.83798941890817,-15.4274925281751));
#58307=CARTESIAN_POINT('Ctrl Pts',(-50.4442803165968,-6.79421858808209,
-15.3859455834456));
#58308=CARTESIAN_POINT('Ctrl Pts',(-50.3845456174402,-6.73516562112925,
-15.3467194221617));
#58309=CARTESIAN_POINT('Ctrl Pts',(-50.2235302462153,-6.56816980859925,
-15.2438530879325));
#58310=CARTESIAN_POINT('Ctrl Pts',(-50.1242297628299,-6.45791730059814,
-15.1830391185586));
#58311=CARTESIAN_POINT('Ctrl Pts',(-50.,-6.34597219029741,-15.0953390806557));
#58312=CARTESIAN_POINT('Ctrl Pts',(-65.5,-6.83798941890817,-15.4274925281751));
#58313=CARTESIAN_POINT('Ctrl Pts',(-60.5,-6.83798941890817,-15.4274925281751));
#58314=CARTESIAN_POINT('Ctrl Pts',(-55.5,-6.83798941890817,-15.4274925281751));
#58315=CARTESIAN_POINT('Ctrl Pts',(-50.5,-6.83798941890817,-15.4274925281751));
#58316=CARTESIAN_POINT('Origin',(-66.,0.,0.));
#58317=CARTESIAN_POINT('',(-66.,-3.67810171359515,-13.5729685048794));
#58318=CARTESIAN_POINT('Ctrl Pts',(-66.,-3.34099285631593,-17.1526497000914));
#58319=CARTESIAN_POINT('Ctrl Pts',(-50.,-3.34099285631593,-17.1526497000914));
#58320=CARTESIAN_POINT('Ctrl Pts',(-66.,-3.34938014763553,-17.1317613272011));
#58321=CARTESIAN_POINT('Ctrl Pts',(-50.,-3.34938014763553,-17.1317613272011));
#58322=CARTESIAN_POINT('Ctrl Pts',(-66.,-3.36600697541335,-17.0899789690413));
#58323=CARTESIAN_POINT('Ctrl Pts',(-50.,-3.36600697541335,-17.0899789690413));
#58324=CARTESIAN_POINT('Ctrl Pts',(-66.,-3.39050395317181,-17.0272885946305));
#58325=CARTESIAN_POINT('Ctrl Pts',(-50.,-3.39050395317181,-17.0272885946305));
#58326=CARTESIAN_POINT('Ctrl Pts',(-66.,-3.42227887755104,-16.9436677099084));
#58327=CARTESIAN_POINT('Ctrl Pts',(-50.,-3.42227887755104,-16.9436677099084));
#58328=CARTESIAN_POINT('Ctrl Pts',(-66.,-3.46051194269489,-16.8390854862393));
#58329=CARTESIAN_POINT('Ctrl Pts',(-50.,-3.46051194269489,-16.8390854862393));
#58330=CARTESIAN_POINT('Ctrl Pts',(-66.,-3.49725302120834,-16.7344478450781));
#58331=CARTESIAN_POINT('Ctrl Pts',(-50.,-3.49725302120834,-16.7344478450781));
#58332=CARTESIAN_POINT('Ctrl Pts',(-66.,-3.53249856659576,-16.6297565252442));
#58333=CARTESIAN_POINT('Ctrl Pts',(-50.,-3.53249856659576,-16.6297565252442));
#58334=CARTESIAN_POINT('Ctrl Pts',(-66.,-3.56625058387612,-16.5250147694666));
#58335=CARTESIAN_POINT('Ctrl Pts',(-50.,-3.56625058387612,-16.5250147694666));
#58336=CARTESIAN_POINT('Ctrl Pts',(-66.,-3.59852103965262,-16.4202277040114));
#58337=CARTESIAN_POINT('Ctrl Pts',(-50.,-3.59852103965262,-16.4202277040114));
#58338=CARTESIAN_POINT('Ctrl Pts',(-66.,-3.62932237332147,-16.3154035234118));
#58339=CARTESIAN_POINT('Ctrl Pts',(-50.,-3.62932237332147,-16.3154035234118));
#58340=CARTESIAN_POINT('Ctrl Pts',(-66.,-3.658656500891,-16.2105547216479));
#58341=CARTESIAN_POINT('Ctrl Pts',(-50.,-3.658656500891,-16.2105547216479));
#58342=CARTESIAN_POINT('Ctrl Pts',(-66.,-3.68650360681028,-16.1056994959229));
#58343=CARTESIAN_POINT('Ctrl Pts',(-50.,-3.68650360681028,-16.1056994959229));
#58344=CARTESIAN_POINT('Ctrl Pts',(-66.,-3.712813060392,-16.0008627412701));
#58345=CARTESIAN_POINT('Ctrl Pts',(-50.,-3.712813060392,-16.0008627412701));
#58346=CARTESIAN_POINT('Ctrl Pts',(-66.,-3.73748838326994,-15.8960782085386));
#58347=CARTESIAN_POINT('Ctrl Pts',(-50.,-3.73748838326994,-15.8960782085386));
#58348=CARTESIAN_POINT('Ctrl Pts',(-66.,-3.76040909241452,-15.7913837733062));
#58349=CARTESIAN_POINT('Ctrl Pts',(-50.,-3.76040909241452,-15.7913837733062));
#58350=CARTESIAN_POINT('Ctrl Pts',(-66.,-3.78146164640637,-15.6868150664286));
#58351=CARTESIAN_POINT('Ctrl Pts',(-50.,-3.78146164640637,-15.6868150664286));
#58352=CARTESIAN_POINT('Ctrl Pts',(-66.,-3.80057004743305,-15.5823990924153));
#58353=CARTESIAN_POINT('Ctrl Pts',(-50.,-3.80057004743305,-15.5823990924153));
#58354=CARTESIAN_POINT('Ctrl Pts',(-66.,-3.81772126627406,-15.4781490410999));
#58355=CARTESIAN_POINT('Ctrl Pts',(-50.,-3.81772126627406,-15.4781490410999));
#58356=CARTESIAN_POINT('Ctrl Pts',(-66.,-3.83300795359517,-15.3740553411364));
#58357=CARTESIAN_POINT('Ctrl Pts',(-50.,-3.83300795359517,-15.3740553411364));
#58358=CARTESIAN_POINT('Ctrl Pts',(-66.,-3.84657772273756,-15.2700970690198));
#58359=CARTESIAN_POINT('Ctrl Pts',(-50.,-3.84657772273756,-15.2700970690198));
#58360=CARTESIAN_POINT('Ctrl Pts',(-66.,-3.85855158779829,-15.1662600850723));
#58361=CARTESIAN_POINT('Ctrl Pts',(-50.,-3.85855158779829,-15.1662600850723));
#58362=CARTESIAN_POINT('Ctrl Pts',(-66.,-3.86894768714904,-15.0625540503165));
#58363=CARTESIAN_POINT('Ctrl Pts',(-50.,-3.86894768714904,-15.0625540503165));
#58364=CARTESIAN_POINT('Ctrl Pts',(-66.,-3.87761375658259,-14.9590275514473));
#58365=CARTESIAN_POINT('Ctrl Pts',(-50.,-3.87761375658259,-14.9590275514473));
#58366=CARTESIAN_POINT('Ctrl Pts',(-66.,-3.88412655939816,-14.8557904709058));
#58367=CARTESIAN_POINT('Ctrl Pts',(-50.,-3.88412655939816,-14.8557904709058));
#58368=CARTESIAN_POINT('Ctrl Pts',(-66.,-3.88787877668998,-14.7529954092481));
#58369=CARTESIAN_POINT('Ctrl Pts',(-50.,-3.88787877668998,-14.7529954092481));
#58370=CARTESIAN_POINT('Ctrl Pts',(-66.,-3.88822932173376,-14.6508052317201));
#58371=CARTESIAN_POINT('Ctrl Pts',(-50.,-3.88822932173376,-14.6508052317201));
#58372=CARTESIAN_POINT('Ctrl Pts',(-66.,-3.88463805371054,-14.5493641299902));
#58373=CARTESIAN_POINT('Ctrl Pts',(-50.,-3.88463805371054,-14.5493641299902));
#58374=CARTESIAN_POINT('Ctrl Pts',(-66.,-3.87679564863944,-14.4487695813147));
#58375=CARTESIAN_POINT('Ctrl Pts',(-50.,-3.87679564863944,-14.4487695813147));
#58376=CARTESIAN_POINT('Ctrl Pts',(-66.,-3.86478832158859,-14.3490371882169));
#58377=CARTESIAN_POINT('Ctrl Pts',(-50.,-3.86478832158859,-14.3490371882169));
#58378=CARTESIAN_POINT('Ctrl Pts',(-66.,-3.84902164513744,-14.2501151271916));
#58379=CARTESIAN_POINT('Ctrl Pts',(-50.,-3.84902164513744,-14.2501151271916));
#58380=CARTESIAN_POINT('Ctrl Pts',(-66.,-3.83008256273264,-14.1519113521203));
#58381=CARTESIAN_POINT('Ctrl Pts',(-50.,-3.83008256273264,-14.1519113521203));
#58382=CARTESIAN_POINT('Ctrl Pts',(-66.,-3.8086220490069,-14.0543164841154));
#58383=CARTESIAN_POINT('Ctrl Pts',(-50.,-3.8086220490069,-14.0543164841154));
#58384=CARTESIAN_POINT('Ctrl Pts',(-66.,-3.7852344832017,-13.9572274551481));
#58385=CARTESIAN_POINT('Ctrl Pts',(-50.,-3.7852344832017,-13.9572274551481));
#58386=CARTESIAN_POINT('Ctrl Pts',(-66.,-3.76032689601146,-13.8605729560155));
#58387=CARTESIAN_POINT('Ctrl Pts',(-50.,-3.76032689601146,-13.8605729560155));
#58388=CARTESIAN_POINT('Ctrl Pts',(-66.,-3.73414411132176,-13.764309571506));
#58389=CARTESIAN_POINT('Ctrl Pts',(-50.,-3.73414411132176,-13.764309571506));
#58390=CARTESIAN_POINT('Ctrl Pts',(-66.,-3.71227892449176,-13.6875933984758));
#58391=CARTESIAN_POINT('Ctrl Pts',(-50.,-3.71227892449176,-13.6875933984758));
#58392=CARTESIAN_POINT('Ctrl Pts',(-66.,-3.69538324295473,-13.6302181028421));
#58393=CARTESIAN_POINT('Ctrl Pts',(-50.,-3.69538324295473,-13.6302181028421));
#58394=CARTESIAN_POINT('Ctrl Pts',(-66.,-3.68389897142971,-13.5920397328724));
#58395=CARTESIAN_POINT('Ctrl Pts',(-50.,-3.68389897142971,-13.5920397328724));
#58396=CARTESIAN_POINT('Ctrl Pts',(-66.,-3.67810171359514,-13.5729685048794));
#58397=CARTESIAN_POINT('Ctrl Pts',(-50.,-3.67810171359514,-13.5729685048794));
#58398=CARTESIAN_POINT('Origin',(-65.75,0.,0.));
#58399=CARTESIAN_POINT('',(-65.5,-7.56526278753169,-15.0841779343651));
#58400=CARTESIAN_POINT('Origin',(-65.5,0.,0.));
#58401=CARTESIAN_POINT('Ctrl Pts',(-65.5,-7.56526278753169,-15.0841779343651));
#58402=CARTESIAN_POINT('Ctrl Pts',(-65.6931595476753,-7.57631059668304,
-14.8625452434075));
#58403=CARTESIAN_POINT('Ctrl Pts',(-65.8611256967106,-7.57728353276941,
-14.6730213958903));
#58404=CARTESIAN_POINT('Ctrl Pts',(-66.,-7.57407686781798,-14.5180571909737));
#58405=CARTESIAN_POINT('Origin',(-58.,0.,0.));
#58406=CARTESIAN_POINT('',(-50.5,-7.56526278753169,-15.0841779343651));
#58407=CARTESIAN_POINT('Origin',(-50.5,0.,0.));
#58408=CARTESIAN_POINT('Ctrl Pts',(-50.5,-7.56526278753169,-15.0841779343651));
#58409=CARTESIAN_POINT('Ctrl Pts',(-55.5,-7.56526278753169,-15.0841779343651));
#58410=CARTESIAN_POINT('Ctrl Pts',(-60.5,-7.56526278753169,-15.0841779343651));
#58411=CARTESIAN_POINT('Ctrl Pts',(-65.5,-7.56526278753169,-15.0841779343651));
#58412=CARTESIAN_POINT('Origin',(-50.25,0.,0.));
#58413=CARTESIAN_POINT('Ctrl Pts',(-50.,-7.57407686781798,-14.5180571909737));
#58414=CARTESIAN_POINT('Ctrl Pts',(-50.1388743032875,-7.57728353276935,
-14.6730213958882));
#58415=CARTESIAN_POINT('Ctrl Pts',(-50.3068404523229,-7.57631059668312,
-14.8625452434055));
#58416=CARTESIAN_POINT('Ctrl Pts',(-50.5,-7.56526278753169,-15.0841779343651));
#58417=CARTESIAN_POINT('Ctrl Pts',(-66.,-8.11364170780698,-11.4857618157149));
#58418=CARTESIAN_POINT('Ctrl Pts',(-50.,-8.11364170780698,-11.4857618157149));
#58419=CARTESIAN_POINT('Ctrl Pts',(-66.,-8.12633089210227,-11.5053893225758));
#58420=CARTESIAN_POINT('Ctrl Pts',(-50.,-8.12633089210227,-11.5053893225758));
#58421=CARTESIAN_POINT('Ctrl Pts',(-66.,-8.15190308143842,-11.5445298762901));
#58422=CARTESIAN_POINT('Ctrl Pts',(-50.,-8.15190308143842,-11.5445298762901));
#58423=CARTESIAN_POINT('Ctrl Pts',(-66.,-8.19084282166638,-11.6028973387695));
#58424=CARTESIAN_POINT('Ctrl Pts',(-50.,-8.19084282166638,-11.6028973387695));
#58425=CARTESIAN_POINT('Ctrl Pts',(-66.,-8.24392698602517,-11.6800328696824));
#58426=CARTESIAN_POINT('Ctrl Pts',(-50.,-8.24392698602517,-11.6800328696824));
#58427=CARTESIAN_POINT('Ctrl Pts',(-66.,-8.3122597763829,-11.775262383207));
#58428=CARTESIAN_POINT('Ctrl Pts',(-50.,-8.3122597763829,-11.775262383207));
#58429=CARTESIAN_POINT('Ctrl Pts',(-66.,-8.3826658022629,-11.8691782078618));
#58430=CARTESIAN_POINT('Ctrl Pts',(-50.,-8.3826658022629,-11.8691782078618));
#58431=CARTESIAN_POINT('Ctrl Pts',(-66.,-8.45532310380908,-11.9615427552514));
#58432=CARTESIAN_POINT('Ctrl Pts',(-50.,-8.45532310380908,-11.9615427552514));
#58433=CARTESIAN_POINT('Ctrl Pts',(-66.,-8.53052243279731,-12.0519568423361));
#58434=CARTESIAN_POINT('Ctrl Pts',(-50.,-8.53052243279731,-12.0519568423361));
#58435=CARTESIAN_POINT('Ctrl Pts',(-66.,-8.60865015717173,-12.1399248062686));
#58436=CARTESIAN_POINT('Ctrl Pts',(-50.,-8.60865015717173,-12.1399248062686));
#58437=CARTESIAN_POINT('Ctrl Pts',(-66.,-8.69016937887314,-12.2249411582788));
#58438=CARTESIAN_POINT('Ctrl Pts',(-50.,-8.69016937887314,-12.2249411582788));
#58439=CARTESIAN_POINT('Ctrl Pts',(-66.,-8.77558942093922,-12.3065676074844));
#58440=CARTESIAN_POINT('Ctrl Pts',(-50.,-8.77558942093922,-12.3065676074844));
#58441=CARTESIAN_POINT('Ctrl Pts',(-66.,-8.86547091932666,-12.3845199371372));
#58442=CARTESIAN_POINT('Ctrl Pts',(-50.,-8.86547091932666,-12.3845199371372));
#58443=CARTESIAN_POINT('Ctrl Pts',(-66.,-8.96023870955522,-12.4587311071067));
#58444=CARTESIAN_POINT('Ctrl Pts',(-50.,-8.96023870955522,-12.4587311071067));
#58445=CARTESIAN_POINT('Ctrl Pts',(-66.,-9.05985628822634,-12.5294228183105));
#58446=CARTESIAN_POINT('Ctrl Pts',(-50.,-9.05985628822634,-12.5294228183105));
#58447=CARTESIAN_POINT('Ctrl Pts',(-66.,-9.16361561347667,-12.5971460670373));
#58448=CARTESIAN_POINT('Ctrl Pts',(-50.,-9.16361561347667,-12.5971460670373));
#58449=CARTESIAN_POINT('Ctrl Pts',(-66.,-9.26970137008846,-12.6629072844668));
#58450=CARTESIAN_POINT('Ctrl Pts',(-50.,-9.26970137008846,-12.6629072844668));
#58451=CARTESIAN_POINT('Ctrl Pts',(-66.,-9.37550212434126,-12.7279933116739));
#58452=CARTESIAN_POINT('Ctrl Pts',(-50.,-9.37550212434126,-12.7279933116739));
#58453=CARTESIAN_POINT('Ctrl Pts',(-66.,-9.47889915384706,-12.7933918468958));
#58454=CARTESIAN_POINT('Ctrl Pts',(-50.,-9.47889915384706,-12.7933918468958));
#58455=CARTESIAN_POINT('Ctrl Pts',(-66.,-9.57920178477654,-12.8593645469766));
#58456=CARTESIAN_POINT('Ctrl Pts',(-50.,-9.57920178477654,-12.8593645469766));
#58457=CARTESIAN_POINT('Ctrl Pts',(-66.,-9.67846562159703,-12.9248440002217));
#58458=CARTESIAN_POINT('Ctrl Pts',(-50.,-9.67846562159703,-12.9248440002217));
#58459=CARTESIAN_POINT('Ctrl Pts',(-66.,-9.78196401486522,-12.9872310729365));
#58460=CARTESIAN_POINT('Ctrl Pts',(-50.,-9.78196401486522,-12.9872310729365));
#58461=CARTESIAN_POINT('Ctrl Pts',(-66.,-9.89526449262547,-13.0438087451241));
#58462=CARTESIAN_POINT('Ctrl Pts',(-50.,-9.89526449262547,-13.0438087451241));
#58463=CARTESIAN_POINT('Ctrl Pts',(-66.,-10.0217297985278,-13.0929542385258));
#58464=CARTESIAN_POINT('Ctrl Pts',(-50.,-10.0217297985278,-13.0929542385258));
#58465=CARTESIAN_POINT('Ctrl Pts',(-66.,-10.1599672475493,-13.135374669787));
#58466=CARTESIAN_POINT('Ctrl Pts',(-50.,-10.1599672475493,-13.135374669787));
#58467=CARTESIAN_POINT('Ctrl Pts',(-66.,-10.3009500823582,-13.1755031661724));
#58468=CARTESIAN_POINT('Ctrl Pts',(-50.,-10.3009500823582,-13.1755031661724));
#58469=CARTESIAN_POINT('Ctrl Pts',(-66.,-10.4302241855029,-13.2204208401335));
#58470=CARTESIAN_POINT('Ctrl Pts',(-50.,-10.4302241855029,-13.2204208401335));
#58471=CARTESIAN_POINT('Ctrl Pts',(-66.,-10.5307169796315,-13.2784859202976));
#58472=CARTESIAN_POINT('Ctrl Pts',(-50.,-10.5307169796315,-13.2784859202976));
#58473=CARTESIAN_POINT('Ctrl Pts',(-66.,-10.5851255494393,-13.3581679293586));
#58474=CARTESIAN_POINT('Ctrl Pts',(-50.,-10.5851255494393,-13.3581679293586));
#58475=CARTESIAN_POINT('Ctrl Pts',(-66.,-10.5789309655315,-13.4665765402144));
#58476=CARTESIAN_POINT('Ctrl Pts',(-50.,-10.5789309655315,-13.4665765402144));
#58477=CARTESIAN_POINT('Ctrl Pts',(-66.,-10.5012086755218,-13.6090657674601));
#58478=CARTESIAN_POINT('Ctrl Pts',(-50.,-10.5012086755218,-13.6090657674601));
#58479=CARTESIAN_POINT('Ctrl Pts',(-66.,-10.3438208784378,-13.7896277003499));
#58480=CARTESIAN_POINT('Ctrl Pts',(-50.,-10.3438208784378,-13.7896277003499));
#58481=CARTESIAN_POINT('Ctrl Pts',(-66.,-10.1010991329779,-14.0110470920039));
#58482=CARTESIAN_POINT('Ctrl Pts',(-50.,-10.1010991329779,-14.0110470920039));
#58483=CARTESIAN_POINT('Ctrl Pts',(-66.,-9.76934875096609,-14.2751429634022));
#58484=CARTESIAN_POINT('Ctrl Pts',(-50.,-9.76934875096609,-14.2751429634022));
#58485=CARTESIAN_POINT('Ctrl Pts',(-66.,-9.34645158510148,-14.5829622514464));
#58486=CARTESIAN_POINT('Ctrl Pts',(-50.,-9.34645158510148,-14.5829622514464));
#58487=CARTESIAN_POINT('Ctrl Pts',(-66.,-8.83144656838121,-14.9349843652275));
#58488=CARTESIAN_POINT('Ctrl Pts',(-50.,-8.83144656838121,-14.9349843652275));
#58489=CARTESIAN_POINT('Ctrl Pts',(-66.,-8.34559967843141,-15.25204669397));
#58490=CARTESIAN_POINT('Ctrl Pts',(-50.,-8.34559967843141,-15.25204669397));
#58491=CARTESIAN_POINT('Ctrl Pts',(-66.,-7.93975968827824,-15.509743135298));
#58492=CARTESIAN_POINT('Ctrl Pts',(-50.,-7.93975968827824,-15.509743135298));
#58493=CARTESIAN_POINT('Ctrl Pts',(-66.,-7.65079983454787,-15.6903733080951));
#58494=CARTESIAN_POINT('Ctrl Pts',(-50.,-7.65079983454787,-15.6903733080951));
#58495=CARTESIAN_POINT('Ctrl Pts',(-66.,-7.50171994057268,-15.7828965317908));
#58496=CARTESIAN_POINT('Ctrl Pts',(-50.,-7.50171994057268,-15.7828965317908));
#58497=CARTESIAN_POINT('',(-65.5,-10.4598227831987,-13.2422706642055));
#58498=CARTESIAN_POINT('Ctrl Pts',(-66.,-9.90065997719615,-13.0429121370937));
#58499=CARTESIAN_POINT('Ctrl Pts',(-65.7933280154041,-10.1173278619927,
-13.1379138268532));
#58500=CARTESIAN_POINT('Ctrl Pts',(-65.6370761749487,-10.3301064714307,
-13.1700511149055));
#58501=CARTESIAN_POINT('Ctrl Pts',(-65.5,-10.4598227831987,-13.2422706642055));
#58502=CARTESIAN_POINT('',(-66.,-8.11364170780698,-11.4857618157149));
#58503=CARTESIAN_POINT('',(-50.5,-10.4598227831987,-13.2422706642055));
#58504=CARTESIAN_POINT('Ctrl Pts',(-50.5,-10.4598227831987,-13.2422706642055));
#58505=CARTESIAN_POINT('Ctrl Pts',(-50.4518618349117,-10.4142692416525,
-13.2169087325051));
#58506=CARTESIAN_POINT('Ctrl Pts',(-50.4012423593874,-10.3586165910348,
-13.1963094071548));
#58507=CARTESIAN_POINT('Ctrl Pts',(-50.2441129793791,-10.1781263556467,
-13.1379513556689));
#58508=CARTESIAN_POINT('Ctrl Pts',(-50.1366827452935,-10.0439535221284,
-13.105741609551));
#58509=CARTESIAN_POINT('Ctrl Pts',(-50.,-9.90065997719615,-13.0429121370937));
#58510=CARTESIAN_POINT('Ctrl Pts',(-65.5,-10.4598227831987,-13.2422706642055));
#58511=CARTESIAN_POINT('Ctrl Pts',(-60.5,-10.4598227831987,-13.2422706642055));
#58512=CARTESIAN_POINT('Ctrl Pts',(-55.5,-10.4598227831987,-13.2422706642055));
#58513=CARTESIAN_POINT('Ctrl Pts',(-50.5,-10.4598227831987,-13.2422706642055));
#58514=CARTESIAN_POINT('Origin',(-66.,0.,0.));
#58515=CARTESIAN_POINT('',(-66.,-6.93800739067722,-12.2318420402206));
#58516=CARTESIAN_POINT('Ctrl Pts',(-66.,-7.50171994057268,-15.7828965317908));
#58517=CARTESIAN_POINT('Ctrl Pts',(-50.,-7.50171994057268,-15.7828965317908));
#58518=CARTESIAN_POINT('Ctrl Pts',(-66.,-7.50464900261518,-15.760578571014));
#58519=CARTESIAN_POINT('Ctrl Pts',(-50.,-7.50464900261518,-15.760578571014));
#58520=CARTESIAN_POINT('Ctrl Pts',(-66.,-7.5103626180875,-15.7159739585441));
#58521=CARTESIAN_POINT('Ctrl Pts',(-50.,-7.5103626180875,-15.7159739585441));
#58522=CARTESIAN_POINT('Ctrl Pts',(-66.,-7.51849951610435,-15.6491609668904));
#58523=CARTESIAN_POINT('Ctrl Pts',(-50.,-7.51849951610435,-15.6491609668904));
#58524=CARTESIAN_POINT('Ctrl Pts',(-66.,-7.52848050441805,-15.5602650836714));
#58525=CARTESIAN_POINT('Ctrl Pts',(-50.,-7.52848050441805,-15.5602650836714));
#58526=CARTESIAN_POINT('Ctrl Pts',(-66.,-7.53950386611099,-15.4494603262155));
#58527=CARTESIAN_POINT('Ctrl Pts',(-50.,-7.53950386611099,-15.4494603262155));
#58528=CARTESIAN_POINT('Ctrl Pts',(-66.,-7.54906833290726,-15.3389729342967));
#58529=CARTESIAN_POINT('Ctrl Pts',(-50.,-7.54906833290726,-15.3389729342967));
#58530=CARTESIAN_POINT('Ctrl Pts',(-66.,-7.55717090215767,-15.2288054740838));
#58531=CARTESIAN_POINT('Ctrl Pts',(-50.,-7.55717090215767,-15.2288054740838));
#58532=CARTESIAN_POINT('Ctrl Pts',(-66.,-7.56381432232377,-15.1189605878015));
#58533=CARTESIAN_POINT('Ctrl Pts',(-50.,-7.56381432232377,-15.1189605878015));
#58534=CARTESIAN_POINT('Ctrl Pts',(-66.,-7.56901145890645,-15.0094402646918));
#58535=CARTESIAN_POINT('Ctrl Pts',(-50.,-7.56901145890645,-15.0094402646918));
#58536=CARTESIAN_POINT('Ctrl Pts',(-66.,-7.57277639839295,-14.9002493482892));
#58537=CARTESIAN_POINT('Ctrl Pts',(-50.,-7.57277639839295,-14.9002493482892));
#58538=CARTESIAN_POINT('Ctrl Pts',(-66.,-7.57511410372315,-14.7913994635608));
#58539=CARTESIAN_POINT('Ctrl Pts',(-50.,-7.57511410372315,-14.7913994635608));
#58540=CARTESIAN_POINT('Ctrl Pts',(-66.,-7.57600990734854,-14.6829131639384));
#58541=CARTESIAN_POINT('Ctrl Pts',(-50.,-7.57600990734854,-14.6829131639384));
#58542=CARTESIAN_POINT('Ctrl Pts',(-66.,-7.57542096038094,-14.5748271536716));
#58543=CARTESIAN_POINT('Ctrl Pts',(-50.,-7.57542096038094,-14.5748271536716));
#58544=CARTESIAN_POINT('Ctrl Pts',(-66.,-7.57326220899431,-14.4671981164589));
#58545=CARTESIAN_POINT('Ctrl Pts',(-50.,-7.57326220899431,-14.4671981164589));
#58546=CARTESIAN_POINT('Ctrl Pts',(-66.,-7.56942637462814,-14.360092700858));
#58547=CARTESIAN_POINT('Ctrl Pts',(-50.,-7.56942637462814,-14.360092700858));
#58548=CARTESIAN_POINT('Ctrl Pts',(-66.,-7.56381234400904,-14.2535736549186));
#58549=CARTESIAN_POINT('Ctrl Pts',(-50.,-7.56381234400904,-14.2535736549186));
#58550=CARTESIAN_POINT('Ctrl Pts',(-66.,-7.556353222684,-14.1476860346413));
#58551=CARTESIAN_POINT('Ctrl Pts',(-50.,-7.556353222684,-14.1476860346413));
#58552=CARTESIAN_POINT('Ctrl Pts',(-66.,-7.54703967094767,-14.0424458557121));
#58553=CARTESIAN_POINT('Ctrl Pts',(-50.,-7.54703967094767,-14.0424458557121));
#58554=CARTESIAN_POINT('Ctrl Pts',(-66.,-7.53595904837785,-13.9378208062029));
#58555=CARTESIAN_POINT('Ctrl Pts',(-50.,-7.53595904837785,-13.9378208062029));
#58556=CARTESIAN_POINT('Ctrl Pts',(-66.,-7.52324912730704,-13.8337539100138));
#58557=CARTESIAN_POINT('Ctrl Pts',(-50.,-7.52324912730704,-13.8337539100138));
#58558=CARTESIAN_POINT('Ctrl Pts',(-66.,-7.50902360355704,-13.730201376709));
#58559=CARTESIAN_POINT('Ctrl Pts',(-50.,-7.50902360355704,-13.730201376709));
#58560=CARTESIAN_POINT('Ctrl Pts',(-66.,-7.49330244824787,-13.6271680529626));
#58561=CARTESIAN_POINT('Ctrl Pts',(-50.,-7.49330244824787,-13.6271680529626));
#58562=CARTESIAN_POINT('Ctrl Pts',(-66.,-7.47595026385202,-13.5247388655977));
#58563=CARTESIAN_POINT('Ctrl Pts',(-50.,-7.47595026385202,-13.5247388655977));
#58564=CARTESIAN_POINT('Ctrl Pts',(-66.,-7.45658443707985,-13.4231254995838));
#58565=CARTESIAN_POINT('Ctrl Pts',(-50.,-7.45658443707985,-13.4231254995838));
#58566=CARTESIAN_POINT('Ctrl Pts',(-66.,-7.43465467928082,-13.32262679532));
#58567=CARTESIAN_POINT('Ctrl Pts',(-50.,-7.43465467928082,-13.32262679532));
#58568=CARTESIAN_POINT('Ctrl Pts',(-66.,-7.40958054758866,-13.2235599331263));
#58569=CARTESIAN_POINT('Ctrl Pts',(-50.,-7.40958054758866,-13.2235599331263));
#58570=CARTESIAN_POINT('Ctrl Pts',(-66.,-7.38087472971119,-13.1261989021839));
#58571=CARTESIAN_POINT('Ctrl Pts',(-50.,-7.38087472971119,-13.1261989021839));
#58572=CARTESIAN_POINT('Ctrl Pts',(-66.,-7.34826186125705,-13.0307150430677));
#58573=CARTESIAN_POINT('Ctrl Pts',(-50.,-7.34826186125705,-13.0307150430677));
#58574=CARTESIAN_POINT('Ctrl Pts',(-66.,-7.31182932887926,-12.9371020273035));
#58575=CARTESIAN_POINT('Ctrl Pts',(-50.,-7.31182932887926,-12.9371020273035));
#58576=CARTESIAN_POINT('Ctrl Pts',(-66.,-7.27195707536722,-12.8452087977179));
#58577=CARTESIAN_POINT('Ctrl Pts',(-50.,-7.27195707536722,-12.8452087977179));
#58578=CARTESIAN_POINT('Ctrl Pts',(-66.,-7.22919071332107,-12.7548002330908));
#58579=CARTESIAN_POINT('Ctrl Pts',(-50.,-7.22919071332107,-12.7548002330908));
#58580=CARTESIAN_POINT('Ctrl Pts',(-66.,-7.18413356438513,-12.6656085000656));
#58581=CARTESIAN_POINT('Ctrl Pts',(-50.,-7.18413356438513,-12.6656085000656));
#58582=CARTESIAN_POINT('Ctrl Pts',(-66.,-7.13733570230759,-12.5773859525787));
#58583=CARTESIAN_POINT('Ctrl Pts',(-50.,-7.13733570230759,-12.5773859525787));
#58584=CARTESIAN_POINT('Ctrl Pts',(-66.,-7.08917363628753,-12.4899622973194));
#58585=CARTESIAN_POINT('Ctrl Pts',(-50.,-7.08917363628753,-12.4899622973194));
#58586=CARTESIAN_POINT('Ctrl Pts',(-66.,-7.03987370169386,-12.4032345978205));
#58587=CARTESIAN_POINT('Ctrl Pts',(-50.,-7.03987370169386,-12.4032345978205));
#58588=CARTESIAN_POINT('Ctrl Pts',(-66.,-6.99961691350077,-12.3343662552827));
#58589=CARTESIAN_POINT('Ctrl Pts',(-50.,-6.99961691350077,-12.3343662552827));
#58590=CARTESIAN_POINT('Ctrl Pts',(-66.,-6.96898338507103,-12.2829952952022));
#58591=CARTESIAN_POINT('Ctrl Pts',(-50.,-6.96898338507103,-12.2829952952022));
#58592=CARTESIAN_POINT('Ctrl Pts',(-66.,-6.94836533853418,-12.24887239112));
#58593=CARTESIAN_POINT('Ctrl Pts',(-50.,-6.94836533853418,-12.24887239112));
#58594=CARTESIAN_POINT('Ctrl Pts',(-66.,-6.93800739067721,-12.2318420402206));
#58595=CARTESIAN_POINT('Ctrl Pts',(-50.,-6.93800739067721,-12.2318420402206));
#58596=CARTESIAN_POINT('Origin',(-65.75,0.,0.));
#58597=CARTESIAN_POINT('',(-65.5,-11.0788686539881,-12.7288763976904));
#58598=CARTESIAN_POINT('Origin',(-65.5,0.,0.));
#58599=CARTESIAN_POINT('Ctrl Pts',(-65.5,-11.0788686539881,-12.7288763976904));
#58600=CARTESIAN_POINT('Ctrl Pts',(-65.693159547666,-11.0344515669953,-12.5114592268724));
#58601=CARTESIAN_POINT('Ctrl Pts',(-65.8611256966936,-10.9882612722543,
-12.3276476601772));
#58602=CARTESIAN_POINT('Ctrl Pts',(-66.,-10.9466173199385,-12.178349405844));
#58603=CARTESIAN_POINT('Origin',(-58.,0.,0.));
#58604=CARTESIAN_POINT('',(-50.5,-11.0788686539881,-12.7288763976904));
#58605=CARTESIAN_POINT('Origin',(-50.5,0.,0.));
#58606=CARTESIAN_POINT('Ctrl Pts',(-50.5,-11.0788686539881,-12.7288763976904));
#58607=CARTESIAN_POINT('Ctrl Pts',(-55.5,-11.0788686539881,-12.7288763976904));
#58608=CARTESIAN_POINT('Ctrl Pts',(-60.5,-11.0788686539881,-12.7288763976904));
#58609=CARTESIAN_POINT('Ctrl Pts',(-65.5,-11.0788686539881,-12.7288763976904));
#58610=CARTESIAN_POINT('Origin',(-50.25,0.,0.));
#58611=CARTESIAN_POINT('Ctrl Pts',(-50.,-10.9466173199385,-12.178349405844));
#58612=CARTESIAN_POINT('Ctrl Pts',(-50.1388743032945,-10.9882612722507,
-12.3276476601644));
#58613=CARTESIAN_POINT('Ctrl Pts',(-50.3068404523294,-11.0344515669942,
-12.5114592268673));
#58614=CARTESIAN_POINT('Ctrl Pts',(-50.5,-11.0788686539881,-12.7288763976904));
#58615=CARTESIAN_POINT('Ctrl Pts',(-66.,-10.7151295435653,-9.10713484662511));
#58616=CARTESIAN_POINT('Ctrl Pts',(-50.,-10.7151295435653,-9.10713484662511));
#58617=CARTESIAN_POINT('Ctrl Pts',(-66.,-10.7323012362688,-9.12299004745485));
#58618=CARTESIAN_POINT('Ctrl Pts',(-50.,-10.7323012362688,-9.12299004745485));
#58619=CARTESIAN_POINT('Ctrl Pts',(-66.,-10.7668038881397,-9.15454138381928));
#58620=CARTESIAN_POINT('Ctrl Pts',(-50.,-10.7668038881397,-9.15454138381928));
#58621=CARTESIAN_POINT('Ctrl Pts',(-66.,-10.8190356624814,-9.20139120553108));
#58622=CARTESIAN_POINT('Ctrl Pts',(-50.,-10.8190356624814,-9.20139120553108));
#58623=CARTESIAN_POINT('Ctrl Pts',(-66.,-10.889634916681,-9.26290188705335));
#58624=CARTESIAN_POINT('Ctrl Pts',(-50.,-10.889634916681,-9.26290188705335));
#58625=CARTESIAN_POINT('Ctrl Pts',(-66.,-10.9795035237476,-9.33814591637203));
#58626=CARTESIAN_POINT('Ctrl Pts',(-50.,-10.9795035237476,-9.33814591637203));
#58627=CARTESIAN_POINT('Ctrl Pts',(-66.,-11.0710535306934,-9.4116019360644));
#58628=CARTESIAN_POINT('Ctrl Pts',(-50.,-11.0710535306934,-9.4116019360644));
#58629=CARTESIAN_POINT('Ctrl Pts',(-66.,-11.1643982983724,-9.48299554522798));
#58630=CARTESIAN_POINT('Ctrl Pts',(-50.,-11.1643982983724,-9.48299554522798));
#58631=CARTESIAN_POINT('Ctrl Pts',(-66.,-11.2597201712738,-9.55186779486609));
#58632=CARTESIAN_POINT('Ctrl Pts',(-50.,-11.2597201712738,-9.55186779486609));
#58633=CARTESIAN_POINT('Ctrl Pts',(-66.,-11.3572701125446,-9.61764250849074));
#58634=CARTESIAN_POINT('Ctrl Pts',(-50.,-11.3572701125446,-9.61764250849074));
#58635=CARTESIAN_POINT('Ctrl Pts',(-66.,-11.4573709649815,-9.6797149094218));
#58636=CARTESIAN_POINT('Ctrl Pts',(-50.,-11.4573709649815,-9.6797149094218));
#58637=CARTESIAN_POINT('Ctrl Pts',(-66.,-11.5604070517922,-9.73753381300202));
#58638=CARTESIAN_POINT('Ctrl Pts',(-50.,-11.5604070517922,-9.73753381300202));
#58639=CARTESIAN_POINT('Ctrl Pts',(-66.,-11.6668507136929,-9.79068450718227));
#58640=CARTESIAN_POINT('Ctrl Pts',(-50.,-11.6668507136929,-9.79068450718227));
#58641=CARTESIAN_POINT('Ctrl Pts',(-66.,-11.7770967670118,-9.83899640572359));
#58642=CARTESIAN_POINT('Ctrl Pts',(-50.,-11.7770967670118,-9.83899640572359));
#58643=CARTESIAN_POINT('Ctrl Pts',(-66.,-11.8911649899478,-9.88269332242761));
#58644=CARTESIAN_POINT('Ctrl Pts',(-50.,-11.8911649899478,-9.88269332242761));
#58645=CARTESIAN_POINT('Ctrl Pts',(-66.,-12.0085066122796,-9.9224850258725));
#58646=CARTESIAN_POINT('Ctrl Pts',(-50.,-12.0085066122796,-9.9224850258725));
#58647=CARTESIAN_POINT('Ctrl Pts',(-66.,-12.1276136395118,-9.95979777888845));
#58648=CARTESIAN_POINT('Ctrl Pts',(-50.,-12.1276136395118,-9.95979777888845));
#58649=CARTESIAN_POINT('Ctrl Pts',(-66.,-12.2462767052779,-9.99652743122885));
#58650=CARTESIAN_POINT('Ctrl Pts',(-50.,-12.2462767052779,-9.99652743122885));
#58651=CARTESIAN_POINT('Ctrl Pts',(-66.,-12.362689281313,-10.0341575556064));
#58652=CARTESIAN_POINT('Ctrl Pts',(-50.,-12.362689281313,-10.0341575556064));
#58653=CARTESIAN_POINT('Ctrl Pts',(-66.,-12.4762474639872,-10.0731133520306));
#58654=CARTESIAN_POINT('Ctrl Pts',(-50.,-12.4762474639872,-10.0731133520306));
#58655=CARTESIAN_POINT('Ctrl Pts',(-66.,-12.5886768226797,-10.1118497354652));
#58656=CARTESIAN_POINT('Ctrl Pts',(-50.,-12.5886768226797,-10.1118497354652));
#58657=CARTESIAN_POINT('Ctrl Pts',(-66.,-12.7044386576771,-10.1465377998253));
#58658=CARTESIAN_POINT('Ctrl Pts',(-50.,-12.7044386576771,-10.1465377998253));
#58659=CARTESIAN_POINT('Ctrl Pts',(-66.,-12.8282498874959,-10.1731612973722));
#58660=CARTESIAN_POINT('Ctrl Pts',(-50.,-12.8282498874959,-10.1731612973722));
#58661=CARTESIAN_POINT('Ctrl Pts',(-66.,-12.9629640404687,-10.1893121520713));
#58662=CARTESIAN_POINT('Ctrl Pts',(-50.,-12.9629640404687,-10.1893121520713));
#58663=CARTESIAN_POINT('Ctrl Pts',(-66.,-13.1074080380921,-10.1960216118796));
#58664=CARTESIAN_POINT('Ctrl Pts',(-50.,-13.1074080380921,-10.1960216118796));
#58665=CARTESIAN_POINT('Ctrl Pts',(-66.,-13.2539411891343,-10.1998283924791));
#58666=CARTESIAN_POINT('Ctrl Pts',(-50.,-13.2539411891343,-10.1998283924791));
#58667=CARTESIAN_POINT('Ctrl Pts',(-66.,-13.3903244798794,-10.2111857329905));
#58668=CARTESIAN_POINT('Ctrl Pts',(-50.,-13.3903244798794,-10.2111857329905));
#58669=CARTESIAN_POINT('Ctrl Pts',(-66.,-13.5021003063213,-10.2424350502543));
#58670=CARTESIAN_POINT('Ctrl Pts',(-50.,-13.5021003063213,-10.2424350502543));
#58671=CARTESIAN_POINT('Ctrl Pts',(-66.,-13.5746156407008,-10.3060828413894));
#58672=CARTESIAN_POINT('Ctrl Pts',(-50.,-13.5746156407008,-10.3060828413894));
#58673=CARTESIAN_POINT('Ctrl Pts',(-66.,-13.5955757962388,-10.4126261267587));
#58674=CARTESIAN_POINT('Ctrl Pts',(-50.,-13.5955757962388,-10.4126261267587));
#58675=CARTESIAN_POINT('Ctrl Pts',(-66.,-13.5557309247371,-10.5699675404438));
#58676=CARTESIAN_POINT('Ctrl Pts',(-50.,-13.5557309247371,-10.5699675404438));
#58677=CARTESIAN_POINT('Ctrl Pts',(-66.,-13.448191681431,-10.7839975416797));
#58678=CARTESIAN_POINT('Ctrl Pts',(-50.,-13.448191681431,-10.7839975416797));
#58679=CARTESIAN_POINT('Ctrl Pts',(-66.,-13.2681602494653,-11.0588230794739));
#58680=CARTESIAN_POINT('Ctrl Pts',(-50.,-13.2681602494653,-11.0588230794739));
#58681=CARTESIAN_POINT('Ctrl Pts',(-66.,-13.0125103882094,-11.3971248585033));
#58682=CARTESIAN_POINT('Ctrl Pts',(-50.,-13.0125103882094,-11.3971248585033));
#58683=CARTESIAN_POINT('Ctrl Pts',(-66.,-12.6794508584748,-11.8004436860348));
#58684=CARTESIAN_POINT('Ctrl Pts',(-50.,-12.6794508584748,-11.8004436860348));
#58685=CARTESIAN_POINT('Ctrl Pts',(-66.,-12.2681700111386,-12.2694829172856));
#58686=CARTESIAN_POINT('Ctrl Pts',(-50.,-12.2681700111386,-12.2694829172856));
#58687=CARTESIAN_POINT('Ctrl Pts',(-66.,-11.8764370894057,-12.6974093581748));
#58688=CARTESIAN_POINT('Ctrl Pts',(-50.,-11.8764370894057,-12.6974093581748));
#58689=CARTESIAN_POINT('Ctrl Pts',(-66.,-11.5474338077474,-13.0479380932861));
#58690=CARTESIAN_POINT('Ctrl Pts',(-50.,-11.5474338077474,-13.0479380932861));
#58691=CARTESIAN_POINT('Ctrl Pts',(-66.,-11.3124730564734,-13.2947548304684));
#58692=CARTESIAN_POINT('Ctrl Pts',(-50.,-11.3124730564734,-13.2947548304684));
#58693=CARTESIAN_POINT('Ctrl Pts',(-66.,-11.1910863715672,-13.4214459289647));
#58694=CARTESIAN_POINT('Ctrl Pts',(-50.,-11.1910863715672,-13.4214459289647));
#58695=CARTESIAN_POINT('',(-65.5,-13.4244270134836,-10.224988232739));
#58696=CARTESIAN_POINT('Ctrl Pts',(-66.,-12.8332528856473,-10.1709510554827));
#58697=CARTESIAN_POINT('Ctrl Pts',(-65.7933280154042,-13.0667397099252,
-10.2090849806402));
#58698=CARTESIAN_POINT('Ctrl Pts',(-65.6370761749484,-13.2808257066153,
-10.1872967283199));
#58699=CARTESIAN_POINT('Ctrl Pts',(-65.5,-13.4244270134836,-10.224988232739));
#58700=CARTESIAN_POINT('',(-66.,-10.7151295435653,-9.10713484662511));
#58701=CARTESIAN_POINT('',(-50.5,-13.4244270134836,-10.224988232739));
#58702=CARTESIAN_POINT('Ctrl Pts',(-50.5,-13.4244270134836,-10.224988232739));
#58703=CARTESIAN_POINT('Ctrl Pts',(-50.4518618349118,-13.3739973642794,
-10.2117517978674));
#58704=CARTESIAN_POINT('Ctrl Pts',(-50.4012423593876,-13.3149703001221,
-10.205639889605));
#58705=CARTESIAN_POINT('Ctrl Pts',(-50.2441129793791,-13.1256374401377,
-10.1940013598926));
#58706=CARTESIAN_POINT('Ctrl Pts',(-50.1366827452936,-12.9876696547833,
-10.1961709690068));
#58707=CARTESIAN_POINT('Ctrl Pts',(-50.,-12.8332528856473,-10.1709510554827));
#58708=CARTESIAN_POINT('Ctrl Pts',(-65.5,-13.4244270134836,-10.224988232739));
#58709=CARTESIAN_POINT('Ctrl Pts',(-60.5,-13.4244270134836,-10.224988232739));
#58710=CARTESIAN_POINT('Ctrl Pts',(-55.5,-13.4244270134836,-10.224988232739));
#58711=CARTESIAN_POINT('Ctrl Pts',(-50.5,-13.4244270134836,-10.224988232739));
#58712=CARTESIAN_POINT('Origin',(-66.,0.,0.));
#58713=CARTESIAN_POINT('',(-66.,-9.76197254719673,-10.1221439546065));
#58714=CARTESIAN_POINT('Ctrl Pts',(-66.,-11.1910863715672,-13.4214459289647));
#58715=CARTESIAN_POINT('Ctrl Pts',(-50.,-11.1910863715672,-13.4214459289647));
#58716=CARTESIAN_POINT('Ctrl Pts',(-66.,-11.1883731605921,-13.3991006998567));
#58717=CARTESIAN_POINT('Ctrl Pts',(-50.,-11.1883731605921,-13.3991006998567));
#58718=CARTESIAN_POINT('Ctrl Pts',(-66.,-11.1828145562856,-13.3544765049226));
#58719=CARTESIAN_POINT('Ctrl Pts',(-50.,-11.1828145562856,-13.3544765049226));
#58720=CARTESIAN_POINT('Ctrl Pts',(-66.,-11.1740801033331,-13.2877390020125));
#58721=CARTESIAN_POINT('Ctrl Pts',(-50.,-11.1740801033331,-13.2877390020125));
#58722=CARTESIAN_POINT('Ctrl Pts',(-66.,-11.161640013378,-13.1991537755753));
#58723=CARTESIAN_POINT('Ctrl Pts',(-50.,-11.161640013378,-13.1991537755753));
#58724=CARTESIAN_POINT('Ctrl Pts',(-66.,-11.1447610332637,-13.089088754755));
#58725=CARTESIAN_POINT('Ctrl Pts',(-50.,-11.1447610332637,-13.089088754755));
#58726=CARTESIAN_POINT('Ctrl Pts',(-66.,-11.1265479177184,-12.9796939412571));
#58727=CARTESIAN_POINT('Ctrl Pts',(-50.,-11.1265479177184,-12.9796939412571));
#58728=CARTESIAN_POINT('Ctrl Pts',(-66.,-11.1069983966066,-12.870972567358));
#58729=CARTESIAN_POINT('Ctrl Pts',(-50.,-11.1069983966066,-12.870972567358));
#58730=CARTESIAN_POINT('Ctrl Pts',(-66.,-11.0861157891366,-12.7629265087573));
#58731=CARTESIAN_POINT('Ctrl Pts',(-50.,-11.0861157891366,-12.7629265087573));
#58732=CARTESIAN_POINT('Ctrl Pts',(-66.,-11.0639130513203,-12.6555544926816));
#58733=CARTESIAN_POINT('Ctrl Pts',(-50.,-11.0639130513203,-12.6555544926816));
#58734=CARTESIAN_POINT('Ctrl Pts',(-66.,-11.04040503163,-12.5488577073298));
#58735=CARTESIAN_POINT('Ctrl Pts',(-50.,-11.04040503163,-12.5488577073298));
#58736=CARTESIAN_POINT('Ctrl Pts',(-66.,-11.0155994280975,-12.4428461782163));
#58737=CARTESIAN_POINT('Ctrl Pts',(-50.,-11.0155994280975,-12.4428461782163));
#58738=CARTESIAN_POINT('Ctrl Pts',(-66.,-10.9894876427927,-12.3375453978863));
#58739=CARTESIAN_POINT('Ctrl Pts',(-50.,-10.9894876427927,-12.3375453978863));
#58740=CARTESIAN_POINT('Ctrl Pts',(-66.,-10.9620373009797,-12.2330015735433));
#58741=CARTESIAN_POINT('Ctrl Pts',(-50.,-10.9620373009797,-12.2330015735433));
#58742=CARTESIAN_POINT('Ctrl Pts',(-66.,-10.9331801176175,-12.1292907600893));
#58743=CARTESIAN_POINT('Ctrl Pts',(-50.,-10.9331801176175,-12.1292907600893));
#58744=CARTESIAN_POINT('Ctrl Pts',(-66.,-10.902828759321,-12.0265041912883));
#58745=CARTESIAN_POINT('Ctrl Pts',(-50.,-10.902828759321,-12.0265041912883));
#58746=CARTESIAN_POINT('Ctrl Pts',(-66.,-10.8709008942817,-11.9247277896931));
#58747=CARTESIAN_POINT('Ctrl Pts',(-50.,-10.8709008942817,-11.9247277896931));
#58748=CARTESIAN_POINT('Ctrl Pts',(-66.,-10.8373429346305,-11.8240218317612));
#58749=CARTESIAN_POINT('Ctrl Pts',(-50.,-10.8373429346305,-11.8240218317612));
#58750=CARTESIAN_POINT('Ctrl Pts',(-66.,-10.8021498170253,-11.7244041527066));
#58751=CARTESIAN_POINT('Ctrl Pts',(-50.,-10.8021498170253,-11.7244041527066));
#58752=CARTESIAN_POINT('Ctrl Pts',(-66.,-10.7653981208323,-11.6258217302963));
#58753=CARTESIAN_POINT('Ctrl Pts',(-50.,-10.7653981208323,-11.6258217302963));
#58754=CARTESIAN_POINT('Ctrl Pts',(-66.,-10.727207120633,-11.5281851158537));
#58755=CARTESIAN_POINT('Ctrl Pts',(-50.,-10.727207120633,-11.5281851158537));
#58756=CARTESIAN_POINT('Ctrl Pts',(-66.,-10.6876760500473,-11.4314236196986));
#58757=CARTESIAN_POINT('Ctrl Pts',(-50.,-10.6876760500473,-11.4314236196986));
#58758=CARTESIAN_POINT('Ctrl Pts',(-66.,-10.6468254580846,-11.3355369696227));
#58759=CARTESIAN_POINT('Ctrl Pts',(-50.,-10.6468254580846,-11.3355369696227));
#58760=CARTESIAN_POINT('Ctrl Pts',(-66.,-10.6045453214218,-11.2406410963124));
#58761=CARTESIAN_POINT('Ctrl Pts',(-50.,-10.6045453214218,-11.2406410963124));
#58762=CARTESIAN_POINT('Ctrl Pts',(-66.,-10.5605176911805,-11.1470361863206));
#58763=CARTESIAN_POINT('Ctrl Pts',(-50.,-10.5605176911805,-11.1470361863206));
#58764=CARTESIAN_POINT('Ctrl Pts',(-66.,-10.5142838856252,-11.055148542648));
#58765=CARTESIAN_POINT('Ctrl Pts',(-50.,-10.5142838856252,-11.055148542648));
#58766=CARTESIAN_POINT('Ctrl Pts',(-66.,-10.4653605771075,-10.9654297310826));
#58767=CARTESIAN_POINT('Ctrl Pts',(-50.,-10.4653605771075,-10.9654297310826));
#58768=CARTESIAN_POINT('Ctrl Pts',(-66.,-10.4133439014856,-10.8782663225706));
#58769=CARTESIAN_POINT('Ctrl Pts',(-50.,-10.4133439014856,-10.8782663225706));
#58770=CARTESIAN_POINT('Ctrl Pts',(-66.,-10.3580097561152,-10.7938927550471));
#58771=CARTESIAN_POINT('Ctrl Pts',(-50.,-10.3580097561152,-10.7938927550471));
#58772=CARTESIAN_POINT('Ctrl Pts',(-66.,-10.2994412084092,-10.7122811666816));
#58773=CARTESIAN_POINT('Ctrl Pts',(-50.,-10.2994412084092,-10.7122811666816));
#58774=CARTESIAN_POINT('Ctrl Pts',(-66.,-10.2379686981643,-10.6331907581101));
#58775=CARTESIAN_POINT('Ctrl Pts',(-50.,-10.2379686981643,-10.6331907581101));
#58776=CARTESIAN_POINT('Ctrl Pts',(-66.,-10.1740622242879,-10.5562581065423));
#58777=CARTESIAN_POINT('Ctrl Pts',(-50.,-10.1740622242879,-10.5562581065423));
#58778=CARTESIAN_POINT('Ctrl Pts',(-66.,-10.108239546518,-10.4810737531071));
#58779=CARTESIAN_POINT('Ctrl Pts',(-50.,-10.108239546518,-10.4810737531071));
#58780=CARTESIAN_POINT('Ctrl Pts',(-66.,-10.0409718699529,-10.4072610342189));
#58781=CARTESIAN_POINT('Ctrl Pts',(-50.,-10.0409718699529,-10.4072610342189));
#58782=CARTESIAN_POINT('Ctrl Pts',(-66.,-9.97258152483879,-10.3345613726147));
#58783=CARTESIAN_POINT('Ctrl Pts',(-50.,-9.97258152483879,-10.3345613726147));
#58784=CARTESIAN_POINT('Ctrl Pts',(-66.,-9.90326213654415,-10.2628187784479));
#58785=CARTESIAN_POINT('Ctrl Pts',(-50.,-9.90326213654415,-10.2628187784479));
#58786=CARTESIAN_POINT('Ctrl Pts',(-66.,-9.84714322904426,-10.2061255176443));
#58787=CARTESIAN_POINT('Ctrl Pts',(-50.,-9.84714322904426,-10.2061255176443));
#58788=CARTESIAN_POINT('Ctrl Pts',(-66.,-9.80469667097528,-10.163986719468));
#58789=CARTESIAN_POINT('Ctrl Pts',(-50.,-9.80469667097528,-10.163986719468));
#58790=CARTESIAN_POINT('Ctrl Pts',(-66.,-9.77624035711837,-10.1360633488319));
#58791=CARTESIAN_POINT('Ctrl Pts',(-50.,-9.77624035711837,-10.1360633488319));
#58792=CARTESIAN_POINT('Ctrl Pts',(-66.,-9.76197254719672,-10.1221439546065));
#58793=CARTESIAN_POINT('Ctrl Pts',(-50.,-9.76197254719672,-10.1221439546065));
#58794=CARTESIAN_POINT('Origin',(-65.75,0.,0.));
#58795=CARTESIAN_POINT('',(-65.5,-13.8963484576857,-9.57377274341605));
#58796=CARTESIAN_POINT('Origin',(-65.5,0.,0.));
#58797=CARTESIAN_POINT('Ctrl Pts',(-65.5,-13.8963484576857,-9.57377274341605));
#58798=CARTESIAN_POINT('Ctrl Pts',(-65.6931595476708,-13.7992573634772,
-9.37423221316899));
#58799=CARTESIAN_POINT('Ctrl Pts',(-65.8611256967054,-13.7088061439983,
-9.2076824840282));
#58800=CARTESIAN_POINT('Ctrl Pts',(-66.,-13.631341547005,-9.07343113870903));
#58801=CARTESIAN_POINT('Origin',(-58.,0.,0.));
#58802=CARTESIAN_POINT('',(-50.5,-13.8963484576857,-9.57377274341605));
#58803=CARTESIAN_POINT('Origin',(-50.5,0.,0.));
#58804=CARTESIAN_POINT('Ctrl Pts',(-50.5,-13.8963484576857,-9.57377274341605));
#58805=CARTESIAN_POINT('Ctrl Pts',(-55.5,-13.8963484576857,-9.57377274341605));
#58806=CARTESIAN_POINT('Ctrl Pts',(-60.5,-13.8963484576857,-9.57377274341605));
#58807=CARTESIAN_POINT('Ctrl Pts',(-65.5,-13.8963484576857,-9.57377274341605));
#58808=CARTESIAN_POINT('Origin',(-50.25,0.,0.));
#58809=CARTESIAN_POINT('Ctrl Pts',(-50.,-13.631341547005,-9.07343113870903));
#58810=CARTESIAN_POINT('Ctrl Pts',(-50.1388743032954,-13.7088061439988,
-9.20768248402894));
#58811=CARTESIAN_POINT('Ctrl Pts',(-50.3068404523299,-13.7992573634776,
-9.37423221316971));
#58812=CARTESIAN_POINT('Ctrl Pts',(-50.5,-13.8963484576857,-9.57377274341605));
#58813=CARTESIAN_POINT('Ctrl Pts',(-66.,-12.6433463826116,-6.1562731014228));
#58814=CARTESIAN_POINT('Ctrl Pts',(-50.,-12.6433463826116,-6.1562731014228));
#58815=CARTESIAN_POINT('Ctrl Pts',(-66.,-12.6639216231176,-6.16735975564195));
#58816=CARTESIAN_POINT('Ctrl Pts',(-50.,-12.6639216231176,-6.16735975564195));
#58817=CARTESIAN_POINT('Ctrl Pts',(-66.,-12.7051868090144,-6.18933938815496));
#58818=CARTESIAN_POINT('Ctrl Pts',(-50.,-12.7051868090144,-6.18933938815496));
#58819=CARTESIAN_POINT('Ctrl Pts',(-66.,-12.7674287029928,-6.22172782249946));
#58820=CARTESIAN_POINT('Ctrl Pts',(-50.,-12.7674287029928,-6.22172782249946));
#58821=CARTESIAN_POINT('Ctrl Pts',(-66.,-12.851107036246,-6.26374871229064));
#58822=CARTESIAN_POINT('Ctrl Pts',(-50.,-12.851107036246,-6.26374871229064));
#58823=CARTESIAN_POINT('Ctrl Pts',(-66.,-12.9568646849259,-6.31427939831312));
#58824=CARTESIAN_POINT('Ctrl Pts',(-50.,-12.9568646849259,-6.31427939831312));
#58825=CARTESIAN_POINT('Ctrl Pts',(-66.,-13.0638062493037,-6.3626601011734));
#58826=CARTESIAN_POINT('Ctrl Pts',(-50.,-13.0638062493037,-6.3626601011734));
#58827=CARTESIAN_POINT('Ctrl Pts',(-66.,-13.1719732880642,-6.40859684907992));
#58828=CARTESIAN_POINT('Ctrl Pts',(-50.,-13.1719732880642,-6.40859684907992));
#58829=CARTESIAN_POINT('Ctrl Pts',(-66.,-13.281428281035,-6.45159976453225));
#58830=CARTESIAN_POINT('Ctrl Pts',(-50.,-13.281428281035,-6.45159976453225));
#58831=CARTESIAN_POINT('Ctrl Pts',(-66.,-13.3922710176287,-6.49104836068956));
#58832=CARTESIAN_POINT('Ctrl Pts',(-50.,-13.3922710176287,-6.49104836068956));
#58833=CARTESIAN_POINT('Ctrl Pts',(-66.,-13.5046637960973,-6.52627657330457));
#58834=CARTESIAN_POINT('Ctrl Pts',(-50.,-13.5046637960973,-6.52627657330457));
#58835=CARTESIAN_POINT('Ctrl Pts',(-66.,-13.6188417913781,-6.55665495690443));
#58836=CARTESIAN_POINT('Ctrl Pts',(-50.,-13.6188417913781,-6.55665495690443));
#58837=CARTESIAN_POINT('Ctrl Pts',(-66.,-13.7351593700424,-6.58166436202222));
#58838=CARTESIAN_POINT('Ctrl Pts',(-50.,-13.7351593700424,-6.58166436202222));
#58839=CARTESIAN_POINT('Ctrl Pts',(-66.,-13.8539565214648,-6.60104137487127));
#58840=CARTESIAN_POINT('Ctrl Pts',(-50.,-13.8539565214648,-6.60104137487127));
#58841=CARTESIAN_POINT('Ctrl Pts',(-66.,-13.9753080627051,-6.61499785909296));
#58842=CARTESIAN_POINT('Ctrl Pts',(-50.,-13.9753080627051,-6.61499785909296));
#58843=CARTESIAN_POINT('Ctrl Pts',(-66.,-14.0988589764351,-6.62435775818486));
#58844=CARTESIAN_POINT('Ctrl Pts',(-50.,-14.0988589764351,-6.62435775818486));
#58845=CARTESIAN_POINT('Ctrl Pts',(-66.,-14.2235033417215,-6.63087754928856));
#58846=CARTESIAN_POINT('Ctrl Pts',(-50.,-14.2235033417215,-6.63087754928856));
#58847=CARTESIAN_POINT('Ctrl Pts',(-66.,-14.3475726821666,-6.63694296762358));
#58848=CARTESIAN_POINT('Ctrl Pts',(-50.,-14.3475726821666,-6.63694296762358));
#58849=CARTESIAN_POINT('Ctrl Pts',(-66.,-14.4696861744433,-6.64444024204806));
#58850=CARTESIAN_POINT('Ctrl Pts',(-50.,-14.4696861744433,-6.64444024204806));
#58851=CARTESIAN_POINT('Ctrl Pts',(-66.,-14.5893646306071,-6.65393139885702));
#58852=CARTESIAN_POINT('Ctrl Pts',(-50.,-14.5893646306071,-6.65393139885702));
#58853=CARTESIAN_POINT('Ctrl Pts',(-66.,-14.7078951610787,-6.6634907630476));
#58854=CARTESIAN_POINT('Ctrl Pts',(-50.,-14.7078951610787,-6.6634907630476));
#58855=CARTESIAN_POINT('Ctrl Pts',(-66.,-14.8286466959702,-6.66830024039538));
#58856=CARTESIAN_POINT('Ctrl Pts',(-50.,-14.8286466959702,-6.66830024039538));
#58857=CARTESIAN_POINT('Ctrl Pts',(-66.,-14.9551891629322,-6.66329671103626));
#58858=CARTESIAN_POINT('Ctrl Pts',(-50.,-14.9551891629322,-6.66329671103626));
#58859=CARTESIAN_POINT('Ctrl Pts',(-66.,-15.0896875773,-6.64543810943336));
#58860=CARTESIAN_POINT('Ctrl Pts',(-50.,-15.0896875773,-6.64543810943336));
#58861=CARTESIAN_POINT('Ctrl Pts',(-66.,-15.2312621759268,-6.61601501775332));
#58862=CARTESIAN_POINT('Ctrl Pts',(-50.,-15.2312621759268,-6.61601501775332));
#58863=CARTESIAN_POINT('Ctrl Pts',(-66.,-15.3741384264112,-6.58326088854155));
#58864=CARTESIAN_POINT('Ctrl Pts',(-50.,-15.3741384264112,-6.58326088854155));
#58865=CARTESIAN_POINT('Ctrl Pts',(-66.,-15.5090614410165,-6.56034427212951));
#58866=CARTESIAN_POINT('Ctrl Pts',(-50.,-15.5090614410165,-6.56034427212951));
#58867=CARTESIAN_POINT('Ctrl Pts',(-66.,-15.6250970135137,-6.56281431696235));
#58868=CARTESIAN_POINT('Ctrl Pts',(-50.,-15.6250970135137,-6.56281431696235));
#58869=CARTESIAN_POINT('Ctrl Pts',(-66.,-15.7111627073129,-6.60642866537431));
#58870=CARTESIAN_POINT('Ctrl Pts',(-50.,-15.7111627073129,-6.60642866537431));
#58871=CARTESIAN_POINT('Ctrl Pts',(-66.,-15.7579605986384,-6.70441211879867));
#58872=CARTESIAN_POINT('Ctrl Pts',(-50.,-15.7579605986384,-6.70441211879867));
#58873=CARTESIAN_POINT('Ctrl Pts',(-66.,-15.7584967454601,-6.86671937924014));
#58874=CARTESIAN_POINT('Ctrl Pts',(-50.,-15.7584967454601,-6.86671937924014));
#58875=CARTESIAN_POINT('Ctrl Pts',(-66.,-15.7075631420906,-7.10076915669713));
#58876=CARTESIAN_POINT('Ctrl Pts',(-50.,-15.7075631420906,-7.10076915669713));
#58877=CARTESIAN_POINT('Ctrl Pts',(-66.,-15.6015340605988,-7.41173254135438));
#58878=CARTESIAN_POINT('Ctrl Pts',(-50.,-15.6015340605988,-7.41173254135438));
#58879=CARTESIAN_POINT('Ctrl Pts',(-66.,-15.438048141096,-7.80298348305155));
#58880=CARTESIAN_POINT('Ctrl Pts',(-50.,-15.438048141096,-7.80298348305155));
#58881=CARTESIAN_POINT('Ctrl Pts',(-66.,-15.2157536026519,-8.27645984483354));
#58882=CARTESIAN_POINT('Ctrl Pts',(-50.,-15.2157536026519,-8.27645984483354));
#58883=CARTESIAN_POINT('Ctrl Pts',(-66.,-14.9340392129229,-8.83304473364892));
#58884=CARTESIAN_POINT('Ctrl Pts',(-50.,-14.9340392129229,-8.83304473364892));
#58885=CARTESIAN_POINT('Ctrl Pts',(-66.,-14.6610342795723,-9.34494709460039));
#58886=CARTESIAN_POINT('Ctrl Pts',(-50.,-14.6610342795723,-9.34494709460039));
#58887=CARTESIAN_POINT('Ctrl Pts',(-66.,-14.4295401925849,-9.76628311391338));
#58888=CARTESIAN_POINT('Ctrl Pts',(-50.,-14.4295401925849,-9.76628311391338));
#58889=CARTESIAN_POINT('Ctrl Pts',(-66.,-14.2633419918951,-10.0637780121554));
#58890=CARTESIAN_POINT('Ctrl Pts',(-50.,-14.2633419918951,-10.0637780121554));
#58891=CARTESIAN_POINT('Ctrl Pts',(-66.,-14.1772756878995,-10.2166765177964));
#58892=CARTESIAN_POINT('Ctrl Pts',(-50.,-14.1772756878995,-10.2166765177964));
#58893=CARTESIAN_POINT('',(-65.5,-15.5455251229224,-6.56523218573333));
#58894=CARTESIAN_POINT('Ctrl Pts',(-66.,-14.9594853178907,-6.65991171291435));
#58895=CARTESIAN_POINT('Ctrl Pts',(-65.7933280154027,-15.195120245778,-6.63878177870532));
#58896=CARTESIAN_POINT('Ctrl Pts',(-65.6370761749496,-15.3970618191913,
-6.56443702203716));
#58897=CARTESIAN_POINT('Ctrl Pts',(-65.5,-15.5455251229224,-6.56523218573333));
#58898=CARTESIAN_POINT('',(-66.,-12.6433463826116,-6.1562731014228));
#58899=CARTESIAN_POINT('',(-50.5,-15.5455251229224,-6.56523218573333));
#58900=CARTESIAN_POINT('Ctrl Pts',(-50.5,-15.5455251229224,-6.56523218573333));
#58901=CARTESIAN_POINT('Ctrl Pts',(-50.4518618349121,-15.4933880463872,
-6.56495294157371));
#58902=CARTESIAN_POINT('Ctrl Pts',(-50.4012423593883,-15.4346954562179,
-6.57371248407322));
#58903=CARTESIAN_POINT('Ctrl Pts',(-50.24411297938,-15.248416451548,-6.60952476775937));
#58904=CARTESIAN_POINT('Ctrl Pts',(-50.1366827452942,-15.1153227377209,
-6.64593740758603));
#58905=CARTESIAN_POINT('Ctrl Pts',(-50.,-14.9594853178907,-6.65991171291435));
#58906=CARTESIAN_POINT('Ctrl Pts',(-65.5,-15.5455251229224,-6.56523218573333));
#58907=CARTESIAN_POINT('Ctrl Pts',(-60.5,-15.5455251229224,-6.56523218573333));
#58908=CARTESIAN_POINT('Ctrl Pts',(-55.5,-15.5455251229224,-6.56523218573333));
#58909=CARTESIAN_POINT('Ctrl Pts',(-50.5,-15.5455251229224,-6.56523218573333));
#58910=CARTESIAN_POINT('Origin',(-66.,0.,0.));
#58911=CARTESIAN_POINT('',(-66.,-11.9725570665522,-7.37643433768308));
#58912=CARTESIAN_POINT('Ctrl Pts',(-66.,-14.1772756878995,-10.2166765177964));
#58913=CARTESIAN_POINT('Ctrl Pts',(-50.,-14.1772756878995,-10.2166765177964));
#58914=CARTESIAN_POINT('Ctrl Pts',(-66.,-14.169090684931,-10.1957080532821));
#58915=CARTESIAN_POINT('Ctrl Pts',(-50.,-14.169090684931,-10.1957080532821));
#58916=CARTESIAN_POINT('Ctrl Pts',(-66.,-14.1526091283973,-10.1538681781678));
#58917=CARTESIAN_POINT('Ctrl Pts',(-50.,-14.1526091283973,-10.1538681781678));
#58918=CARTESIAN_POINT('Ctrl Pts',(-66.,-14.1275521422774,-10.0913995267525));
#58919=CARTESIAN_POINT('Ctrl Pts',(-50.,-14.1275521422774,-10.0913995267525));
#58920=CARTESIAN_POINT('Ctrl Pts',(-66.,-14.0934726306568,-10.008691092668));
#58921=CARTESIAN_POINT('Ctrl Pts',(-50.,-14.0934726306568,-10.008691092668));
#58922=CARTESIAN_POINT('Ctrl Pts',(-66.,-14.0497518771326,-9.9062815985322));
#58923=CARTESIAN_POINT('Ctrl Pts',(-50.,-14.0497518771326,-9.9062815985322));
#58924=CARTESIAN_POINT('Ctrl Pts',(-66.,-14.0049055762784,-9.80485304191326));
#58925=CARTESIAN_POINT('Ctrl Pts',(-50.,-14.0049055762784,-9.80485304191326));
#58926=CARTESIAN_POINT('Ctrl Pts',(-66.,-13.9589323331141,-9.70440911809916));
#58927=CARTESIAN_POINT('Ctrl Pts',(-50.,-13.9589323331141,-9.70440911809916));
#58928=CARTESIAN_POINT('Ctrl Pts',(-66.,-13.9118358290362,-9.60495081840769));
#58929=CARTESIAN_POINT('Ctrl Pts',(-50.,-13.9118358290362,-9.60495081840769));
#58930=CARTESIAN_POINT('Ctrl Pts',(-66.,-13.8636282964938,-9.50647368802256));
#58931=CARTESIAN_POINT('Ctrl Pts',(-50.,-13.8636282964938,-9.50647368802256));
#58932=CARTESIAN_POINT('Ctrl Pts',(-66.,-13.8143244129603,-9.40897518514854));
#58933=CARTESIAN_POINT('Ctrl Pts',(-50.,-13.8143244129603,-9.40897518514854));
#58934=CARTESIAN_POINT('Ctrl Pts',(-66.,-13.7639341278636,-9.31246310590722));
#58935=CARTESIAN_POINT('Ctrl Pts',(-50.,-13.7639341278636,-9.31246310590722));
#58936=CARTESIAN_POINT('Ctrl Pts',(-66.,-13.7124554531318,-9.21696428016702));
#58937=CARTESIAN_POINT('Ctrl Pts',(-50.,-13.7124554531318,-9.21696428016702));
#58938=CARTESIAN_POINT('Ctrl Pts',(-66.,-13.6598685224049,-9.12253151471647));
#58939=CARTESIAN_POINT('Ctrl Pts',(-50.,-13.6598685224049,-9.12253151471647));
#58940=CARTESIAN_POINT('Ctrl Pts',(-66.,-13.606126110027,-9.02925545685226));
#58941=CARTESIAN_POINT('Ctrl Pts',(-50.,-13.606126110027,-9.02925545685226));
#58942=CARTESIAN_POINT('Ctrl Pts',(-66.,-13.5511663152664,-8.93724619299147));
#58943=CARTESIAN_POINT('Ctrl Pts',(-50.,-13.5511663152664,-8.93724619299147));
#58944=CARTESIAN_POINT('Ctrl Pts',(-66.,-13.4949307609898,-8.84660742136017));
#58945=CARTESIAN_POINT('Ctrl Pts',(-50.,-13.4949307609898,-8.84660742136017));
#58946=CARTESIAN_POINT('Ctrl Pts',(-66.,-13.4373825330349,-8.7574108514811));
#58947=CARTESIAN_POINT('Ctrl Pts',(-50.,-13.4373825330349,-8.7574108514811));
#58948=CARTESIAN_POINT('Ctrl Pts',(-66.,-13.3785211625712,-8.66967501744431));
#58949=CARTESIAN_POINT('Ctrl Pts',(-50.,-13.3785211625712,-8.66967501744431));
#58950=CARTESIAN_POINT('Ctrl Pts',(-66.,-13.3184076369901,-8.58332951829382));
#58951=CARTESIAN_POINT('Ctrl Pts',(-50.,-13.3184076369901,-8.58332951829382));
#58952=CARTESIAN_POINT('Ctrl Pts',(-66.,-13.2571352386615,-8.49825805316535));
#58953=CARTESIAN_POINT('Ctrl Pts',(-50.,-13.2571352386615,-8.49825805316535));
#58954=CARTESIAN_POINT('Ctrl Pts',(-66.,-13.1947825037901,-8.41436747482742));
#58955=CARTESIAN_POINT('Ctrl Pts',(-50.,-13.1947825037901,-8.41436747482742));
#58956=CARTESIAN_POINT('Ctrl Pts',(-66.,-13.1313692681049,-8.3316524092927));
#58957=CARTESIAN_POINT('Ctrl Pts',(-50.,-13.1313692681049,-8.3316524092927));
#58958=CARTESIAN_POINT('Ctrl Pts',(-66.,-13.0668177956572,-8.25025250675973));
#58959=CARTESIAN_POINT('Ctrl Pts',(-50.,-13.0668177956572,-8.25025250675973));
#58960=CARTESIAN_POINT('Ctrl Pts',(-66.,-13.0008947798771,-8.17053759353955));
#58961=CARTESIAN_POINT('Ctrl Pts',(-50.,-13.0008947798771,-8.17053759353955));
#58962=CARTESIAN_POINT('Ctrl Pts',(-66.,-12.9332619666045,-8.09303464904925));
#58963=CARTESIAN_POINT('Ctrl Pts',(-50.,-12.9332619666045,-8.09303464904925));
#58964=CARTESIAN_POINT('Ctrl Pts',(-66.,-12.8635635126628,-8.01830125100551));
#58965=CARTESIAN_POINT('Ctrl Pts',(-50.,-12.8635635126628,-8.01830125100551));
#58966=CARTESIAN_POINT('Ctrl Pts',(-66.,-12.7915043783298,-7.9468122624453));
#58967=CARTESIAN_POINT('Ctrl Pts',(-50.,-12.7915043783298,-7.9468122624453));
#58968=CARTESIAN_POINT('Ctrl Pts',(-66.,-12.7169258039014,-7.87885048806616));
#58969=CARTESIAN_POINT('Ctrl Pts',(-50.,-12.7169258039014,-7.87885048806616));
#58970=CARTESIAN_POINT('Ctrl Pts',(-66.,-12.6399013181197,-7.81436828334278));
#58971=CARTESIAN_POINT('Ctrl Pts',(-50.,-12.6399013181197,-7.81436828334278));
#58972=CARTESIAN_POINT('Ctrl Pts',(-66.,-12.5606910950408,-7.75305023703025));
#58973=CARTESIAN_POINT('Ctrl Pts',(-50.,-12.5606910950408,-7.75305023703025));
#58974=CARTESIAN_POINT('Ctrl Pts',(-66.,-12.4796599881192,-7.69442745995809));
#58975=CARTESIAN_POINT('Ctrl Pts',(-50.,-12.4796599881192,-7.69442745995809));
#58976=CARTESIAN_POINT('Ctrl Pts',(-66.,-12.3972076624386,-7.63797459554787));
#58977=CARTESIAN_POINT('Ctrl Pts',(-50.,-12.3972076624386,-7.63797459554787));
#58978=CARTESIAN_POINT('Ctrl Pts',(-66.,-12.3136968468978,-7.58320962985052));
#58979=CARTESIAN_POINT('Ctrl Pts',(-50.,-12.3136968468978,-7.58320962985052));
#58980=CARTESIAN_POINT('Ctrl Pts',(-66.,-12.2293754395952,-7.5298019490105));
#58981=CARTESIAN_POINT('Ctrl Pts',(-50.,-12.2293754395952,-7.5298019490105));
#58982=CARTESIAN_POINT('Ctrl Pts',(-66.,-12.144392189705,-7.47755231121817));
#58983=CARTESIAN_POINT('Ctrl Pts',(-50.,-12.144392189705,-7.47755231121817));
#58984=CARTESIAN_POINT('Ctrl Pts',(-66.,-12.0759373202474,-7.43659637822836));
#58985=CARTESIAN_POINT('Ctrl Pts',(-50.,-12.0759373202474,-7.43659637822836));
#58986=CARTESIAN_POINT('Ctrl Pts',(-66.,-12.0243448058902,-7.40633747762124));
#58987=CARTESIAN_POINT('Ctrl Pts',(-50.,-12.0243448058902,-7.40633747762124));
#58988=CARTESIAN_POINT('Ctrl Pts',(-66.,-11.9898382395678,-7.38636816850343));
#58989=CARTESIAN_POINT('Ctrl Pts',(-50.,-11.9898382395678,-7.38636816850343));
#58990=CARTESIAN_POINT('Ctrl Pts',(-66.,-11.9725570665522,-7.37643433768309));
#58991=CARTESIAN_POINT('Ctrl Pts',(-50.,-11.9725570665522,-7.37643433768309));
#58992=CARTESIAN_POINT('Origin',(-65.75,0.,0.));
#58993=CARTESIAN_POINT('',(-65.5,-15.8406695805923,-5.81711373779967));
#58994=CARTESIAN_POINT('Origin',(-65.5,0.,0.));
#58995=CARTESIAN_POINT('Ctrl Pts',(-65.5,-15.8406695805923,-5.81711373779968));
#58996=CARTESIAN_POINT('Ctrl Pts',(-65.6931595476752,-15.6970050696912,
-5.64798771349928));
#58997=CARTESIAN_POINT('Ctrl Pts',(-65.8611256967103,-15.5679763082525,
-5.509164753929));
#58998=CARTESIAN_POINT('Ctrl Pts',(-66.,-15.4595584521058,-5.39839582338346));
#58999=CARTESIAN_POINT('Origin',(-58.,0.,0.));
#59000=CARTESIAN_POINT('',(-50.5,-15.8406695805923,-5.81711373779967));
#59001=CARTESIAN_POINT('Origin',(-50.5,0.,0.));
#59002=CARTESIAN_POINT('Ctrl Pts',(-50.5,-15.8406695805923,-5.81711373779967));
#59003=CARTESIAN_POINT('Ctrl Pts',(-55.5,-15.8406695805923,-5.81711373779967));
#59004=CARTESIAN_POINT('Ctrl Pts',(-60.5,-15.8406695805923,-5.81711373779967));
#59005=CARTESIAN_POINT('Ctrl Pts',(-65.5,-15.8406695805923,-5.81711373779967));
#59006=CARTESIAN_POINT('Origin',(-50.25,0.,0.));
#59007=CARTESIAN_POINT('Ctrl Pts',(-50.,-15.4595584521058,-5.39839582338346));
#59008=CARTESIAN_POINT('Ctrl Pts',(-50.1388743032875,-15.5679763082507,
-5.50916475392723));
#59009=CARTESIAN_POINT('Ctrl Pts',(-50.3068404523245,-15.697005069691,-5.64798771349904));
#59010=CARTESIAN_POINT('Ctrl Pts',(-50.5,-15.8406695805923,-5.81711373779967));
#59011=CARTESIAN_POINT('Ctrl Pts',(-66.,-13.7771352694631,-2.8185900760694));
#59012=CARTESIAN_POINT('Ctrl Pts',(-50.,-13.7771352694631,-2.8185900760694));
#59013=CARTESIAN_POINT('Ctrl Pts',(-66.,-13.7998212397401,-2.82421156841951));
#59014=CARTESIAN_POINT('Ctrl Pts',(-50.,-13.7998212397401,-2.82421156841951));
#59015=CARTESIAN_POINT('Ctrl Pts',(-66.,-13.8452561162702,-2.83523843593487));
#59016=CARTESIAN_POINT('Ctrl Pts',(-50.,-13.8452561162702,-2.83523843593487));
#59017=CARTESIAN_POINT('Ctrl Pts',(-66.,-13.913597242777,-2.85113039846586));
#59018=CARTESIAN_POINT('Ctrl Pts',(-50.,-13.913597242777,-2.85113039846586));
#59019=CARTESIAN_POINT('Ctrl Pts',(-66.,-14.0050968376581,-2.87102116947837));
#59020=CARTESIAN_POINT('Ctrl Pts',(-50.,-14.0050968376581,-2.87102116947837));
#59021=CARTESIAN_POINT('Ctrl Pts',(-66.,-14.1200983859353,-2.89366348336299));
#59022=CARTESIAN_POINT('Ctrl Pts',(-50.,-14.1200983859353,-2.89366348336299));
#59023=CARTESIAN_POINT('Ctrl Pts',(-66.,-14.2357119759516,-2.91392893189869));
#59024=CARTESIAN_POINT('Ctrl Pts',(-50.,-14.2357119759516,-2.91392893189869));
#59025=CARTESIAN_POINT('Ctrl Pts',(-66.,-14.3519047529378,-2.93152244373364));
#59026=CARTESIAN_POINT('Ctrl Pts',(-50.,-14.3519047529378,-2.93152244373364));
#59027=CARTESIAN_POINT('Ctrl Pts',(-66.,-14.4686154062224,-2.94595399366867));
#59028=CARTESIAN_POINT('Ctrl Pts',(-50.,-14.4686154062224,-2.94595399366867));
#59029=CARTESIAN_POINT('Ctrl Pts',(-66.,-14.5857862813476,-2.95659777198027));
#59030=CARTESIAN_POINT('Ctrl Pts',(-50.,-14.5857862813476,-2.95659777198027));
#59031=CARTESIAN_POINT('Ctrl Pts',(-66.,-14.703408934225,-2.96276827812033));
#59032=CARTESIAN_POINT('Ctrl Pts',(-50.,-14.703408934225,-2.96276827812033));
#59033=CARTESIAN_POINT('Ctrl Pts',(-66.,-14.8215546146151,-2.96379735617437));
#59034=CARTESIAN_POINT('Ctrl Pts',(-50.,-14.8215546146151,-2.96379735617437));
#59035=CARTESIAN_POINT('Ctrl Pts',(-66.,-14.9404374487894,-2.959094039328));
#59036=CARTESIAN_POINT('Ctrl Pts',(-50.,-14.9404374487894,-2.959094039328));
#59037=CARTESIAN_POINT('Ctrl Pts',(-66.,-15.0603212363863,-2.9483186375038));
#59038=CARTESIAN_POINT('Ctrl Pts',(-50.,-15.0603212363863,-2.9483186375038));
#59039=CARTESIAN_POINT('Ctrl Pts',(-66.,-15.181331132295,-2.93165775201116));
#59040=CARTESIAN_POINT('Ctrl Pts',(-50.,-15.181331132295,-2.93165775201116));
#59041=CARTESIAN_POINT('Ctrl Pts',(-66.,-15.3033281791249,-2.90999772986683));
#59042=CARTESIAN_POINT('Ctrl Pts',(-50.,-15.3033281791249,-2.90999772986683));
#59043=CARTESIAN_POINT('Ctrl Pts',(-66.,-15.4256780185848,-2.88531489660512));
#59044=CARTESIAN_POINT('Ctrl Pts',(-50.,-15.4256780185848,-2.88531489660512));
#59045=CARTESIAN_POINT('Ctrl Pts',(-66.,-15.5473579007536,-2.86033496839371));
#59046=CARTESIAN_POINT('Ctrl Pts',(-50.,-15.5473579007536,-2.86033496839371));
#59047=CARTESIAN_POINT('Ctrl Pts',(-66.,-15.6674994694501,-2.83722831154002));
#59048=CARTESIAN_POINT('Ctrl Pts',(-50.,-15.6674994694501,-2.83722831154002));
#59049=CARTESIAN_POINT('Ctrl Pts',(-66.,-15.7857783615561,-2.81665846444538));
#59050=CARTESIAN_POINT('Ctrl Pts',(-50.,-15.7857783615561,-2.81665846444538));
#59051=CARTESIAN_POINT('Ctrl Pts',(-66.,-15.9029623546524,-2.7964401593829));
#59052=CARTESIAN_POINT('Ctrl Pts',(-50.,-15.9029623546524,-2.7964401593829));
#59053=CARTESIAN_POINT('Ctrl Pts',(-66.,-16.0211163264077,-2.77106885256863));
#59054=CARTESIAN_POINT('Ctrl Pts',(-50.,-16.0211163264077,-2.77106885256863));
#59055=CARTESIAN_POINT('Ctrl Pts',(-66.,-16.1424389019231,-2.73475268645485));
#59056=CARTESIAN_POINT('Ctrl Pts',(-50.,-16.1424389019231,-2.73475268645485));
#59057=CARTESIAN_POINT('Ctrl Pts',(-66.,-16.2682705476607,-2.68400675016798));
#59058=CARTESIAN_POINT('Ctrl Pts',(-50.,-16.2682705476607,-2.68400675016798));
#59059=CARTESIAN_POINT('Ctrl Pts',(-66.,-16.3980800945842,-2.62029986806045));
#59060=CARTESIAN_POINT('Ctrl Pts',(-50.,-16.3980800945842,-2.62029986806045));
#59061=CARTESIAN_POINT('Ctrl Pts',(-66.,-16.5283220042307,-2.55304289143699));
#59062=CARTESIAN_POINT('Ctrl Pts',(-50.,-16.5283220042307,-2.55304289143699));
#59063=CARTESIAN_POINT('Ctrl Pts',(-66.,-16.6533070334764,-2.49729225339212));
#59064=CARTESIAN_POINT('Ctrl Pts',(-50.,-16.6533070334764,-2.49729225339212));
#59065=CARTESIAN_POINT('Ctrl Pts',(-66.,-16.7663114102599,-2.470827823793));
#59066=CARTESIAN_POINT('Ctrl Pts',(-50.,-16.7663114102599,-2.470827823793));
#59067=CARTESIAN_POINT('Ctrl Pts',(-66.,-16.86051963941,-2.49166827956873));
#59068=CARTESIAN_POINT('Ctrl Pts',(-50.,-16.86051963941,-2.49166827956873));
#59069=CARTESIAN_POINT('Ctrl Pts',(-66.,-16.9302147829003,-2.57493524031151));
#59070=CARTESIAN_POINT('Ctrl Pts',(-50.,-16.9302147829003,-2.57493524031151));
#59071=CARTESIAN_POINT('Ctrl Pts',(-66.,-16.971098259969,-2.73200998541143));
#59072=CARTESIAN_POINT('Ctrl Pts',(-50.,-16.971098259969,-2.73200998541143));
#59073=CARTESIAN_POINT('Ctrl Pts',(-66.,-16.9799706421563,-2.97137333079705));
#59074=CARTESIAN_POINT('Ctrl Pts',(-50.,-16.9799706421563,-2.97137333079705));
#59075=CARTESIAN_POINT('Ctrl Pts',(-66.,-16.9546061082763,-3.29893558921601));
#59076=CARTESIAN_POINT('Ctrl Pts',(-50.,-16.9546061082763,-3.29893558921601));
#59077=CARTESIAN_POINT('Ctrl Pts',(-66.,-16.8935565521081,-3.71855195799381));
#59078=CARTESIAN_POINT('Ctrl Pts',(-50.,-16.8935565521081,-3.71855195799381));
#59079=CARTESIAN_POINT('Ctrl Pts',(-66.,-16.795994588347,-4.23243559289131));
#59080=CARTESIAN_POINT('Ctrl Pts',(-50.,-16.795994588347,-4.23243559289131));
#59081=CARTESIAN_POINT('Ctrl Pts',(-66.,-16.6615478074051,-4.84159386373095));
#59082=CARTESIAN_POINT('Ctrl Pts',(-50.,-16.6615478074051,-4.84159386373095));
#59083=CARTESIAN_POINT('Ctrl Pts',(-66.,-16.5244247664411,-5.40530743676095));
#59084=CARTESIAN_POINT('Ctrl Pts',(-50.,-16.5244247664411,-5.40530743676095));
#59085=CARTESIAN_POINT('Ctrl Pts',(-66.,-16.4049854989856,-5.87097664861672));
#59086=CARTESIAN_POINT('Ctrl Pts',(-50.,-16.4049854989856,-5.87097664861672));
#59087=CARTESIAN_POINT('Ctrl Pts',(-66.,-16.3179926930635,-6.20045700935217));
#59088=CARTESIAN_POINT('Ctrl Pts',(-50.,-16.3179926930635,-6.20045700935217));
#59089=CARTESIAN_POINT('Ctrl Pts',(-66.,-16.2726546323884,-6.36995574670713));
#59090=CARTESIAN_POINT('Ctrl Pts',(-50.,-16.2726546323884,-6.36995574670713));
#59091=CARTESIAN_POINT('',(-65.5,-16.6898407164458,-2.49295845526303));
#59092=CARTESIAN_POINT('Ctrl Pts',(-66.,-16.1457582704724,-2.73040562398164));
#59093=CARTESIAN_POINT('Ctrl Pts',(-65.7933280154031,-16.3687354928431,
-2.65133950188281));
#59094=CARTESIAN_POINT('Ctrl Pts',(-65.6370761749492,-16.5458439112369,
-2.5291095953495));
#59095=CARTESIAN_POINT('Ctrl Pts',(-65.5,-16.6898407164458,-2.49295845526303));
#59096=CARTESIAN_POINT('',(-66.,-13.7771352694631,-2.8185900760694));
#59097=CARTESIAN_POINT('',(-50.5,-16.6898407164458,-2.49295845526303));
#59098=CARTESIAN_POINT('Ctrl Pts',(-50.5,-16.6898407164458,-2.49295845526304));
#59099=CARTESIAN_POINT('Ctrl Pts',(-50.451861834912,-16.6392721768446,-2.50565394775287));
#59100=CARTESIAN_POINT('Ctrl Pts',(-50.401242359388,-16.5846019319592,-2.52873454674382));
#59101=CARTESIAN_POINT('Ctrl Pts',(-50.2441129793792,-16.4130813775527,
-2.6097474263366));
#59102=CARTESIAN_POINT('Ctrl Pts',(-50.1366827452938,-16.293224502778,-2.67811515679866));
#59103=CARTESIAN_POINT('Ctrl Pts',(-50.,-16.1457582704724,-2.73040562398164));
#59104=CARTESIAN_POINT('Ctrl Pts',(-65.5,-16.6898407164458,-2.49295845526303));
#59105=CARTESIAN_POINT('Ctrl Pts',(-60.5,-16.6898407164458,-2.49295845526303));
#59106=CARTESIAN_POINT('Ctrl Pts',(-55.5,-16.6898407164458,-2.49295845526303));
#59107=CARTESIAN_POINT('Ctrl Pts',(-50.5,-16.6898407164458,-2.49295845526303));
#59108=CARTESIAN_POINT('Origin',(-66.,0.,0.));
#59109=CARTESIAN_POINT('',(-66.,-13.4308617934315,-4.16723622269519));
#59110=CARTESIAN_POINT('Ctrl Pts',(-66.,-16.2726546323884,-6.36995574670713));
#59111=CARTESIAN_POINT('Ctrl Pts',(-50.,-16.2726546323884,-6.36995574670713));
#59112=CARTESIAN_POINT('Ctrl Pts',(-66.,-16.2595121312652,-6.35168157252855));
#59113=CARTESIAN_POINT('Ctrl Pts',(-50.,-16.2595121312652,-6.35168157252855));
#59114=CARTESIAN_POINT('Ctrl Pts',(-66.,-16.2331432193164,-6.31525497046376));
#59115=CARTESIAN_POINT('Ctrl Pts',(-50.,-16.2331432193164,-6.31525497046376));
#59116=CARTESIAN_POINT('Ctrl Pts',(-66.,-16.1933381226201,-6.26098030565532));
#59117=CARTESIAN_POINT('Ctrl Pts',(-50.,-16.1933381226201,-6.26098030565532));
#59118=CARTESIAN_POINT('Ctrl Pts',(-66.,-16.1397605303849,-6.18934553901729));
#59119=CARTESIAN_POINT('Ctrl Pts',(-50.,-16.1397605303849,-6.18934553901729));
#59120=CARTESIAN_POINT('Ctrl Pts',(-66.,-16.0719451391882,-6.1010263367184));
#59121=CARTESIAN_POINT('Ctrl Pts',(-50.,-16.0719451391882,-6.1010263367184));
#59122=CARTESIAN_POINT('Ctrl Pts',(-66.,-16.0032835110412,-6.01393716621888));
#59123=CARTESIAN_POINT('Ctrl Pts',(-50.,-16.0032835110412,-6.01393716621888));
#59124=CARTESIAN_POINT('Ctrl Pts',(-66.,-15.9337752137699,-5.92808195363001));
#59125=CARTESIAN_POINT('Ctrl Pts',(-50.,-15.9337752137699,-5.92808195363001));
#59126=CARTESIAN_POINT('Ctrl Pts',(-66.,-15.8634240596442,-5.84346074359936));
#59127=CARTESIAN_POINT('Ctrl Pts',(-50.,-15.8634240596442,-5.84346074359936));
#59128=CARTESIAN_POINT('Ctrl Pts',(-66.,-15.7922407889403,-5.76006617918052));
#59129=CARTESIAN_POINT('Ctrl Pts',(-50.,-15.7922407889403,-5.76006617918052));
#59130=CARTESIAN_POINT('Ctrl Pts',(-66.,-15.720238985893,-5.67789214829422));
#59131=CARTESIAN_POINT('Ctrl Pts',(-50.,-15.720238985893,-5.67789214829422));
#59132=CARTESIAN_POINT('Ctrl Pts',(-66.,-15.6474302261674,-5.59694372781046));
#59133=CARTESIAN_POINT('Ctrl Pts',(-50.,-15.6474302261674,-5.59694372781046));
#59134=CARTESIAN_POINT('Ctrl Pts',(-66.,-15.5738192564671,-5.5172473991014));
#59135=CARTESIAN_POINT('Ctrl Pts',(-50.,-15.5738192564671,-5.5172473991014));
#59136=CARTESIAN_POINT('Ctrl Pts',(-66.,-15.4993999670851,-5.43885925049602));
#59137=CARTESIAN_POINT('Ctrl Pts',(-50.,-15.4993999670851,-5.43885925049602));
#59138=CARTESIAN_POINT('Ctrl Pts',(-66.,-15.424149159112,-5.36187882598251));
#59139=CARTESIAN_POINT('Ctrl Pts',(-50.,-15.424149159112,-5.36187882598251));
#59140=CARTESIAN_POINT('Ctrl Pts',(-66.,-15.3480342539202,-5.28642814749671));
#59141=CARTESIAN_POINT('Ctrl Pts',(-50.,-15.3480342539202,-5.28642814749671));
#59142=CARTESIAN_POINT('Ctrl Pts',(-66.,-15.2710244971014,-5.21262217319695));
#59143=CARTESIAN_POINT('Ctrl Pts',(-50.,-15.2710244971014,-5.21262217319695));
#59144=CARTESIAN_POINT('Ctrl Pts',(-66.,-15.1931019676527,-5.14053953989829));
#59145=CARTESIAN_POINT('Ctrl Pts',(-50.,-15.1931019676527,-5.14053953989829));
#59146=CARTESIAN_POINT('Ctrl Pts',(-66.,-15.1142708207137,-5.07019831600168));
#59147=CARTESIAN_POINT('Ctrl Pts',(-50.,-15.1142708207137,-5.07019831600168));
#59148=CARTESIAN_POINT('Ctrl Pts',(-66.,-15.0345726196388,-5.00151514537911));
#59149=CARTESIAN_POINT('Ctrl Pts',(-50.,-15.0345726196388,-5.00151514537911));
#59150=CARTESIAN_POINT('Ctrl Pts',(-66.,-14.954068793312,-4.9343541825898));
#59151=CARTESIAN_POINT('Ctrl Pts',(-50.,-14.954068793312,-4.9343541825898));
#59152=CARTESIAN_POINT('Ctrl Pts',(-66.,-14.8728122458042,-4.86860567563393));
#59153=CARTESIAN_POINT('Ctrl Pts',(-50.,-14.8728122458042,-4.86860567563393));
#59154=CARTESIAN_POINT('Ctrl Pts',(-66.,-14.7908208532122,-4.80425948641264));
#59155=CARTESIAN_POINT('Ctrl Pts',(-50.,-14.7908208532122,-4.80425948641264));
#59156=CARTESIAN_POINT('Ctrl Pts',(-66.,-14.7080540513971,-4.74147020990105));
#59157=CARTESIAN_POINT('Ctrl Pts',(-50.,-14.7080540513971,-4.74147020990105));
#59158=CARTESIAN_POINT('Ctrl Pts',(-66.,-14.6243778356077,-4.68065407462106));
#59159=CARTESIAN_POINT('Ctrl Pts',(-50.,-14.6243778356077,-4.68065407462106));
#59160=CARTESIAN_POINT('Ctrl Pts',(-66.,-14.5395956330118,-4.62240562435127));
#59161=CARTESIAN_POINT('Ctrl Pts',(-50.,-14.5395956330118,-4.62240562435127));
#59162=CARTESIAN_POINT('Ctrl Pts',(-66.,-14.4535014438403,-4.56735341407851));
#59163=CARTESIAN_POINT('Ctrl Pts',(-50.,-14.4535014438403,-4.56735341407851));
#59164=CARTESIAN_POINT('Ctrl Pts',(-66.,-14.3659275912213,-4.51603076153944));
#59165=CARTESIAN_POINT('Ctrl Pts',(-50.,-14.3659275912213,-4.51603076153944));
#59166=CARTESIAN_POINT('Ctrl Pts',(-66.,-14.2767906338471,-4.4687510685349));
#59167=CARTESIAN_POINT('Ctrl Pts',(-50.,-14.2767906338471,-4.4687510685349));
#59168=CARTESIAN_POINT('Ctrl Pts',(-66.,-14.1861499417075,-4.42544990152536));
#59169=CARTESIAN_POINT('Ctrl Pts',(-50.,-14.1861499417075,-4.42544990152536));
#59170=CARTESIAN_POINT('Ctrl Pts',(-66.,-14.0941790754254,-4.38575705583354));
#59171=CARTESIAN_POINT('Ctrl Pts',(-50.,-14.0941790754254,-4.38575705583354));
#59172=CARTESIAN_POINT('Ctrl Pts',(-66.,-14.0011148179182,-4.34912763794002));
#59173=CARTESIAN_POINT('Ctrl Pts',(-50.,-14.0011148179182,-4.34912763794002));
#59174=CARTESIAN_POINT('Ctrl Pts',(-66.,-13.9072136271877,-4.31495340364481));
#59175=CARTESIAN_POINT('Ctrl Pts',(-50.,-13.9072136271877,-4.31495340364481));
#59176=CARTESIAN_POINT('Ctrl Pts',(-66.,-13.8127069643429,-4.28267727534445));
#59177=CARTESIAN_POINT('Ctrl Pts',(-50.,-13.8127069643429,-4.28267727534445));
#59178=CARTESIAN_POINT('Ctrl Pts',(-66.,-13.717752718985,-4.25191737627554));
#59179=CARTESIAN_POINT('Ctrl Pts',(-50.,-13.717752718985,-4.25191737627554));
#59180=CARTESIAN_POINT('Ctrl Pts',(-66.,-13.6224454176364,-4.22244373176092));
#59181=CARTESIAN_POINT('Ctrl Pts',(-50.,-13.6224454176364,-4.22244373176092));
#59182=CARTESIAN_POINT('Ctrl Pts',(-66.,-13.5459558574286,-4.19979853847996));
#59183=CARTESIAN_POINT('Ctrl Pts',(-50.,-13.5459558574286,-4.19979853847996));
#59184=CARTESIAN_POINT('Ctrl Pts',(-66.,-13.4884591342042,-4.1833208134517));
#59185=CARTESIAN_POINT('Ctrl Pts',(-50.,-13.4884591342042,-4.1833208134517));
#59186=CARTESIAN_POINT('Ctrl Pts',(-66.,-13.4500704898848,-4.17256031098595));
#59187=CARTESIAN_POINT('Ctrl Pts',(-50.,-13.4500704898848,-4.17256031098595));
#59188=CARTESIAN_POINT('Ctrl Pts',(-66.,-13.4308617934315,-4.1672362226952));
#59189=CARTESIAN_POINT('Ctrl Pts',(-50.,-13.4308617934315,-4.1672362226952));
#59190=CARTESIAN_POINT('Origin',(-65.75,0.,0.));
#59191=CARTESIAN_POINT('',(-65.5,-16.7896631758428,-1.69494408218955));
#59192=CARTESIAN_POINT('Origin',(-65.5,0.,0.));
#59193=CARTESIAN_POINT('Ctrl Pts',(-65.5,-16.7896631758444,-1.69494408219071));
#59194=CARTESIAN_POINT('Ctrl Pts',(-65.5831526942313,-16.7116597831043,
-1.63980921666946));
#59195=CARTESIAN_POINT('Ctrl Pts',(-65.6668642214866,-16.632756953137,-1.58602207616305));
#59196=CARTESIAN_POINT('Ctrl Pts',(-65.7504318115564,-16.5536453909681,
-1.53405266616925));
#59197=CARTESIAN_POINT('Ctrl Pts',(-65.8128644036996,-16.4945418570434,
-1.49522678911148));
#59198=CARTESIAN_POINT('Ctrl Pts',(-65.8752166580337,-16.4353232089395,
-1.45741341708658));
#59199=CARTESIAN_POINT('Ctrl Pts',(-65.9371955299004,-16.3762823874727,
-1.42085043219345));
#59200=CARTESIAN_POINT('Ctrl Pts',(-65.9581769321365,-16.3562955889681,
-1.40847294499675));
#59201=CARTESIAN_POINT('Ctrl Pts',(-65.9791155450307,-16.3363291519437,
-1.39623925385214));
#59202=CARTESIAN_POINT('Ctrl Pts',(-66.,-16.3163944433819,-1.38415944456368));
#59203=CARTESIAN_POINT('Origin',(-58.,0.,0.));
#59204=CARTESIAN_POINT('',(-50.5,-16.7896631758428,-1.69494408218955));
#59205=CARTESIAN_POINT('Origin',(-50.5,0.,0.));
#59206=CARTESIAN_POINT('Ctrl Pts',(-50.5,-16.7896631758428,-1.69494408218955));
#59207=CARTESIAN_POINT('Ctrl Pts',(-55.5,-16.7896631758428,-1.69494408218955));
#59208=CARTESIAN_POINT('Ctrl Pts',(-60.5,-16.7896631758428,-1.69494408218955));
#59209=CARTESIAN_POINT('Ctrl Pts',(-65.5,-16.7896631758428,-1.69494408218955));
#59210=CARTESIAN_POINT('Origin',(-50.25,0.,0.));
#59211=CARTESIAN_POINT('Ctrl Pts',(-50.,-16.3163944433819,-1.38415944456368));
#59212=CARTESIAN_POINT('Ctrl Pts',(-50.0654889940711,-16.3789052444887,
-1.42203903299602));
#59213=CARTESIAN_POINT('Ctrl Pts',(-50.1315105283009,-16.4417279886672,
-1.46142918595527));
#59214=CARTESIAN_POINT('Ctrl Pts',(-50.1977140592374,-16.5045125667653,
-1.50202867177275));
#59215=CARTESIAN_POINT('Ctrl Pts',(-50.271970484712,-16.5749341632954,-1.54756661590145));
#59216=CARTESIAN_POINT('Ctrl Pts',(-50.346455875293,-16.6453067355572,-1.59462664329308));
#59217=CARTESIAN_POINT('Ctrl Pts',(-50.4206755781269,-16.715139000376,-1.64286733678613));
#59218=CARTESIAN_POINT('Ctrl Pts',(-50.4471583693976,-16.7400562827491,
-1.66008039703497));
#59219=CARTESIAN_POINT('Ctrl Pts',(-50.4736073338915,-16.7649048980886,
-1.67744427523805));
#59220=CARTESIAN_POINT('Ctrl Pts',(-50.5,-16.7896631758444,-1.69494408219072));
#59221=CARTESIAN_POINT('Ctrl Pts',(-66.,-14.045256078575,0.696195329812624));
#59222=CARTESIAN_POINT('Ctrl Pts',(-50.,-14.045256078575,0.696195329812624));
#59223=CARTESIAN_POINT('Ctrl Pts',(-66.,-14.0686273356774,0.696392218370307));
#59224=CARTESIAN_POINT('Ctrl Pts',(-50.,-14.0686273356774,0.696392218370307));
#59225=CARTESIAN_POINT('Ctrl Pts',(-66.,-14.1153770624506,0.697010974492569));
#59226=CARTESIAN_POINT('Ctrl Pts',(-50.,-14.1153770624506,0.697010974492569));
#59227=CARTESIAN_POINT('Ctrl Pts',(-66.,-14.1855232971663,0.698614034227448));
#59228=CARTESIAN_POINT('Ctrl Pts',(-50.,-14.1855232971663,0.698614034227448));
#59229=CARTESIAN_POINT('Ctrl Pts',(-66.,-14.279094897617,0.702103192289484));
#59230=CARTESIAN_POINT('Ctrl Pts',(-50.,-14.279094897617,0.702103192289484));
#59231=CARTESIAN_POINT('Ctrl Pts',(-66.,-14.3961143752671,0.708771950396692));
#59232=CARTESIAN_POINT('Ctrl Pts',(-50.,-14.3961143752671,0.708771950396692));
#59233=CARTESIAN_POINT('Ctrl Pts',(-66.,-14.5131355638642,0.717895108848178));
#59234=CARTESIAN_POINT('Ctrl Pts',(-50.,-14.5131355638642,0.717895108848178));
#59235=CARTESIAN_POINT('Ctrl Pts',(-66.,-14.6300532595709,0.7297502981378));
#59236=CARTESIAN_POINT('Ctrl Pts',(-50.,-14.6300532595709,0.7297502981378));
#59237=CARTESIAN_POINT('Ctrl Pts',(-66.,-14.7466862135917,0.744796901078022));
#59238=CARTESIAN_POINT('Ctrl Pts',(-50.,-14.7466862135917,0.744796901078022));
#59239=CARTESIAN_POINT('Ctrl Pts',(-66.,-14.8628229502399,0.763626728348506));
#59240=CARTESIAN_POINT('Ctrl Pts',(-50.,-14.8628229502399,0.763626728348506));
#59241=CARTESIAN_POINT('Ctrl Pts',(-66.,-14.97828481366,0.786901644277719));
#59242=CARTESIAN_POINT('Ctrl Pts',(-50.,-14.97828481366,0.786901644277719));
#59243=CARTESIAN_POINT('Ctrl Pts',(-66.,-15.0929746515511,0.81528653252832));
#59244=CARTESIAN_POINT('Ctrl Pts',(-50.,-15.0929746515511,0.81528653252832));
#59245=CARTESIAN_POINT('Ctrl Pts',(-66.,-15.2069528955437,0.849407044643804));
#59246=CARTESIAN_POINT('Ctrl Pts',(-50.,-15.2069528955437,0.849407044643804));
#59247=CARTESIAN_POINT('Ctrl Pts',(-66.,-15.3203905800386,0.889657803015486));
#59248=CARTESIAN_POINT('Ctrl Pts',(-50.,-15.3203905800386,0.889657803015486));
#59249=CARTESIAN_POINT('Ctrl Pts',(-66.,-15.4334553338124,0.935889193512498));
#59250=CARTESIAN_POINT('Ctrl Pts',(-50.,-15.4334553338124,0.935889193512498));
#59251=CARTESIAN_POINT('Ctrl Pts',(-66.,-15.5462329906162,0.987208158041752));
#59252=CARTESIAN_POINT('Ctrl Pts',(-50.,-15.5462329906162,0.987208158041752));
#59253=CARTESIAN_POINT('Ctrl Pts',(-66.,-15.6586006138651,1.04154270247793));
#59254=CARTESIAN_POINT('Ctrl Pts',(-50.,-15.6586006138651,1.04154270247793));
#59255=CARTESIAN_POINT('Ctrl Pts',(-66.,-15.7702454432537,1.09599839647648));
#59256=CARTESIAN_POINT('Ctrl Pts',(-50.,-15.7702454432537,1.09599839647648));
#59257=CARTESIAN_POINT('Ctrl Pts',(-66.,-15.8808661517589,1.14825710837788));
#59258=CARTESIAN_POINT('Ctrl Pts',(-50.,-15.8808661517589,1.14825710837788));
#59259=CARTESIAN_POINT('Ctrl Pts',(-66.,-15.9903135820168,1.19759548023257));
#59260=CARTESIAN_POINT('Ctrl Pts',(-50.,-15.9903135820168,1.19759548023257));
#59261=CARTESIAN_POINT('Ctrl Pts',(-66.,-16.0987879364791,1.2463210640833));
#59262=CARTESIAN_POINT('Ctrl Pts',(-50.,-16.0987879364791,1.2463210640833));
#59263=CARTESIAN_POINT('Ctrl Pts',(-66.,-16.2069202965129,1.30027898254334));
#59264=CARTESIAN_POINT('Ctrl Pts',(-50.,-16.2069202965129,1.30027898254334));
#59265=CARTESIAN_POINT('Ctrl Pts',(-66.,-16.3153998369687,1.36562590713335));
#59266=CARTESIAN_POINT('Ctrl Pts',(-50.,-16.3153998369687,1.36562590713335));
#59267=CARTESIAN_POINT('Ctrl Pts',(-66.,-16.424658248998,1.44607062429677));
#59268=CARTESIAN_POINT('Ctrl Pts',(-50.,-16.424658248998,1.44607062429677));
#59269=CARTESIAN_POINT('Ctrl Pts',(-66.,-16.5345463329789,1.54005835913147));
#59270=CARTESIAN_POINT('Ctrl Pts',(-50.,-16.5345463329789,1.54005835913147));
#59271=CARTESIAN_POINT('Ctrl Pts',(-66.,-16.6439703236082,1.63759217997151));
#59272=CARTESIAN_POINT('Ctrl Pts',(-50.,-16.6439703236082,1.63759217997151));
#59273=CARTESIAN_POINT('Ctrl Pts',(-66.,-16.751164098444,1.72267382202435));
#59274=CARTESIAN_POINT('Ctrl Pts',(-50.,-16.751164098444,1.72267382202435));
#59275=CARTESIAN_POINT('Ctrl Pts',(-66.,-16.8540367989194,1.77640986861434));
#59276=CARTESIAN_POINT('Ctrl Pts',(-50.,-16.8540367989194,1.77640986861434));
#59277=CARTESIAN_POINT('Ctrl Pts',(-66.,-16.9504681139093,1.77965278795706));
#59278=CARTESIAN_POINT('Ctrl Pts',(-50.,-16.9504681139093,1.77965278795706));
#59279=CARTESIAN_POINT('Ctrl Pts',(-66.,-17.0386813073781,1.71633428927379));
#59280=CARTESIAN_POINT('Ctrl Pts',(-50.,-17.0386813073781,1.71633428927379));
#59281=CARTESIAN_POINT('Ctrl Pts',(-66.,-17.1173432554706,1.57436164343055));
#59282=CARTESIAN_POINT('Ctrl Pts',(-50.,-17.1173432554706,1.57436164343055));
#59283=CARTESIAN_POINT('Ctrl Pts',(-66.,-17.1854641388117,1.34472480942369));
#59284=CARTESIAN_POINT('Ctrl Pts',(-50.,-17.1854641388117,1.34472480942369));
#59285=CARTESIAN_POINT('Ctrl Pts',(-66.,-17.2423578994913,1.02114561862921));
#59286=CARTESIAN_POINT('Ctrl Pts',(-50.,-17.2423578994913,1.02114561862921));
#59287=CARTESIAN_POINT('Ctrl Pts',(-66.,-17.2875806747963,0.599529862462145));
#59288=CARTESIAN_POINT('Ctrl Pts',(-50.,-17.2875806747963,0.599529862462145));
#59289=CARTESIAN_POINT('Ctrl Pts',(-66.,-17.3208814627092,0.0775281531615438));
#59290=CARTESIAN_POINT('Ctrl Pts',(-50.,-17.3208814627092,0.0775281531615438));
#59291=CARTESIAN_POINT('Ctrl Pts',(-66.,-17.3421500762616,-0.545927845218096));
#59292=CARTESIAN_POINT('Ctrl Pts',(-50.,-17.3421500762616,-0.545927845218096));
#59293=CARTESIAN_POINT('Ctrl Pts',(-66.,-17.3495248726512,-1.12603243333965));
#59294=CARTESIAN_POINT('Ctrl Pts',(-50.,-17.3495248726512,-1.12603243333965));
#59295=CARTESIAN_POINT('Ctrl Pts',(-66.,-17.3496452331689,-1.60677512854574));
#59296=CARTESIAN_POINT('Ctrl Pts',(-50.,-17.3496452331689,-1.60677512854574));
#59297=CARTESIAN_POINT('Ctrl Pts',(-66.,-17.3473238999477,-1.94753848896561));
#59298=CARTESIAN_POINT('Ctrl Pts',(-50.,-17.3473238999477,-1.94753848896561));
#59299=CARTESIAN_POINT('Ctrl Pts',(-66.,-17.345562839687,-2.12298722899376));
#59300=CARTESIAN_POINT('Ctrl Pts',(-50.,-17.345562839687,-2.12298722899376));
#59301=CARTESIAN_POINT('',(-65.5,-16.7854722368145,1.73595702341129));
#59302=CARTESIAN_POINT('Ctrl Pts',(-66.,-16.3175338509752,1.37066189203528));
#59303=CARTESIAN_POINT('Ctrl Pts',(-65.8729887704777,-16.4381764834115,
1.45180418206711));
#59304=CARTESIAN_POINT('Ctrl Pts',(-65.7718691849107,-16.5316964789852,
1.54005558503416));
#59305=CARTESIAN_POINT('Ctrl Pts',(-65.6164770304283,-16.675938104789,1.66211853613209));
#59306=CARTESIAN_POINT('Ctrl Pts',(-65.5625284355056,-16.7261279559211,
1.70187129664813));
#59307=CARTESIAN_POINT('Ctrl Pts',(-65.5076868273056,-16.7781614587951,
1.73192223528954));
#59308=CARTESIAN_POINT('Ctrl Pts',(-65.5038549844531,-16.7818026870438,
1.73396519020203));
#59309=CARTESIAN_POINT('Ctrl Pts',(-65.5,-16.7854722368145,1.73595702341129));
#59310=CARTESIAN_POINT('',(-66.,-14.045256078575,0.696195329812624));
#59311=CARTESIAN_POINT('',(-50.5,-16.7854722368145,1.73595702341129));
#59312=CARTESIAN_POINT('Ctrl Pts',(-50.5,-16.7854722368145,1.73595702341129));
#59313=CARTESIAN_POINT('Ctrl Pts',(-50.4675027013721,-16.754538141962,1.71916598329007));
#59314=CARTESIAN_POINT('Ctrl Pts',(-50.4339845147439,-16.7230774265929,
1.6973772200423));
#59315=CARTESIAN_POINT('Ctrl Pts',(-50.2820350749108,-16.5813058210333,
1.58823427035107));
#59316=CARTESIAN_POINT('Ctrl Pts',(-50.1596733333234,-16.4692008439998,
1.47267066694127));
#59317=CARTESIAN_POINT('Ctrl Pts',(-50.,-16.3175338509752,1.37066189203528));
#59318=CARTESIAN_POINT('Ctrl Pts',(-65.5,-16.7854722368145,1.73595702341129));
#59319=CARTESIAN_POINT('Ctrl Pts',(-60.5,-16.7854722368145,1.73595702341129));
#59320=CARTESIAN_POINT('Ctrl Pts',(-55.5,-16.7854722368145,1.73595702341129));
#59321=CARTESIAN_POINT('Ctrl Pts',(-50.5,-16.7854722368145,1.73595702341129));
#59322=CARTESIAN_POINT('Origin',(-66.,0.,0.));
#59323=CARTESIAN_POINT('',(-66.,-14.045256078575,-0.696195329812616));
#59324=CARTESIAN_POINT('Ctrl Pts',(-66.,-17.345562839687,-2.12298722899376));
#59325=CARTESIAN_POINT('Ctrl Pts',(-50.,-17.345562839687,-2.12298722899376));
#59326=CARTESIAN_POINT('Ctrl Pts',(-66.,-17.3282886320894,-2.10855557872225));
#59327=CARTESIAN_POINT('Ctrl Pts',(-50.,-17.3282886320894,-2.10855557872225));
#59328=CARTESIAN_POINT('Ctrl Pts',(-66.,-17.2936892204412,-2.07983106708238));
#59329=CARTESIAN_POINT('Ctrl Pts',(-50.,-17.2936892204412,-2.07983106708238));
#59330=CARTESIAN_POINT('Ctrl Pts',(-66.,-17.241637113787,-2.03716066567899));
#59331=CARTESIAN_POINT('Ctrl Pts',(-50.,-17.241637113787,-2.03716066567899));
#59332=CARTESIAN_POINT('Ctrl Pts',(-66.,-17.1719279181019,-1.98110064232955));
#59333=CARTESIAN_POINT('Ctrl Pts',(-50.,-17.1719279181019,-1.98110064232955));
#59334=CARTESIAN_POINT('Ctrl Pts',(-66.,-17.0842789796692,-1.91242115216328));
#59335=CARTESIAN_POINT('Ctrl Pts',(-50.,-17.0842789796692,-1.91242115216328));
#59336=CARTESIAN_POINT('Ctrl Pts',(-66.,-16.9961162868454,-1.84514350065724));
#59337=CARTESIAN_POINT('Ctrl Pts',(-50.,-16.9961162868454,-1.84514350065724));
#59338=CARTESIAN_POINT('Ctrl Pts',(-66.,-16.9074403974186,-1.77927159805394));
#59339=CARTESIAN_POINT('Ctrl Pts',(-50.,-16.9074403974186,-1.77927159805394));
#59340=CARTESIAN_POINT('Ctrl Pts',(-66.,-16.8182550149921,-1.71480453952538));
#59341=CARTESIAN_POINT('Ctrl Pts',(-50.,-16.8182550149921,-1.71480453952538));
#59342=CARTESIAN_POINT('Ctrl Pts',(-66.,-16.7285687128188,-1.65173252825902));
#59343=CARTESIAN_POINT('Ctrl Pts',(-50.,-16.7285687128188,-1.65173252825902));
#59344=CARTESIAN_POINT('Ctrl Pts',(-66.,-16.6383931283473,-1.59004626593597));
#59345=CARTESIAN_POINT('Ctrl Pts',(-50.,-16.6383931283473,-1.59004626593597));
#59346=CARTESIAN_POINT('Ctrl Pts',(-66.,-16.5477407361381,-1.52974779117622));
#59347=CARTESIAN_POINT('Ctrl Pts',(-50.,-16.5477407361381,-1.52974779117622));
#59348=CARTESIAN_POINT('Ctrl Pts',(-66.,-16.456622719418,-1.4708615729337));
#59349=CARTESIAN_POINT('Ctrl Pts',(-50.,-16.456622719418,-1.4708615729337));
#59350=CARTESIAN_POINT('Ctrl Pts',(-66.,-16.3650471090276,-1.41344345684179));
#59351=CARTESIAN_POINT('Ctrl Pts',(-50.,-16.3650471090276,-1.41344345684179));
#59352=CARTESIAN_POINT('Ctrl Pts',(-66.,-16.2730161904774,-1.35759562886537));
#59353=CARTESIAN_POINT('Ctrl Pts',(-50.,-16.2730161904774,-1.35759562886537));
#59354=CARTESIAN_POINT('Ctrl Pts',(-66.,-16.1805287542786,-1.30344437937201));
#59355=CARTESIAN_POINT('Ctrl Pts',(-50.,-16.1805287542786,-1.30344437937201));
#59356=CARTESIAN_POINT('Ctrl Pts',(-66.,-16.0875836011606,-1.25110870320843));
#59357=CARTESIAN_POINT('Ctrl Pts',(-50.,-16.0875836011606,-1.25110870320843));
#59358=CARTESIAN_POINT('Ctrl Pts',(-66.,-15.9941829293225,-1.20066922344171));
#59359=CARTESIAN_POINT('Ctrl Pts',(-50.,-15.9941829293225,-1.20066922344171));
#59360=CARTESIAN_POINT('Ctrl Pts',(-66.,-15.900335256791,-1.15214240747963));
#59361=CARTESIAN_POINT('Ctrl Pts',(-50.,-15.900335256791,-1.15214240747963));
#59362=CARTESIAN_POINT('Ctrl Pts',(-66.,-15.8060601113054,-1.10543718159424));
#59363=CARTESIAN_POINT('Ctrl Pts',(-50.,-15.8060601113054,-1.10543718159424));
#59364=CARTESIAN_POINT('Ctrl Pts',(-66.,-15.7113832084608,-1.06040669143688));
#59365=CARTESIAN_POINT('Ctrl Pts',(-50.,-15.7113832084608,-1.06040669143688));
#59366=CARTESIAN_POINT('Ctrl Pts',(-66.,-15.6163284960372,-1.01693147636119));
#59367=CARTESIAN_POINT('Ctrl Pts',(-50.,-15.6163284960372,-1.01693147636119));
#59368=CARTESIAN_POINT('Ctrl Pts',(-66.,-15.5209107672782,-0.974997271170846));
#59369=CARTESIAN_POINT('Ctrl Pts',(-50.,-15.5209107672782,-0.974997271170846));
#59370=CARTESIAN_POINT('Ctrl Pts',(-66.,-15.4251291786488,-0.934763901846662));
#59371=CARTESIAN_POINT('Ctrl Pts',(-50.,-15.4251291786488,-0.934763901846662));
#59372=CARTESIAN_POINT('Ctrl Pts',(-66.,-15.3289574472276,-0.89666784595261));
#59373=CARTESIAN_POINT('Ctrl Pts',(-50.,-15.3289574472276,-0.89666784595261));
#59374=CARTESIAN_POINT('Ctrl Pts',(-66.,-15.2323530329047,-0.861333854256595));
#59375=CARTESIAN_POINT('Ctrl Pts',(-50.,-15.2323530329047,-0.861333854256595));
#59376=CARTESIAN_POINT('Ctrl Pts',(-66.,-15.1352727230412,-0.829421964594113));
#59377=CARTESIAN_POINT('Ctrl Pts',(-50.,-15.1352727230412,-0.829421964594113));
#59378=CARTESIAN_POINT('Ctrl Pts',(-66.,-15.0376867393704,-0.801490439086723));
#59379=CARTESIAN_POINT('Ctrl Pts',(-50.,-15.0376867393704,-0.801490439086723));
#59380=CARTESIAN_POINT('Ctrl Pts',(-66.,-14.939592201905,-0.777863584450799));
#59381=CARTESIAN_POINT('Ctrl Pts',(-50.,-14.939592201905,-0.777863584450799));
#59382=CARTESIAN_POINT('Ctrl Pts',(-66.,-14.8410305914479,-0.758464226728878));
#59383=CARTESIAN_POINT('Ctrl Pts',(-50.,-14.8410305914479,-0.758464226728878));
#59384=CARTESIAN_POINT('Ctrl Pts',(-66.,-14.7420779497362,-0.742890629132665));
#59385=CARTESIAN_POINT('Ctrl Pts',(-50.,-14.7420779497362,-0.742890629132665));
#59386=CARTESIAN_POINT('Ctrl Pts',(-66.,-14.6428281112089,-0.730556131457601));
#59387=CARTESIAN_POINT('Ctrl Pts',(-50.,-14.6428281112089,-0.730556131457601));
#59388=CARTESIAN_POINT('Ctrl Pts',(-66.,-14.5433782125866,-0.72080782010221));
#59389=CARTESIAN_POINT('Ctrl Pts',(-50.,-14.5433782125866,-0.72080782010221));
#59390=CARTESIAN_POINT('Ctrl Pts',(-66.,-14.4438139036356,-0.71304855704325));
#59391=CARTESIAN_POINT('Ctrl Pts',(-50.,-14.4438139036356,-0.71304855704325));
#59392=CARTESIAN_POINT('Ctrl Pts',(-66.,-14.3441931446757,-0.706869197330954));
#59393=CARTESIAN_POINT('Ctrl Pts',(-50.,-14.3441931446757,-0.706869197330954));
#59394=CARTESIAN_POINT('Ctrl Pts',(-66.,-14.2445503001281,-0.702023483575367));
#59395=CARTESIAN_POINT('Ctrl Pts',(-50.,-14.2445503001281,-0.702023483575367));
#59396=CARTESIAN_POINT('Ctrl Pts',(-66.,-14.1648321695468,-0.699111910780302));
#59397=CARTESIAN_POINT('Ctrl Pts',(-50.,-14.1648321695468,-0.699111910780302));
#59398=CARTESIAN_POINT('Ctrl Pts',(-66.,-14.1050439680336,-0.697450717395246));
#59399=CARTESIAN_POINT('Ctrl Pts',(-50.,-14.1050439680336,-0.697450717395246));
#59400=CARTESIAN_POINT('Ctrl Pts',(-66.,-14.0651853454231,-0.696575143525857));
#59401=CARTESIAN_POINT('Ctrl Pts',(-50.,-14.0651853454231,-0.696575143525857));
#59402=CARTESIAN_POINT('Ctrl Pts',(-66.,-14.045256078575,-0.696195329812629));
#59403=CARTESIAN_POINT('Ctrl Pts',(-50.,-14.045256078575,-0.696195329812629));
#59404=CARTESIAN_POINT('Origin',(-65.75,0.,0.));
#59405=CARTESIAN_POINT('',(-65.5,-16.6837004856932,2.53372514367283));
#59406=CARTESIAN_POINT('Origin',(-65.5,0.,0.));
#59407=CARTESIAN_POINT('Ctrl Pts',(-65.5,-16.6837004857171,2.53372514366373));
#59408=CARTESIAN_POINT('Ctrl Pts',(-65.5738810032737,-16.6043913553664,
2.56393691646143));
#59409=CARTESIAN_POINT('Ctrl Pts',(-65.647826758183,-16.5250605133332,2.59279124243202));
#59410=CARTESIAN_POINT('Ctrl Pts',(-65.7215770308288,-16.4460101931368,
2.6202092323328));
#59411=CARTESIAN_POINT('Ctrl Pts',(-65.7821649037802,-16.3810681856701,
2.64273386348462));
#59412=CARTESIAN_POINT('Ctrl Pts',(-65.842620844317,-16.3163158245858,2.6642910002248));
#59413=CARTESIAN_POINT('Ctrl Pts',(-65.9028005644781,-16.2519319156941,
2.68479258877889));
#59414=CARTESIAN_POINT('Ctrl Pts',(-65.935288443709,-16.2171744151459,2.6958603227465));
#59415=CARTESIAN_POINT('Ctrl Pts',(-65.967695822527,-16.1825245252962,2.70661906026748));
#59416=CARTESIAN_POINT('Ctrl Pts',(-66.,-16.1480113642792,2.71704876274038));
#59417=CARTESIAN_POINT('Origin',(-58.,0.,0.));
#59418=CARTESIAN_POINT('',(-50.5,-16.6837004856932,2.53372514367283));
#59419=CARTESIAN_POINT('Origin',(-50.5,0.,0.));
#59420=CARTESIAN_POINT('Ctrl Pts',(-50.5,-16.6837004856932,2.53372514367283));
#59421=CARTESIAN_POINT('Ctrl Pts',(-55.5,-16.6837004856932,2.53372514367283));
#59422=CARTESIAN_POINT('Ctrl Pts',(-60.5,-16.6837004856932,2.53372514367283));
#59423=CARTESIAN_POINT('Ctrl Pts',(-65.5,-16.6837004856932,2.53372514367283));
#59424=CARTESIAN_POINT('Origin',(-50.25,0.,0.));
#59425=CARTESIAN_POINT('Ctrl Pts',(-50.,-16.1480113642792,2.71704876274038));
#59426=CARTESIAN_POINT('Ctrl Pts',(-50.0601511103782,-16.2122756520658,
2.69762842042758));
#59427=CARTESIAN_POINT('Ctrl Pts',(-50.1206600330683,-16.2770136258072,
2.6770696979896));
#59428=CARTESIAN_POINT('Ctrl Pts',(-50.1813802137674,-16.3420386981439,
2.65549281295864));
#59429=CARTESIAN_POINT('Ctrl Pts',(-50.2450302523274,-16.4102013471008,
2.63287480444134));
#59430=CARTESIAN_POINT('Ctrl Pts',(-50.3089124279122,-16.4786791569631,
2.60913798457234));
#59431=CARTESIAN_POINT('Ctrl Pts',(-50.3728579315898,-16.5472689407516,
2.58435539231395));
#59432=CARTESIAN_POINT('Ctrl Pts',(-50.4152271869693,-16.5927154209358,
2.56793484794457));
#59433=CARTESIAN_POINT('Ctrl Pts',(-50.4576242444773,-16.638211331949,2.55105364004647));
#59434=CARTESIAN_POINT('Ctrl Pts',(-50.5,-16.6837004857171,2.53372514366373));
#59435=CARTESIAN_POINT('Ctrl Pts',(-66.,-13.4308617934315,4.1672362226952));
#59436=CARTESIAN_POINT('Ctrl Pts',(-50.,-13.4308617934315,4.1672362226952));
#59437=CARTESIAN_POINT('Ctrl Pts',(-66.,-13.4534498353221,4.1732391209285));
#59438=CARTESIAN_POINT('Ctrl Pts',(-50.,-13.4534498353221,4.1732391209285));
#59439=CARTESIAN_POINT('Ctrl Pts',(-66.,-13.4985769550718,4.18546462196559));
#59440=CARTESIAN_POINT('Ctrl Pts',(-50.,-13.4985769550718,4.18546462196559));
#59441=CARTESIAN_POINT('Ctrl Pts',(-66.,-13.5661207520894,4.20446197782756));
#59442=CARTESIAN_POINT('Ctrl Pts',(-50.,-13.5661207520894,4.20446197782756));
#59443=CARTESIAN_POINT('Ctrl Pts',(-66.,-13.655884910321,4.23111182833087));
#59444=CARTESIAN_POINT('Ctrl Pts',(-50.,-13.655884910321,4.23111182833087));
#59445=CARTESIAN_POINT('Ctrl Pts',(-66.,-13.7675695531958,4.26667263583206));
#59446=CARTESIAN_POINT('Ctrl Pts',(-50.,-13.7675695531958,4.26667263583206));
#59447=CARTESIAN_POINT('Ctrl Pts',(-66.,-13.8786454687203,4.30461115967259));
#59448=CARTESIAN_POINT('Ctrl Pts',(-50.,-13.8786454687203,4.30461115967259));
#59449=CARTESIAN_POINT('Ctrl Pts',(-66.,-13.988941714333,4.34517014494338));
#59450=CARTESIAN_POINT('Ctrl Pts',(-50.,-13.988941714333,4.34517014494338));
#59451=CARTESIAN_POINT('Ctrl Pts',(-66.,-14.0981684916428,4.38874946735859));
#59452=CARTESIAN_POINT('Ctrl Pts',(-50.,-14.0981684916428,4.38874946735859));
#59453=CARTESIAN_POINT('Ctrl Pts',(-66.,-14.2059737915295,4.4358697529125));
#59454=CARTESIAN_POINT('Ctrl Pts',(-50.,-14.2059737915295,4.4358697529125));
#59455=CARTESIAN_POINT('Ctrl Pts',(-66.,-14.3120199719745,4.48712764234399));
#59456=CARTESIAN_POINT('Ctrl Pts',(-50.,-14.3120199719745,4.48712764234399));
#59457=CARTESIAN_POINT('Ctrl Pts',(-66.,-14.4160475830522,4.54314296997813));
#59458=CARTESIAN_POINT('Ctrl Pts',(-50.,-14.4160475830522,4.54314296997813));
#59459=CARTESIAN_POINT('Ctrl Pts',(-66.,-14.5179595646104,4.60453676010005));
#59460=CARTESIAN_POINT('Ctrl Pts',(-50.,-14.5179595646104,4.60453676010005));
#59461=CARTESIAN_POINT('Ctrl Pts',(-66.,-14.6178234390918,4.67173377183878));
#59462=CARTESIAN_POINT('Ctrl Pts',(-50.,-14.6178234390918,4.67173377183878));
#59463=CARTESIAN_POINT('Ctrl Pts',(-66.,-14.7158387764281,4.74463077904808));
#59464=CARTESIAN_POINT('Ctrl Pts',(-50.,-14.7158387764281,4.74463077904808));
#59465=CARTESIAN_POINT('Ctrl Pts',(-66.,-14.8123108082616,4.82238412668293));
#59466=CARTESIAN_POINT('Ctrl Pts',(-50.,-14.8123108082616,4.82238412668293));
#59467=CARTESIAN_POINT('Ctrl Pts',(-66.,-14.9076357442716,4.90295634303817));
#59468=CARTESIAN_POINT('Ctrl Pts',(-50.,-14.9076357442716,4.90295634303817));
#59469=CARTESIAN_POINT('Ctrl Pts',(-66.,-15.0022304656484,4.98346615129592));
#59470=CARTESIAN_POINT('Ctrl Pts',(-50.,-15.0022304656484,4.98346615129592));
#59471=CARTESIAN_POINT('Ctrl Pts',(-66.,-15.0963796080126,5.06159331118216));
#59472=CARTESIAN_POINT('Ctrl Pts',(-50.,-15.0963796080126,5.06159331118216));
#59473=CARTESIAN_POINT('Ctrl Pts',(-66.,-15.1901185918597,5.13660009643943));
#59474=CARTESIAN_POINT('Ctrl Pts',(-50.,-15.1901185918597,5.13660009643943));
#59475=CARTESIAN_POINT('Ctrl Pts',(-66.,-15.2830674650563,5.2107713514449));
#59476=CARTESIAN_POINT('Ctrl Pts',(-50.,-15.2830674650563,5.2107713514449));
#59477=CARTESIAN_POINT('Ctrl Pts',(-66.,-15.3743838595047,5.28992550709052));
#59478=CARTESIAN_POINT('Ctrl Pts',(-50.,-15.3743838595047,5.28992550709052));
#59479=CARTESIAN_POINT('Ctrl Pts',(-66.,-15.4632041964143,5.3801972025556));
#59480=CARTESIAN_POINT('Ctrl Pts',(-50.,-15.4632041964143,5.3801972025556));
#59481=CARTESIAN_POINT('Ctrl Pts',(-66.,-15.5490242668831,5.48528606316123));
#59482=CARTESIAN_POINT('Ctrl Pts',(-50.,-15.5490242668831,5.48528606316123));
#59483=CARTESIAN_POINT('Ctrl Pts',(-66.,-15.6320862154648,5.6036490556807));
#59484=CARTESIAN_POINT('Ctrl Pts',(-50.,-15.6320862154648,5.6036490556807));
#59485=CARTESIAN_POINT('Ctrl Pts',(-66.,-15.7138167753124,5.72533131206965));
#59486=CARTESIAN_POINT('Ctrl Pts',(-50.,-15.7138167753124,5.72533131206965));
#59487=CARTESIAN_POINT('Ctrl Pts',(-66.,-15.7964839166342,5.83439796565188));
#59488=CARTESIAN_POINT('Ctrl Pts',(-50.,-15.7964839166342,5.83439796565188));
#59489=CARTESIAN_POINT('Ctrl Pts',(-66.,-15.8827610706914,5.91202919579815));
#59490=CARTESIAN_POINT('Ctrl Pts',(-50.,-15.8827610706914,5.91202919579815));
#59491=CARTESIAN_POINT('Ctrl Pts',(-66.,-15.9753563373507,5.9391517257104));
#59492=CARTESIAN_POINT('Ctrl Pts',(-50.,-15.9753563373507,5.9391517257104));
#59493=CARTESIAN_POINT('Ctrl Pts',(-66.,-16.0765448214269,5.89976022322805));
#59494=CARTESIAN_POINT('Ctrl Pts',(-50.,-16.0765448214269,5.89976022322805));
#59495=CARTESIAN_POINT('Ctrl Pts',(-66.,-16.1880426210461,5.78181034011869));
#59496=CARTESIAN_POINT('Ctrl Pts',(-50.,-16.1880426210461,5.78181034011869));
#59497=CARTESIAN_POINT('Ctrl Pts',(-66.,-16.3111317199096,5.57632894431644));
#59498=CARTESIAN_POINT('Ctrl Pts',(-50.,-16.3111317199096,5.57632894431644));
#59499=CARTESIAN_POINT('Ctrl Pts',(-66.,-16.4467089309247,5.27706449174507));
#59500=CARTESIAN_POINT('Ctrl Pts',(-50.,-16.4467089309247,5.27706449174507));
#59501=CARTESIAN_POINT('Ctrl Pts',(-66.,-16.5953625244127,4.879941016743));
#59502=CARTESIAN_POINT('Ctrl Pts',(-50.,-16.5953625244127,4.879941016743));
#59503=CARTESIAN_POINT('Ctrl Pts',(-66.,-16.7574336530234,4.38262052022265));
#59504=CARTESIAN_POINT('Ctrl Pts',(-50.,-16.7574336530234,4.38262052022265));
#59505=CARTESIAN_POINT('Ctrl Pts',(-66.,-16.93308127586,3.78404082759198));
#59506=CARTESIAN_POINT('Ctrl Pts',(-50.,-16.93308127586,3.78404082759198));
#59507=CARTESIAN_POINT('Ctrl Pts',(-66.,-17.0844905240235,3.22399532912598));
#59508=CARTESIAN_POINT('Ctrl Pts',(-50.,-17.0844905240235,3.22399532912598));
#59509=CARTESIAN_POINT('Ctrl Pts',(-66.,-17.2041629498203,2.75838598215733));
#59510=CARTESIAN_POINT('Ctrl Pts',(-50.,-17.2041629498203,2.75838598215733));
#59511=CARTESIAN_POINT('Ctrl Pts',(-66.,-17.2866589472037,2.4277510372282));
#59512=CARTESIAN_POINT('Ctrl Pts',(-50.,-17.2866589472037,2.4277510372282));
#59513=CARTESIAN_POINT('Ctrl Pts',(-66.,-17.3285855412502,2.25737638411816));
#59514=CARTESIAN_POINT('Ctrl Pts',(-50.,-17.3285855412502,2.25737638411816));
#59515=CARTESIAN_POINT('',(-65.5,-15.8264108038954,5.85579593790134));
#59516=CARTESIAN_POINT('Ctrl Pts',(-66.,-15.4640187679296,5.38560568043381));
#59517=CARTESIAN_POINT('Ctrl Pts',(-65.7933280154035,-15.6213248025723,
5.56231194751196));
#59518=CARTESIAN_POINT('Ctrl Pts',(-65.637076174949,-15.7176413861457,5.75474546238425));
#59519=CARTESIAN_POINT('Ctrl Pts',(-65.5,-15.8264108038954,5.85579593790134));
#59520=CARTESIAN_POINT('',(-66.,-13.4308617934315,4.1672362226952));
#59521=CARTESIAN_POINT('',(-50.5,-15.8264108038954,5.85579593790134));
#59522=CARTESIAN_POINT('Ctrl Pts',(-50.5,-15.8264108038954,5.85579593790134));
#59523=CARTESIAN_POINT('Ctrl Pts',(-50.4432204291973,-15.7813564327869,
5.81393890015279));
#59524=CARTESIAN_POINT('Ctrl Pts',(-50.3822807385572,-15.7377169583822,
5.75610061597894));
#59525=CARTESIAN_POINT('Ctrl Pts',(-50.2209130984549,-15.6244042480767,
5.59526303189522));
#59526=CARTESIAN_POINT('Ctrl Pts',(-50.1226480777072,-15.5573709598018,
5.49047080774294));
#59527=CARTESIAN_POINT('Ctrl Pts',(-50.,-15.4640187679296,5.38560568043381));
#59528=CARTESIAN_POINT('Ctrl Pts',(-65.5,-15.8264108038954,5.85579593790135));
#59529=CARTESIAN_POINT('Ctrl Pts',(-60.5,-15.8264108038954,5.85579593790135));
#59530=CARTESIAN_POINT('Ctrl Pts',(-55.5,-15.8264108038954,5.85579593790135));
#59531=CARTESIAN_POINT('Ctrl Pts',(-50.5,-15.8264108038954,5.85579593790135));
#59532=CARTESIAN_POINT('Origin',(-66.,0.,0.));
#59533=CARTESIAN_POINT('',(-66.,-13.7771352694631,2.8185900760694));
#59534=CARTESIAN_POINT('Ctrl Pts',(-66.,-17.3285855412502,2.25737638411816));
#59535=CARTESIAN_POINT('Ctrl Pts',(-50.,-17.3285855412502,2.25737638411816));
#59536=CARTESIAN_POINT('Ctrl Pts',(-66.,-17.3082650291717,2.26705871682014));
#59537=CARTESIAN_POINT('Ctrl Pts',(-50.,-17.3082650291717,2.26705871682014));
#59538=CARTESIAN_POINT('Ctrl Pts',(-66.,-17.2676091261057,2.28627627132739));
#59539=CARTESIAN_POINT('Ctrl Pts',(-50.,-17.2676091261057,2.28627627132739));
#59540=CARTESIAN_POINT('Ctrl Pts',(-66.,-17.2065806347889,2.31466127107479));
#59541=CARTESIAN_POINT('Ctrl Pts',(-50.,-17.2065806347889,2.31466127107479));
#59542=CARTESIAN_POINT('Ctrl Pts',(-66.,-17.1251199207912,2.35162409369425));
#59543=CARTESIAN_POINT('Ctrl Pts',(-50.,-17.1251199207912,2.35162409369425));
#59544=CARTESIAN_POINT('Ctrl Pts',(-66.,-17.0231447402746,2.39634848677526));
#59545=CARTESIAN_POINT('Ctrl Pts',(-50.,-17.0231447402746,2.39634848677526));
#59546=CARTESIAN_POINT('Ctrl Pts',(-66.,-16.921020569004,2.4395873170138));
#59547=CARTESIAN_POINT('Ctrl Pts',(-50.,-16.921020569004,2.4395873170138));
#59548=CARTESIAN_POINT('Ctrl Pts',(-66.,-16.8187489196813,2.48133693573106));
#59549=CARTESIAN_POINT('Ctrl Pts',(-50.,-16.8187489196813,2.48133693573106));
#59550=CARTESIAN_POINT('Ctrl Pts',(-66.,-16.7163331545329,2.52159914037693));
#59551=CARTESIAN_POINT('Ctrl Pts',(-50.,-16.7163331545329,2.52159914037693));
#59552=CARTESIAN_POINT('Ctrl Pts',(-66.,-16.6137791410988,2.56038555206031));
#59553=CARTESIAN_POINT('Ctrl Pts',(-50.,-16.6137791410988,2.56038555206031));
#59554=CARTESIAN_POINT('Ctrl Pts',(-66.,-16.511095838818,2.59770807109214));
#59555=CARTESIAN_POINT('Ctrl Pts',(-50.,-16.511095838818,2.59770807109214));
#59556=CARTESIAN_POINT('Ctrl Pts',(-66.,-16.408295837324,2.63356782519645));
#59557=CARTESIAN_POINT('Ctrl Pts',(-50.,-16.408295837324,2.63356782519645));
#59558=CARTESIAN_POINT('Ctrl Pts',(-66.,-16.3053960536831,2.66794389531189));
#59559=CARTESIAN_POINT('Ctrl Pts',(-50.,-16.3053960536831,2.66794389531189));
#59560=CARTESIAN_POINT('Ctrl Pts',(-66.,-16.2024181546768,2.70078418748721));
#59561=CARTESIAN_POINT('Ctrl Pts',(-50.,-16.2024181546768,2.70078418748721));
#59562=CARTESIAN_POINT('Ctrl Pts',(-66.,-16.099389766628,2.73199029450084));
#59563=CARTESIAN_POINT('Ctrl Pts',(-50.,-16.099389766628,2.73199029450084));
#59564=CARTESIAN_POINT('Ctrl Pts',(-66.,-15.9963411251835,2.76143959284173));
#59565=CARTESIAN_POINT('Ctrl Pts',(-50.,-15.9963411251835,2.76143959284173));
#59566=CARTESIAN_POINT('Ctrl Pts',(-66.,-15.8933006615651,2.78901652785862));
#59567=CARTESIAN_POINT('Ctrl Pts',(-50.,-15.8933006615651,2.78901652785862));
#59568=CARTESIAN_POINT('Ctrl Pts',(-66.,-15.7902905550528,2.81464355607623));
#59569=CARTESIAN_POINT('Ctrl Pts',(-50.,-15.7902905550528,2.81464355607623));
#59570=CARTESIAN_POINT('Ctrl Pts',(-66.,-15.6873231513416,2.83830684578773));
#59571=CARTESIAN_POINT('Ctrl Pts',(-50.,-15.6873231513416,2.83830684578773));
#59572=CARTESIAN_POINT('Ctrl Pts',(-66.,-15.5843947155558,2.86009946582377));
#59573=CARTESIAN_POINT('Ctrl Pts',(-50.,-15.5843947155558,2.86009946582377));
#59574=CARTESIAN_POINT('Ctrl Pts',(-66.,-15.4814936341966,2.88017005204204));
#59575=CARTESIAN_POINT('Ctrl Pts',(-50.,-15.4814936341966,2.88017005204204));
#59576=CARTESIAN_POINT('Ctrl Pts',(-66.,-15.3786133940255,2.89864026758367));
#59577=CARTESIAN_POINT('Ctrl Pts',(-50.,-15.3786133940255,2.89864026758367));
#59578=CARTESIAN_POINT('Ctrl Pts',(-66.,-15.2757647759192,2.91552760840775));
#59579=CARTESIAN_POINT('Ctrl Pts',(-50.,-15.2757647759192,2.91552760840775));
#59580=CARTESIAN_POINT('Ctrl Pts',(-66.,-15.1729867099492,2.9306770599819));
#59581=CARTESIAN_POINT('Ctrl Pts',(-50.,-15.1729867099492,2.9306770599819));
#59582=CARTESIAN_POINT('Ctrl Pts',(-66.,-15.0703622864763,2.94365932119071));
#59583=CARTESIAN_POINT('Ctrl Pts',(-50.,-15.0703622864763,2.94365932119071));
#59584=CARTESIAN_POINT('Ctrl Pts',(-66.,-14.9680056710645,2.95385868966535));
#59585=CARTESIAN_POINT('Ctrl Pts',(-50.,-14.9680056710645,2.95385868966535));
#59586=CARTESIAN_POINT('Ctrl Pts',(-66.,-14.8660391534142,2.96062511732634));
#59587=CARTESIAN_POINT('Ctrl Pts',(-50.,-14.8660391534142,2.96062511732634));
#59588=CARTESIAN_POINT('Ctrl Pts',(-66.,-14.7645727249416,2.96341047532946));
#59589=CARTESIAN_POINT('Ctrl Pts',(-50.,-14.7645727249416,2.96341047532946));
#59590=CARTESIAN_POINT('Ctrl Pts',(-66.,-14.6636842479405,2.96189992942649));
#59591=CARTESIAN_POINT('Ctrl Pts',(-50.,-14.6636842479405,2.96189992942649));
#59592=CARTESIAN_POINT('Ctrl Pts',(-66.,-14.5633947076351,2.95617854486928));
#59593=CARTESIAN_POINT('Ctrl Pts',(-50.,-14.5633947076351,2.95617854486928));
#59594=CARTESIAN_POINT('Ctrl Pts',(-66.,-14.463677848895,2.94665434795724));
#59595=CARTESIAN_POINT('Ctrl Pts',(-50.,-14.463677848895,2.94665434795724));
#59596=CARTESIAN_POINT('Ctrl Pts',(-66.,-14.3644786617177,2.93391890356181));
#59597=CARTESIAN_POINT('Ctrl Pts',(-50.,-14.3644786617177,2.93391890356181));
#59598=CARTESIAN_POINT('Ctrl Pts',(-66.,-14.2657288580852,2.91862876972314));
#59599=CARTESIAN_POINT('Ctrl Pts',(-50.,-14.2657288580852,2.91862876972314));
#59600=CARTESIAN_POINT('Ctrl Pts',(-66.,-14.1673628947312,2.90138362450613));
#59601=CARTESIAN_POINT('Ctrl Pts',(-50.,-14.1673628947312,2.90138362450613));
#59602=CARTESIAN_POINT('Ctrl Pts',(-66.,-14.0693351608341,2.882594172965));
#59603=CARTESIAN_POINT('Ctrl Pts',(-50.,-14.0693351608341,2.882594172965));
#59604=CARTESIAN_POINT('Ctrl Pts',(-66.,-13.9716176994713,2.862507481945));
#59605=CARTESIAN_POINT('Ctrl Pts',(-50.,-13.9716176994713,2.862507481945));
#59606=CARTESIAN_POINT('Ctrl Pts',(-66.,-13.8936799818437,2.84550248942744));
#59607=CARTESIAN_POINT('Ctrl Pts',(-50.,-13.8936799818437,2.84550248942744));
#59608=CARTESIAN_POINT('Ctrl Pts',(-66.,-13.8353570146283,2.83224277227946));
#59609=CARTESIAN_POINT('Ctrl Pts',(-50.,-13.8353570146283,2.83224277227946));
#59610=CARTESIAN_POINT('Ctrl Pts',(-66.,-13.7965328775753,2.82317840202614));
#59611=CARTESIAN_POINT('Ctrl Pts',(-50.,-13.7965328775753,2.82317840202614));
#59612=CARTESIAN_POINT('Ctrl Pts',(-66.,-13.7771352694631,2.81859007606939));
#59613=CARTESIAN_POINT('Ctrl Pts',(-50.,-13.7771352694631,2.81859007606939));
#59614=CARTESIAN_POINT('Origin',(-65.75,0.,0.));
#59615=CARTESIAN_POINT('',(-65.5,-15.5294395356693,6.60319110036901));
#59616=CARTESIAN_POINT('Origin',(-65.5,0.,0.));
#59617=CARTESIAN_POINT('Ctrl Pts',(-65.5,-15.5294395356693,6.60319110036901));
#59618=CARTESIAN_POINT('Ctrl Pts',(-65.6931595476704,-15.308937883882,6.62813354100189));
#59619=CARTESIAN_POINT('Ctrl Pts',(-65.8611256967045,-15.1198491095487,
6.6410048580703));
#59620=CARTESIAN_POINT('Ctrl Pts',(-66.,-14.9649893429273,6.64753480367511));
#59621=CARTESIAN_POINT('Origin',(-58.,0.,0.));
#59622=CARTESIAN_POINT('',(-50.5,-15.5294395356693,6.60319110036901));
#59623=CARTESIAN_POINT('Origin',(-50.5,0.,0.));
#59624=CARTESIAN_POINT('Ctrl Pts',(-50.5,-15.5294395356693,6.60319110036901));
#59625=CARTESIAN_POINT('Ctrl Pts',(-55.5,-15.5294395356693,6.60319110036901));
#59626=CARTESIAN_POINT('Ctrl Pts',(-60.5,-15.5294395356693,6.60319110036901));
#59627=CARTESIAN_POINT('Ctrl Pts',(-65.5,-15.5294395356693,6.60319110036901));
#59628=CARTESIAN_POINT('Origin',(-50.25,0.,0.));
#59629=CARTESIAN_POINT('Ctrl Pts',(-50.,-14.9649893429273,6.64753480367511));
#59630=CARTESIAN_POINT('Ctrl Pts',(-50.1388743032925,-15.1198491095454,
6.64100485807044));
#59631=CARTESIAN_POINT('Ctrl Pts',(-50.3068404523269,-15.3089378838789,
6.62813354100223));
#59632=CARTESIAN_POINT('Ctrl Pts',(-50.5,-15.5294395356693,6.60319110036901));
#59633=CARTESIAN_POINT('Ctrl Pts',(-66.,-11.9725570665522,7.37643433768309));
#59634=CARTESIAN_POINT('Ctrl Pts',(-50.,-11.9725570665522,7.37643433768309));
#59635=CARTESIAN_POINT('Ctrl Pts',(-66.,-11.9929426034861,7.38786606141889));
#59636=CARTESIAN_POINT('Ctrl Pts',(-50.,-11.9929426034861,7.38786606141889));
#59637=CARTESIAN_POINT('Ctrl Pts',(-66.,-12.0336116133124,7.4109301341784));
#59638=CARTESIAN_POINT('Ctrl Pts',(-50.,-12.0336116133124,7.4109301341784));
#59639=CARTESIAN_POINT('Ctrl Pts',(-66.,-12.0943089474566,7.44612811243127));
#59640=CARTESIAN_POINT('Ctrl Pts',(-50.,-12.0943089474566,7.44612811243127));
#59641=CARTESIAN_POINT('Ctrl Pts',(-66.,-12.174625451278,7.49426414725743));
#59642=CARTESIAN_POINT('Ctrl Pts',(-50.,-12.174625451278,7.49426414725743));
#59643=CARTESIAN_POINT('Ctrl Pts',(-66.,-12.2739577025182,7.5564825878338));
#59644=CARTESIAN_POINT('Ctrl Pts',(-50.,-12.2739577025182,7.5564825878338));
#59645=CARTESIAN_POINT('Ctrl Pts',(-66.,-12.3721090366891,7.62085266008235));
#59646=CARTESIAN_POINT('Ctrl Pts',(-50.,-12.3721090366891,7.62085266008235));
#59647=CARTESIAN_POINT('Ctrl Pts',(-66.,-12.4688535134548,7.68756697112423));
#59648=CARTESIAN_POINT('Ctrl Pts',(-50.,-12.4688535134548,7.68756697112423));
#59649=CARTESIAN_POINT('Ctrl Pts',(-66.,-12.5638109939272,7.75694076391353));
#59650=CARTESIAN_POINT('Ctrl Pts',(-50.,-12.5638109939272,7.75694076391353));
#59651=CARTESIAN_POINT('Ctrl Pts',(-66.,-12.6565110535803,7.82939076691323));
#59652=CARTESIAN_POINT('Ctrl Pts',(-50.,-12.6565110535803,7.82939076691323));
#59653=CARTESIAN_POINT('Ctrl Pts',(-66.,-12.7464782795223,7.9054109081407));
#59654=CARTESIAN_POINT('Ctrl Pts',(-50.,-12.7464782795223,7.9054109081407));
#59655=CARTESIAN_POINT('Ctrl Pts',(-66.,-12.8333072263957,7.98553702611316));
#59656=CARTESIAN_POINT('Ctrl Pts',(-50.,-12.8333072263957,7.98553702611316));
#59657=CARTESIAN_POINT('Ctrl Pts',(-66.,-12.9167494409123,8.07034649661759));
#59658=CARTESIAN_POINT('Ctrl Pts',(-50.,-12.9167494409123,8.07034649661759));
#59659=CARTESIAN_POINT('Ctrl Pts',(-66.,-12.9967646908729,8.16026752634251));
#59660=CARTESIAN_POINT('Ctrl Pts',(-50.,-12.9967646908729,8.16026752634251));
#59661=CARTESIAN_POINT('Ctrl Pts',(-66.,-13.0735719476516,8.2552497632047));
#59662=CARTESIAN_POINT('Ctrl Pts',(-50.,-13.0735719476516,8.2552497632047));
#59663=CARTESIAN_POINT('Ctrl Pts',(-66.,-13.1476766619554,8.35455196515643));
#59664=CARTESIAN_POINT('Ctrl Pts',(-50.,-13.1476766619554,8.35455196515643));
#59665=CARTESIAN_POINT('Ctrl Pts',(-66.,-13.2199692944164,8.45629920475326));
#59666=CARTESIAN_POINT('Ctrl Pts',(-50.,-13.2199692944164,8.45629920475326));
#59667=CARTESIAN_POINT('Ctrl Pts',(-66.,-13.2915701735423,8.557804399923));
#59668=CARTESIAN_POINT('Ctrl Pts',(-50.,-13.2915701735423,8.557804399923));
#59669=CARTESIAN_POINT('Ctrl Pts',(-66.,-13.3633320128944,8.65689099100683));
#59670=CARTESIAN_POINT('Ctrl Pts',(-50.,-13.3633320128944,8.65689099100683));
#59671=CARTESIAN_POINT('Ctrl Pts',(-66.,-13.4354725852278,8.7528532374933));
#59672=CARTESIAN_POINT('Ctrl Pts',(-50.,-13.4354725852278,8.7528532374933));
#59673=CARTESIAN_POINT('Ctrl Pts',(-66.,-13.5070556576137,8.84780971091874));
#59674=CARTESIAN_POINT('Ctrl Pts',(-50.,-13.5070556576137,8.84780971091874));
#59675=CARTESIAN_POINT('Ctrl Pts',(-66.,-13.5758183415752,8.9471865570421));
#59676=CARTESIAN_POINT('Ctrl Pts',(-50.,-13.5758183415752,8.9471865570421));
#59677=CARTESIAN_POINT('Ctrl Pts',(-66.,-13.6393985665122,9.0567109207601));
#59678=CARTESIAN_POINT('Ctrl Pts',(-50.,-13.6393985665122,9.0567109207601));
#59679=CARTESIAN_POINT('Ctrl Pts',(-66.,-13.6963879047689,9.17984080520628));
#59680=CARTESIAN_POINT('Ctrl Pts',(-50.,-13.6963879047689,9.17984080520628));
#59681=CARTESIAN_POINT('Ctrl Pts',(-66.,-13.7474046302415,9.31514187328191));
#59682=CARTESIAN_POINT('Ctrl Pts',(-50.,-13.7474046302415,9.31514187328191));
#59683=CARTESIAN_POINT('Ctrl Pts',(-66.,-13.7963063276482,9.4533268215348));
#59684=CARTESIAN_POINT('Ctrl Pts',(-50.,-13.7963063276482,9.4533268215348));
#59685=CARTESIAN_POINT('Ctrl Pts',(-66.,-13.8492525549383,9.57952542768277));
#59686=CARTESIAN_POINT('Ctrl Pts',(-50.,-13.8492525549383,9.57952542768277));
#59687=CARTESIAN_POINT('Ctrl Pts',(-66.,-13.9135130516827,9.67617398568753));
#59688=CARTESIAN_POINT('Ctrl Pts',(-50.,-13.9135130516827,9.67617398568753));
#59689=CARTESIAN_POINT('Ctrl Pts',(-66.,-13.9964541688655,9.72547191786523));
#59690=CARTESIAN_POINT('Ctrl Pts',(-50.,-13.9964541688655,9.72547191786523));
#59691=CARTESIAN_POINT('Ctrl Pts',(-66.,-14.1042598989495,9.71248252455659));
#59692=CARTESIAN_POINT('Ctrl Pts',(-50.,-14.1042598989495,9.71248252455659));
#59693=CARTESIAN_POINT('Ctrl Pts',(-66.,-14.2415877332851,9.62596662912619));
#59694=CARTESIAN_POINT('Ctrl Pts',(-50.,-14.2415877332851,9.62596662912619));
#59695=CARTESIAN_POINT('Ctrl Pts',(-66.,-14.4119109068994,9.45755182333451));
#59696=CARTESIAN_POINT('Ctrl Pts',(-50.,-14.4119109068994,9.45755182333451));
#59697=CARTESIAN_POINT('Ctrl Pts',(-66.,-14.6176527534638,9.20140599515898));
#59698=CARTESIAN_POINT('Ctrl Pts',(-50.,-14.6176527534638,9.20140599515898));
#59699=CARTESIAN_POINT('Ctrl Pts',(-66.,-14.8603967131463,8.85372752977427));
#59700=CARTESIAN_POINT('Ctrl Pts',(-50.,-14.8603967131463,8.85372752977427));
#59701=CARTESIAN_POINT('Ctrl Pts',(-66.,-15.1410546573881,8.41233672184739));
#59702=CARTESIAN_POINT('Ctrl Pts',(-50.,-15.1410546573881,8.41233672184739));
#59703=CARTESIAN_POINT('Ctrl Pts',(-66.,-15.4600447033794,7.87624429847578));
#59704=CARTESIAN_POINT('Ctrl Pts',(-50.,-15.4600447033794,7.87624429847578));
#59705=CARTESIAN_POINT('Ctrl Pts',(-66.,-15.7459748034105,7.37144760803722));
#59706=CARTESIAN_POINT('Ctrl Pts',(-50.,-15.7459748034105,7.37144760803722));
#59707=CARTESIAN_POINT('Ctrl Pts',(-66.,-15.9776798358492,6.95022755696745));
#59708=CARTESIAN_POINT('Ctrl Pts',(-50.,-15.9776798358492,6.95022755696745));
#59709=CARTESIAN_POINT('Ctrl Pts',(-66.,-16.1398096369224,6.65049603710921));
#59710=CARTESIAN_POINT('Ctrl Pts',(-50.,-16.1398096369224,6.65049603710921));
#59711=CARTESIAN_POINT('Ctrl Pts',(-66.,-16.2227894831771,6.49590073696634));
#59712=CARTESIAN_POINT('Ctrl Pts',(-50.,-16.2227894831771,6.49590073696634));
#59713=CARTESIAN_POINT('',(-65.5,-13.8729177747003,9.60769365750208));
#59714=CARTESIAN_POINT('Ctrl Pts',(-66.,-13.6388425130122,9.0621520570585));
#59715=CARTESIAN_POINT('Ctrl Pts',(-65.7933280154028,-13.7472614276904,
9.27242719182262));
#59716=CARTESIAN_POINT('Ctrl Pts',(-65.6370761749494,-13.7926957795761,
9.48276801426461));
#59717=CARTESIAN_POINT('Ctrl Pts',(-65.5,-13.8729177747003,9.60769365750208));
#59718=CARTESIAN_POINT('',(-66.,-11.9725570665522,7.37643433768309));
#59719=CARTESIAN_POINT('',(-50.5,-13.8729177747003,9.60769365750209));
#59720=CARTESIAN_POINT('Ctrl Pts',(-50.5,-13.8729177747003,9.60769365750208));
#59721=CARTESIAN_POINT('Ctrl Pts',(-50.4518618349123,-13.8447455584389,
9.56382249433257));
#59722=CARTESIAN_POINT('Ctrl Pts',(-50.4012423593885,-13.8206924223065,
9.50957310384971));
#59723=CARTESIAN_POINT('Ctrl Pts',(-50.2441129793801,-13.7511164514545,
9.33310335708368));
#59724=CARTESIAN_POINT('Ctrl Pts',(-50.1366827452943,-13.7105454819895,
9.20121774969557));
#59725=CARTESIAN_POINT('Ctrl Pts',(-50.,-13.6388425130122,9.0621520570585));
#59726=CARTESIAN_POINT('Ctrl Pts',(-65.5,-13.8729177747003,9.60769365750208));
#59727=CARTESIAN_POINT('Ctrl Pts',(-60.5,-13.8729177747003,9.60769365750208));
#59728=CARTESIAN_POINT('Ctrl Pts',(-55.5,-13.8729177747003,9.60769365750208));
#59729=CARTESIAN_POINT('Ctrl Pts',(-50.5,-13.8729177747003,9.60769365750208));
#59730=CARTESIAN_POINT('Origin',(-66.,0.,0.));
#59731=CARTESIAN_POINT('',(-66.,-12.6433463826116,6.15627310142281));
#59732=CARTESIAN_POINT('Ctrl Pts',(-66.,-16.2227894831771,6.49590073696634));
#59733=CARTESIAN_POINT('Ctrl Pts',(-50.,-16.2227894831771,6.49590073696634));
#59734=CARTESIAN_POINT('Ctrl Pts',(-66.,-16.2006994791252,6.50022537552599));
#59735=CARTESIAN_POINT('Ctrl Pts',(-50.,-16.2006994791252,6.50022537552599));
#59736=CARTESIAN_POINT('Ctrl Pts',(-66.,-16.156541644553,6.50872846327372));
#59737=CARTESIAN_POINT('Ctrl Pts',(-50.,-16.156541644553,6.50872846327372));
#59738=CARTESIAN_POINT('Ctrl Pts',(-66.,-16.0903714131301,6.52104452743828));
#59739=CARTESIAN_POINT('Ctrl Pts',(-50.,-16.0903714131301,6.52104452743828));
#59740=CARTESIAN_POINT('Ctrl Pts',(-66.,-16.0022776570719,6.53658763924282));
#59741=CARTESIAN_POINT('Ctrl Pts',(-50.,-16.0022776570719,6.53658763924282));
#59742=CARTESIAN_POINT('Ctrl Pts',(-66.,-15.8923837101016,6.55454673713648));
#59743=CARTESIAN_POINT('Ctrl Pts',(-50.,-15.8923837101016,6.55454673713648));
#59744=CARTESIAN_POINT('Ctrl Pts',(-66.,-15.7827148976515,6.57102989138234));
#59745=CARTESIAN_POINT('Ctrl Pts',(-50.,-15.7827148976515,6.57102989138234));
#59746=CARTESIAN_POINT('Ctrl Pts',(-66.,-15.6732735922887,6.58603394412518));
#59747=CARTESIAN_POINT('Ctrl Pts',(-50.,-15.6732735922887,6.58603394412518));
#59748=CARTESIAN_POINT('Ctrl Pts',(-66.,-15.5640626036015,6.59956147249643));
#59749=CARTESIAN_POINT('Ctrl Pts',(-50.,-15.5640626036015,6.59956147249643));
#59750=CARTESIAN_POINT('Ctrl Pts',(-66.,-15.4550847247379,6.61162519170432));
#59751=CARTESIAN_POINT('Ctrl Pts',(-50.,-15.4550847247379,6.61162519170432));
#59752=CARTESIAN_POINT('Ctrl Pts',(-66.,-15.346345674173,6.62223885631155));
#59753=CARTESIAN_POINT('Ctrl Pts',(-50.,-15.346345674173,6.62223885631155));
#59754=CARTESIAN_POINT('Ctrl Pts',(-66.,-15.2378573655599,6.63140668952709));
#59755=CARTESIAN_POINT('Ctrl Pts',(-50.,-15.2378573655599,6.63140668952709));
#59756=CARTESIAN_POINT('Ctrl Pts',(-66.,-15.1296413868434,6.63911263660376));
#59757=CARTESIAN_POINT('Ctrl Pts',(-50.,-15.1296413868434,6.63911263660376));
#59758=CARTESIAN_POINT('Ctrl Pts',(-66.,-15.021731679342,6.64531162852697));
#59759=CARTESIAN_POINT('Ctrl Pts',(-50.,-15.021731679342,6.64531162852697));
#59760=CARTESIAN_POINT('Ctrl Pts',(-66.,-14.9141794743276,6.64991522010611));
#59761=CARTESIAN_POINT('Ctrl Pts',(-50.,-14.9141794743276,6.64991522010611));
#59762=CARTESIAN_POINT('Ctrl Pts',(-66.,-14.8070445527658,6.65281215957283));
#59763=CARTESIAN_POINT('Ctrl Pts',(-50.,-14.8070445527658,6.65281215957283));
#59764=CARTESIAN_POINT('Ctrl Pts',(-66.,-14.7003831899324,6.65389759319505));
#59765=CARTESIAN_POINT('Ctrl Pts',(-50.,-14.7003831899324,6.65389759319505));
#59766=CARTESIAN_POINT('Ctrl Pts',(-66.,-14.5942361525827,6.65310192943101));
#59767=CARTESIAN_POINT('Ctrl Pts',(-50.,-14.5942361525827,6.65310192943101));
#59768=CARTESIAN_POINT('Ctrl Pts',(-66.,-14.4886188383546,6.65041484137187));
#59769=CARTESIAN_POINT('Ctrl Pts',(-50.,-14.4886188383546,6.65041484137187));
#59770=CARTESIAN_POINT('Ctrl Pts',(-66.,-14.3835044844334,6.64592554509403));
#59771=CARTESIAN_POINT('Ctrl Pts',(-50.,-14.3835044844334,6.64592554509403));
#59772=CARTESIAN_POINT('Ctrl Pts',(-66.,-14.278844877945,6.63977511862666));
#59773=CARTESIAN_POINT('Ctrl Pts',(-50.,-14.278844877945,6.63977511862666));
#59774=CARTESIAN_POINT('Ctrl Pts',(-66.,-14.1746034538834,6.63207978306306));
#59775=CARTESIAN_POINT('Ctrl Pts',(-50.,-14.1746034538834,6.63207978306306));
#59776=CARTESIAN_POINT('Ctrl Pts',(-66.,-14.0707863033563,6.6228591657896));
#59777=CARTESIAN_POINT('Ctrl Pts',(-50.,-14.0707863033563,6.6228591657896));
#59778=CARTESIAN_POINT('Ctrl Pts',(-66.,-13.9674696839217,6.61197280385553));
#59779=CARTESIAN_POINT('Ctrl Pts',(-50.,-13.9674696839217,6.61197280385553));
#59780=CARTESIAN_POINT('Ctrl Pts',(-66.,-13.8648408383502,6.59902554716193));
#59781=CARTESIAN_POINT('Ctrl Pts',(-50.,-13.8648408383502,6.59902554716193));
#59782=CARTESIAN_POINT('Ctrl Pts',(-66.,-13.7631634644371,6.58344942858329));
#59783=CARTESIAN_POINT('Ctrl Pts',(-50.,-13.7631634644371,6.58344942858329));
#59784=CARTESIAN_POINT('Ctrl Pts',(-66.,-13.6627176703106,6.56464523470766));
#59785=CARTESIAN_POINT('Ctrl Pts',(-50.,-13.6627176703106,6.56464523470766));
#59786=CARTESIAN_POINT('Ctrl Pts',(-66.,-13.5637463059047,6.54210941091933));
#59787=CARTESIAN_POINT('Ctrl Pts',(-50.,-13.5637463059047,6.54210941091933));
#59788=CARTESIAN_POINT('Ctrl Pts',(-66.,-13.4664030834197,6.51555637763196));
#59789=CARTESIAN_POINT('Ctrl Pts',(-50.,-13.4664030834197,6.51555637763196));
#59790=CARTESIAN_POINT('Ctrl Pts',(-66.,-13.3706871739224,6.48507374642914));
#59791=CARTESIAN_POINT('Ctrl Pts',(-50.,-13.3706871739224,6.48507374642914));
#59792=CARTESIAN_POINT('Ctrl Pts',(-66.,-13.2764716751216,6.45105019532836));
#59793=CARTESIAN_POINT('Ctrl Pts',(-50.,-13.2764716751216,6.45105019532836));
#59794=CARTESIAN_POINT('Ctrl Pts',(-66.,-13.1835561890537,6.41404502367149));
#59795=CARTESIAN_POINT('Ctrl Pts',(-50.,-13.1835561890537,6.41404502367149));
#59796=CARTESIAN_POINT('Ctrl Pts',(-66.,-13.0917112937495,6.37467717998103));
#59797=CARTESIAN_POINT('Ctrl Pts',(-50.,-13.0917112937495,6.37467717998103));
#59798=CARTESIAN_POINT('Ctrl Pts',(-66.,-13.0007243712348,6.33351120238525));
#59799=CARTESIAN_POINT('Ctrl Pts',(-50.,-13.0007243712348,6.33351120238525));
#59800=CARTESIAN_POINT('Ctrl Pts',(-66.,-12.9104491054422,6.29093354993378));
#59801=CARTESIAN_POINT('Ctrl Pts',(-50.,-12.9104491054422,6.29093354993378));
#59802=CARTESIAN_POINT('Ctrl Pts',(-66.,-12.8207969747412,6.24717657480866));
#59803=CARTESIAN_POINT('Ctrl Pts',(-50.,-12.8207969747412,6.24717657480866));
#59804=CARTESIAN_POINT('Ctrl Pts',(-66.,-12.7495367835008,6.21132350319834));
#59805=CARTESIAN_POINT('Ctrl Pts',(-50.,-12.7495367835008,6.21132350319834));
#59806=CARTESIAN_POINT('Ctrl Pts',(-66.,-12.6963436971102,6.18397603231157));
#59807=CARTESIAN_POINT('Ctrl Pts',(-50.,-12.6963436971102,6.18397603231157));
#59808=CARTESIAN_POINT('Ctrl Pts',(-66.,-12.6609935089309,6.16554126565498));
#59809=CARTESIAN_POINT('Ctrl Pts',(-50.,-12.6609935089309,6.16554126565498));
#59810=CARTESIAN_POINT('Ctrl Pts',(-66.,-12.6433463826116,6.1562731014228));
#59811=CARTESIAN_POINT('Ctrl Pts',(-50.,-12.6433463826116,6.1562731014228));
#59812=CARTESIAN_POINT('Origin',(-65.75,0.,0.));
#59813=CARTESIAN_POINT('',(-65.5,-13.3994067863357,10.2577542753909));
#59814=CARTESIAN_POINT('Origin',(-65.5,0.,0.));
#59815=CARTESIAN_POINT('Ctrl Pts',(-65.5,-13.3994067863357,10.2577542753909));
#59816=CARTESIAN_POINT('Ctrl Pts',(-65.6931595476697,-13.1796296666677,
10.2270765724828));
#59817=CARTESIAN_POINT('Ctrl Pts',(-65.8611256967046,-12.9932804974997,
10.1925190475036));
#59818=CARTESIAN_POINT('Ctrl Pts',(-66.,-12.8416620037784,10.1603317849721));
#59819=CARTESIAN_POINT('Origin',(-58.,0.,0.));
#59820=CARTESIAN_POINT('',(-50.5,-13.3994067863357,10.2577542753909));
#59821=CARTESIAN_POINT('Origin',(-50.5,0.,0.));
#59822=CARTESIAN_POINT('Ctrl Pts',(-50.5,-13.3994067863357,10.2577542753909));
#59823=CARTESIAN_POINT('Ctrl Pts',(-55.5,-13.3994067863357,10.2577542753909));
#59824=CARTESIAN_POINT('Ctrl Pts',(-60.5,-13.3994067863357,10.2577542753909));
#59825=CARTESIAN_POINT('Ctrl Pts',(-65.5,-13.3994067863357,10.2577542753909));
#59826=CARTESIAN_POINT('Origin',(-50.25,0.,0.));
#59827=CARTESIAN_POINT('Ctrl Pts',(-50.,-12.8416620037784,10.1603317849721));
#59828=CARTESIAN_POINT('Ctrl Pts',(-50.1388743032962,-12.9932804975006,
10.1925190475038));
#59829=CARTESIAN_POINT('Ctrl Pts',(-50.3068404523311,-13.1796296666686,
10.2270765724829));
#59830=CARTESIAN_POINT('Ctrl Pts',(-50.5,-13.3994067863357,10.2577542753909));
#59831=CARTESIAN_POINT('Ctrl Pts',(-66.,-9.76197254719673,10.1221439546065));
#59832=CARTESIAN_POINT('Ctrl Pts',(-50.,-9.76197254719673,10.1221439546065));
#59833=CARTESIAN_POINT('Ctrl Pts',(-66.,-9.77887468091545,10.1382862065996));
#59834=CARTESIAN_POINT('Ctrl Pts',(-50.,-9.77887468091545,10.1382862065996));
#59835=CARTESIAN_POINT('Ctrl Pts',(-66.,-9.8125301973609,10.1707396505663));
#59836=CARTESIAN_POINT('Ctrl Pts',(-50.,-9.8125301973609,10.1707396505663));
#59837=CARTESIAN_POINT('Ctrl Pts',(-66.,-9.86256723189823,10.2199266327873));
#59838=CARTESIAN_POINT('Ctrl Pts',(-50.,-9.86256723189823,10.2199266327873));
#59839=CARTESIAN_POINT('Ctrl Pts',(-66.,-9.92838949999087,10.2865242878363));
#59840=CARTESIAN_POINT('Ctrl Pts',(-50.,-9.92838949999087,10.2865242878363));
#59841=CARTESIAN_POINT('Ctrl Pts',(-66.,-10.0091279489326,10.371490948043));
#59842=CARTESIAN_POINT('Ctrl Pts',(-50.,-10.0091279489326,10.371490948043));
#59843=CARTESIAN_POINT('Ctrl Pts',(-66.,-10.0881874924486,10.4582479603236));
#59844=CARTESIAN_POINT('Ctrl Pts',(-50.,-10.0881874924486,10.4582479603236));
#59845=CARTESIAN_POINT('Ctrl Pts',(-66.,-10.1653013890907,10.5469256916157));
#59846=CARTESIAN_POINT('Ctrl Pts',(-50.,-10.1653013890907,10.5469256916157));
#59847=CARTESIAN_POINT('Ctrl Pts',(-66.,-10.2400230449985,10.6377349442392));
#59848=CARTESIAN_POINT('Ctrl Pts',(-50.,-10.2400230449985,10.6377349442392));
#59849=CARTESIAN_POINT('Ctrl Pts',(-66.,-10.3117931787431,10.7309623645438));
#59850=CARTESIAN_POINT('Ctrl Pts',(-50.,-10.3117931787431,10.7309623645438));
#59851=CARTESIAN_POINT('Ctrl Pts',(-66.,-10.3800284784999,10.8269681325114));
#59852=CARTESIAN_POINT('Ctrl Pts',(-50.,-10.3800284784999,10.8269681325114));
#59853=CARTESIAN_POINT('Ctrl Pts',(-66.,-10.4442029791024,10.9261704221467));
#59854=CARTESIAN_POINT('Ctrl Pts',(-50.,-10.4442029791024,10.9261704221467));
#59855=CARTESIAN_POINT('Ctrl Pts',(-66.,-10.5039324453602,11.0290666820944));
#59856=CARTESIAN_POINT('Ctrl Pts',(-50.,-10.5039324453602,11.0290666820944));
#59857=CARTESIAN_POINT('Ctrl Pts',(-66.,-10.5590714183695,11.1360616608015));
#59858=CARTESIAN_POINT('Ctrl Pts',(-50.,-10.5590714183695,11.1360616608015));
#59859=CARTESIAN_POINT('Ctrl Pts',(-66.,-10.6098445121699,11.2471610440543));
#59860=CARTESIAN_POINT('Ctrl Pts',(-50.,-10.6098445121699,11.2471610440543));
#59861=CARTESIAN_POINT('Ctrl Pts',(-66.,-10.6569256372063,11.3617725777663));
#59862=CARTESIAN_POINT('Ctrl Pts',(-50.,-10.6569256372063,11.3617725777663));
#59863=CARTESIAN_POINT('Ctrl Pts',(-66.,-10.7016435541469,11.4783016873407));
#59864=CARTESIAN_POINT('Ctrl Pts',(-50.,-10.7016435541469,11.4783016873407));
#59865=CARTESIAN_POINT('Ctrl Pts',(-66.,-10.7457516444569,11.5944243246999));
#59866=CARTESIAN_POINT('Ctrl Pts',(-50.,-10.7457516444569,11.5944243246999));
#59867=CARTESIAN_POINT('Ctrl Pts',(-66.,-10.7906171205087,11.7082443720486));
#59868=CARTESIAN_POINT('Ctrl Pts',(-50.,-10.7906171205087,11.7082443720486));
#59869=CARTESIAN_POINT('Ctrl Pts',(-66.,-10.8366264238543,11.819132418893));
#59870=CARTESIAN_POINT('Ctrl Pts',(-50.,-10.8366264238543,11.819132418893));
#59871=CARTESIAN_POINT('Ctrl Pts',(-66.,-10.8823458677273,11.9289076462876));
#59872=CARTESIAN_POINT('Ctrl Pts',(-50.,-10.8823458677273,11.9289076462876));
#59873=CARTESIAN_POINT('Ctrl Pts',(-66.,-10.9242342288773,12.0422629701643));
#59874=CARTESIAN_POINT('Ctrl Pts',(-50.,-10.9242342288773,12.0422629701643));
#59875=CARTESIAN_POINT('Ctrl Pts',(-66.,-10.9585793624772,12.1641581835604));
#59876=CARTESIAN_POINT('Ctrl Pts',(-50.,-10.9585793624772,12.1641581835604));
#59877=CARTESIAN_POINT('Ctrl Pts',(-66.,-10.983157118807,12.2975923883674));
#59878=CARTESIAN_POINT('Ctrl Pts',(-50.,-10.983157118807,12.2975923883674));
#59879=CARTESIAN_POINT('Ctrl Pts',(-66.,-10.9989230526826,12.4413300682894));
#59880=CARTESIAN_POINT('Ctrl Pts',(-50.,-10.9989230526826,12.4413300682894));
#59881=CARTESIAN_POINT('Ctrl Pts',(-66.,-11.0119232141524,12.5873350398988));
#59882=CARTESIAN_POINT('Ctrl Pts',(-50.,-11.0119232141524,12.5873350398988));
#59883=CARTESIAN_POINT('Ctrl Pts',(-66.,-11.0318217212277,12.7227360760623));
#59884=CARTESIAN_POINT('Ctrl Pts',(-50.,-11.0318217212277,12.7227360760623));
#59885=CARTESIAN_POINT('Ctrl Pts',(-66.,-11.0700278373151,12.8323291775776));
#59886=CARTESIAN_POINT('Ctrl Pts',(-50.,-11.0700278373151,12.8323291775776));
#59887=CARTESIAN_POINT('Ctrl Pts',(-66.,-11.1381033095929,12.9007049416369));
#59888=CARTESIAN_POINT('Ctrl Pts',(-50.,-11.1381033095929,12.9007049416369));
#59889=CARTESIAN_POINT('Ctrl Pts',(-66.,-11.2457524551817,12.9149338288552));
#59890=CARTESIAN_POINT('Ctrl Pts',(-50.,-11.2457524551817,12.9149338288552));
#59891=CARTESIAN_POINT('Ctrl Pts',(-66.,-11.400281511346,12.8652880329968));
#59892=CARTESIAN_POINT('Ctrl Pts',(-50.,-11.400281511346,12.8652880329968));
#59893=CARTESIAN_POINT('Ctrl Pts',(-66.,-11.607136728308,12.7445219388499));
#59894=CARTESIAN_POINT('Ctrl Pts',(-50.,-11.607136728308,12.7445219388499));
#59895=CARTESIAN_POINT('Ctrl Pts',(-66.,-11.8701156935365,12.547589319493));
#59896=CARTESIAN_POINT('Ctrl Pts',(-50.,-11.8701156935365,12.547589319493));
#59897=CARTESIAN_POINT('Ctrl Pts',(-66.,-12.1916975236769,12.2712017803777));
#59898=CARTESIAN_POINT('Ctrl Pts',(-50.,-12.1916975236769,12.2712017803777));
#59899=CARTESIAN_POINT('Ctrl Pts',(-66.,-12.5733075127254,11.9134748688282));
#59900=CARTESIAN_POINT('Ctrl Pts',(-50.,-12.5733075127254,11.9134748688282));
#59901=CARTESIAN_POINT('Ctrl Pts',(-66.,-13.0155966641184,11.4735543732861));
#59902=CARTESIAN_POINT('Ctrl Pts',(-50.,-13.0155966641184,11.4735543732861));
#59903=CARTESIAN_POINT('Ctrl Pts',(-66.,-13.4180815762547,11.0557247234476));
#59904=CARTESIAN_POINT('Ctrl Pts',(-50.,-13.4180815762547,11.0557247234476));
#59905=CARTESIAN_POINT('Ctrl Pts',(-66.,-13.7472603359957,10.7053607732244));
#59906=CARTESIAN_POINT('Ctrl Pts',(-50.,-13.7472603359957,10.7053607732244));
#59907=CARTESIAN_POINT('Ctrl Pts',(-66.,-13.9788367290857,10.4553659121651));
#59908=CARTESIAN_POINT('Ctrl Pts',(-50.,-13.9788367290857,10.4553659121651));
#59909=CARTESIAN_POINT('Ctrl Pts',(-66.,-14.0976558986297,10.3262637562592));
#59910=CARTESIAN_POINT('Ctrl Pts',(-50.,-14.0976558986297,10.3262637562592));
#59911=CARTESIAN_POINT('',(-65.5,-11.0477383006981,12.7559046499764));
#59912=CARTESIAN_POINT('Ctrl Pts',(-66.,-10.9566876228483,12.1692900916743));
#59913=CARTESIAN_POINT('Ctrl Pts',(-65.7933280154032,-11.0094070584153,
12.3999217340683));
#59914=CARTESIAN_POINT('Ctrl Pts',(-65.6370761749493,-11.0011043711894,
12.6149533766279));
#59915=CARTESIAN_POINT('Ctrl Pts',(-65.5,-11.0477383006981,12.7559046499764));
#59916=CARTESIAN_POINT('',(-66.,-9.76197254719673,10.1221439546065));
#59917=CARTESIAN_POINT('',(-50.5,-11.0477383006981,12.7559046499764));
#59918=CARTESIAN_POINT('Ctrl Pts',(-50.5,-11.0477383006981,12.7559046499764));
#59919=CARTESIAN_POINT('Ctrl Pts',(-50.4518618349123,-11.0313614810341,
12.706405634788));
#59920=CARTESIAN_POINT('Ctrl Pts',(-50.4012423593886,-11.0215552932018,
12.6478788169541));
#59921=CARTESIAN_POINT('Ctrl Pts',(-50.2441129793802,-10.9980514208266,
12.4596503514474));
#59922=CARTESIAN_POINT('Ctrl Pts',(-50.1366827452942,-10.9915536797922,
12.3218185831175));
#59923=CARTESIAN_POINT('Ctrl Pts',(-50.,-10.9566876228483,12.1692900916743));
#59924=CARTESIAN_POINT('Ctrl Pts',(-65.5,-11.0477383006981,12.7559046499764));
#59925=CARTESIAN_POINT('Ctrl Pts',(-60.5,-11.0477383006981,12.7559046499764));
#59926=CARTESIAN_POINT('Ctrl Pts',(-55.5,-11.0477383006981,12.7559046499764));
#59927=CARTESIAN_POINT('Ctrl Pts',(-50.5,-11.0477383006981,12.7559046499764));
#59928=CARTESIAN_POINT('Origin',(-66.,0.,0.));
#59929=CARTESIAN_POINT('',(-66.,-10.7151295435653,9.10713484662512));
#59930=CARTESIAN_POINT('Ctrl Pts',(-66.,-14.0976558986297,10.3262637562592));
#59931=CARTESIAN_POINT('Ctrl Pts',(-50.,-14.0976558986297,10.3262637562592));
#59932=CARTESIAN_POINT('Ctrl Pts',(-66.,-14.0751843988004,10.3249589677309));
#59933=CARTESIAN_POINT('Ctrl Pts',(-50.,-14.0751843988004,10.3249589677309));
#59934=CARTESIAN_POINT('Ctrl Pts',(-66.,-14.0302992318693,10.3222133084437));
#59935=CARTESIAN_POINT('Ctrl Pts',(-50.,-14.0302992318693,10.3222133084437));
#59936=CARTESIAN_POINT('Ctrl Pts',(-66.,-13.9631449793377,10.3176865734186));
#59937=CARTESIAN_POINT('Ctrl Pts',(-50.,-13.9631449793377,10.3176865734186));
#59938=CARTESIAN_POINT('Ctrl Pts',(-66.,-13.8739534358983,10.31083334353));
#59939=CARTESIAN_POINT('Ctrl Pts',(-50.,-13.8739534358983,10.31083334353));
#59940=CARTESIAN_POINT('Ctrl Pts',(-66.,-13.7630457633241,10.3008987100667));
#59941=CARTESIAN_POINT('Ctrl Pts',(-50.,-13.7630457633241,10.3008987100667));
#59942=CARTESIAN_POINT('Ctrl Pts',(-66.,-13.6527232045145,10.2895904911179));
#59943=CARTESIAN_POINT('Ctrl Pts',(-50.,-13.6527232045145,10.2895904911179));
#59944=CARTESIAN_POINT('Ctrl Pts',(-66.,-13.5429888428245,10.2769062180714));
#59945=CARTESIAN_POINT('Ctrl Pts',(-50.,-13.5429888428245,10.2769062180714));
#59946=CARTESIAN_POINT('Ctrl Pts',(-66.,-13.4338447586676,10.2628490858097));
#59947=CARTESIAN_POINT('Ctrl Pts',(-50.,-13.4338447586676,10.2628490858097));
#59948=CARTESIAN_POINT('Ctrl Pts',(-66.,-13.3252904952962,10.247432104697));
#59949=CARTESIAN_POINT('Ctrl Pts',(-50.,-13.3252904952962,10.247432104697));
#59950=CARTESIAN_POINT('Ctrl Pts',(-66.,-13.2173281709084,10.230670019298));
#59951=CARTESIAN_POINT('Ctrl Pts',(-50.,-13.2173281709084,10.230670019298));
#59952=CARTESIAN_POINT('Ctrl Pts',(-66.,-13.1099682745984,10.2125698829469));
#59953=CARTESIAN_POINT('Ctrl Pts',(-50.,-13.1099682745984,10.2125698829469));
#59954=CARTESIAN_POINT('Ctrl Pts',(-66.,-13.0032357087396,10.1931215139895));
#59955=CARTESIAN_POINT('Ctrl Pts',(-50.,-13.0032357087396,10.1931215139895));
#59956=CARTESIAN_POINT('Ctrl Pts',(-66.,-12.8971745565295,10.1722897001998));
#59957=CARTESIAN_POINT('Ctrl Pts',(-50.,-12.8971745565295,10.1722897001998));
#59958=CARTESIAN_POINT('Ctrl Pts',(-66.,-12.7918564351399,10.1500015157547));
#59959=CARTESIAN_POINT('Ctrl Pts',(-50.,-12.7918564351399,10.1500015157547));
#59960=CARTESIAN_POINT('Ctrl Pts',(-66.,-12.6873669145973,10.1261640709864));
#59961=CARTESIAN_POINT('Ctrl Pts',(-50.,-12.6873669145973,10.1261640709864));
#59962=CARTESIAN_POINT('Ctrl Pts',(-66.,-12.5837865782488,10.1006898014275));
#59963=CARTESIAN_POINT('Ctrl Pts',(-50.,-12.5837865782488,10.1006898014275));
#59964=CARTESIAN_POINT('Ctrl Pts',(-66.,-12.4811722187999,10.0735214401623));
#59965=CARTESIAN_POINT('Ctrl Pts',(-50.,-12.4811722187999,10.0735214401623));
#59966=CARTESIAN_POINT('Ctrl Pts',(-66.,-12.3795413183411,10.0446528139577));
#59967=CARTESIAN_POINT('Ctrl Pts',(-50.,-12.3795413183411,10.0446528139577));
#59968=CARTESIAN_POINT('Ctrl Pts',(-66.,-12.2788457677249,10.0141636803616));
#59969=CARTESIAN_POINT('Ctrl Pts',(-50.,-12.2788457677249,10.0141636803616));
#59970=CARTESIAN_POINT('Ctrl Pts',(-66.,-12.179003784094,9.98217869512325));
#59971=CARTESIAN_POINT('Ctrl Pts',(-50.,-12.179003784094,9.98217869512325));
#59972=CARTESIAN_POINT('Ctrl Pts',(-66.,-12.079951048189,9.94880133468933));
#59973=CARTESIAN_POINT('Ctrl Pts',(-50.,-12.079951048189,9.94880133468933));
#59974=CARTESIAN_POINT('Ctrl Pts',(-66.,-11.9816885786214,9.91405212461268));
#59975=CARTESIAN_POINT('Ctrl Pts',(-50.,-11.9816885786214,9.91405212461268));
#59976=CARTESIAN_POINT('Ctrl Pts',(-66.,-11.8843251688933,9.87781397932795));
#59977=CARTESIAN_POINT('Ctrl Pts',(-50.,-11.8843251688933,9.87781397932795));
#59978=CARTESIAN_POINT('Ctrl Pts',(-66.,-11.7881404490329,9.83975072848667));
#59979=CARTESIAN_POINT('Ctrl Pts',(-50.,-11.7881404490329,9.83975072848667));
#59980=CARTESIAN_POINT('Ctrl Pts',(-66.,-11.6935310799647,9.79937782767));
#59981=CARTESIAN_POINT('Ctrl Pts',(-50.,-11.6935310799647,9.79937782767));
#59982=CARTESIAN_POINT('Ctrl Pts',(-66.,-11.6009173880207,9.75618454891596));
#59983=CARTESIAN_POINT('Ctrl Pts',(-50.,-11.6009173880207,9.75618454891596));
#59984=CARTESIAN_POINT('Ctrl Pts',(-66.,-11.5106598224983,9.70974355202577));
#59985=CARTESIAN_POINT('Ctrl Pts',(-50.,-11.5106598224983,9.70974355202577));
#59986=CARTESIAN_POINT('Ctrl Pts',(-66.,-11.4229782872014,9.65981645609066));
#59987=CARTESIAN_POINT('Ctrl Pts',(-50.,-11.4229782872014,9.65981645609066));
#59988=CARTESIAN_POINT('Ctrl Pts',(-66.,-11.3378501911246,9.60648791406797));
#59989=CARTESIAN_POINT('Ctrl Pts',(-50.,-11.3378501911246,9.60648791406797));
#59990=CARTESIAN_POINT('Ctrl Pts',(-66.,-11.255055958553,9.55010283362399));
#59991=CARTESIAN_POINT('Ctrl Pts',(-50.,-11.255055958553,9.55010283362399));
#59992=CARTESIAN_POINT('Ctrl Pts',(-66.,-11.1742623953034,9.49115310573639));
#59993=CARTESIAN_POINT('Ctrl Pts',(-50.,-11.1742623953034,9.49115310573639));
#59994=CARTESIAN_POINT('Ctrl Pts',(-66.,-11.0950933608815,9.43018117859799));
#59995=CARTESIAN_POINT('Ctrl Pts',(-50.,-11.0950933608815,9.43018117859799));
#59996=CARTESIAN_POINT('Ctrl Pts',(-66.,-11.0172025221741,9.36768097839366));
#59997=CARTESIAN_POINT('Ctrl Pts',(-50.,-11.0172025221741,9.36768097839366));
#59998=CARTESIAN_POINT('Ctrl Pts',(-66.,-10.9403520514449,9.30399043552504));
#59999=CARTESIAN_POINT('Ctrl Pts',(-50.,-10.9403520514449,9.30399043552504));
#60000=CARTESIAN_POINT('Ctrl Pts',(-66.,-10.8643984244951,9.23931258796881));
#60001=CARTESIAN_POINT('Ctrl Pts',(-50.,-10.8643984244951,9.23931258796881));
#60002=CARTESIAN_POINT('Ctrl Pts',(-66.,-10.8042932995341,9.18686421761339));
#60003=CARTESIAN_POINT('Ctrl Pts',(-50.,-10.8042932995341,9.18686421761339));
#60004=CARTESIAN_POINT('Ctrl Pts',(-66.,-10.7595724112169,9.14714733516059));
#60005=CARTESIAN_POINT('Ctrl Pts',(-50.,-10.7595724112169,9.14714733516059));
#60006=CARTESIAN_POINT('Ctrl Pts',(-66.,-10.7299173542433,9.1205004962881));
#60007=CARTESIAN_POINT('Ctrl Pts',(-50.,-10.7299173542433,9.1205004962881));
#60008=CARTESIAN_POINT('Ctrl Pts',(-66.,-10.7151295435653,9.10713484662511));
#60009=CARTESIAN_POINT('Ctrl Pts',(-50.,-10.7151295435653,9.10713484662511));
#60010=CARTESIAN_POINT('Origin',(-65.75,0.,0.));
#60011=CARTESIAN_POINT('',(-65.5,-10.4274400290457,13.2677850239087));
#60012=CARTESIAN_POINT('Origin',(-65.5,0.,0.));
#60013=CARTESIAN_POINT('Ctrl Pts',(-65.5,-10.4274400290457,13.2677850239087));
#60014=CARTESIAN_POINT('Ctrl Pts',(-65.6931595476722,-10.222196846206,13.183414770357));
#60015=CARTESIAN_POINT('Ctrl Pts',(-65.861125696707,-10.0502962858477,13.1035997797182));
#60016=CARTESIAN_POINT('Ctrl Pts',(-66.,-9.91144581260293,13.0347177531328));
#60017=CARTESIAN_POINT('Origin',(-58.,0.,0.));
#60018=CARTESIAN_POINT('',(-50.5,-10.4274400290457,13.2677850239087));
#60019=CARTESIAN_POINT('Origin',(-50.5,0.,0.));
#60020=CARTESIAN_POINT('Ctrl Pts',(-50.5,-10.4274400290457,13.2677850239087));
#60021=CARTESIAN_POINT('Ctrl Pts',(-55.5,-10.4274400290457,13.2677850239087));
#60022=CARTESIAN_POINT('Ctrl Pts',(-60.5,-10.4274400290457,13.2677850239087));
#60023=CARTESIAN_POINT('Ctrl Pts',(-65.5,-10.4274400290457,13.2677850239087));
#60024=CARTESIAN_POINT('Origin',(-50.25,0.,0.));
#60025=CARTESIAN_POINT('Ctrl Pts',(-50.,-9.91144581260292,13.0347177531328));
#60026=CARTESIAN_POINT('Ctrl Pts',(-50.1388743032951,-10.0502962858498,
13.1035997797192));
#60027=CARTESIAN_POINT('Ctrl Pts',(-50.3068404523279,-10.2221968462061,
13.1834147703571));
#60028=CARTESIAN_POINT('Ctrl Pts',(-50.5,-10.4274400290457,13.2677850239087));
#60029=CARTESIAN_POINT('Ctrl Pts',(-66.,-6.93800739067721,12.2318420402206));
#60030=CARTESIAN_POINT('Ctrl Pts',(-50.,-6.93800739067721,12.2318420402206));
#60031=CARTESIAN_POINT('Ctrl Pts',(-66.,-6.95036409795758,12.2516805434111));
#60032=CARTESIAN_POINT('Ctrl Pts',(-50.,-6.95036409795758,12.2516805434111));
#60033=CARTESIAN_POINT('Ctrl Pts',(-66.,-6.97489142114752,12.2914841893452));
#60034=CARTESIAN_POINT('Ctrl Pts',(-50.,-6.97489142114752,12.2914841893452));
#60035=CARTESIAN_POINT('Ctrl Pts',(-66.,-7.01112414517467,12.3515695765444));
#60036=CARTESIAN_POINT('Ctrl Pts',(-50.,-7.01112414517467,12.3515695765444));
#60037=CARTESIAN_POINT('Ctrl Pts',(-66.,-7.05831632235693,12.4324442762203));
#60038=CARTESIAN_POINT('Ctrl Pts',(-50.,-7.05831632235693,12.4324442762203));
#60039=CARTESIAN_POINT('Ctrl Pts',(-66.,-7.11538787531798,12.5348203883111));
#60040=CARTESIAN_POINT('Ctrl Pts',(-50.,-7.11538787531798,12.5348203883111));
#60041=CARTESIAN_POINT('Ctrl Pts',(-66.,-7.17038802629925,12.6385130784722));
#60042=CARTESIAN_POINT('Ctrl Pts',(-50.,-7.17038802629925,12.6385130784722));
#60043=CARTESIAN_POINT('Ctrl Pts',(-66.,-7.22302599308674,12.7435822820237));
#60044=CARTESIAN_POINT('Ctrl Pts',(-50.,-7.22302599308674,12.7435822820237));
#60045=CARTESIAN_POINT('Ctrl Pts',(-66.,-7.27281678798223,12.8501211151659));
#60046=CARTESIAN_POINT('Ctrl Pts',(-50.,-7.27281678798223,12.8501211151659));
#60047=CARTESIAN_POINT('Ctrl Pts',(-66.,-7.31914741436296,12.9582681310911));
#60048=CARTESIAN_POINT('Ctrl Pts',(-50.,-7.31914741436296,12.9582681310911));
#60049=CARTESIAN_POINT('Ctrl Pts',(-66.,-7.36136331309888,13.0682271303129));
#60050=CARTESIAN_POINT('Ctrl Pts',(-50.,-7.36136331309888,13.0682271303129));
#60051=CARTESIAN_POINT('Ctrl Pts',(-66.,-7.39885104754049,13.1802723469128));
#60052=CARTESIAN_POINT('Ctrl Pts',(-50.,-7.39885104754049,13.1802723469128));
#60053=CARTESIAN_POINT('Ctrl Pts',(-66.,-7.43111474350486,13.2947900458654));
#60054=CARTESIAN_POINT('Ctrl Pts',(-50.,-7.43111474350486,13.2947900458654));
#60055=CARTESIAN_POINT('Ctrl Pts',(-66.,-7.45791285510172,13.4121360855424));
#60056=CARTESIAN_POINT('Ctrl Pts',(-50.,-7.45791285510172,13.4121360855424));
#60057=CARTESIAN_POINT('Ctrl Pts',(-66.,-7.47946152571002,13.5323718323411));
#60058=CARTESIAN_POINT('Ctrl Pts',(-50.,-7.47946152571002,13.5323718323411));
#60059=CARTESIAN_POINT('Ctrl Pts',(-66.,-7.49656078124055,13.6550912336386));
#60060=CARTESIAN_POINT('Ctrl Pts',(-50.,-7.49656078124055,13.6550912336386));
#60061=CARTESIAN_POINT('Ctrl Pts',(-66.,-7.51089419147856,13.7790802606718));
#60062=CARTESIAN_POINT('Ctrl Pts',(-50.,-7.51089419147856,13.7790802606718));
#60063=CARTESIAN_POINT('Ctrl Pts',(-66.,-7.52473801944021,13.9025239278461));
#60064=CARTESIAN_POINT('Ctrl Pts',(-50.,-7.52473801944021,13.9025239278461));
#60065=CARTESIAN_POINT('Ctrl Pts',(-66.,-7.53988806932779,14.0239256992838));
#60066=CARTESIAN_POINT('Ctrl Pts',(-50.,-7.53988806932779,14.0239256992838));
#60067=CARTESIAN_POINT('Ctrl Pts',(-66.,-7.55687516994583,14.1427720426853));
#60068=CARTESIAN_POINT('Ctrl Pts',(-50.,-7.55687516994583,14.1427720426853));
#60069=CARTESIAN_POINT('Ctrl Pts',(-66.,-7.5738582645032,14.2604684427868));
#60070=CARTESIAN_POINT('Ctrl Pts',(-50.,-7.5738582645032,14.2604684427868));
#60071=CARTESIAN_POINT('Ctrl Pts',(-66.,-7.58624030305585,14.380679712526));
#60072=CARTESIAN_POINT('Ctrl Pts',(-50.,-7.58624030305585,14.380679712526));
#60073=CARTESIAN_POINT('Ctrl Pts',(-66.,-7.58919231426205,14.5072866510432));
#60074=CARTESIAN_POINT('Ctrl Pts',(-50.,-7.58919231426205,14.5072866510432));
#60075=CARTESIAN_POINT('Ctrl Pts',(-66.,-7.57981417784402,14.6426410143862));
#60076=CARTESIAN_POINT('Ctrl Pts',(-50.,-7.57981417784402,14.6426410143862));
#60077=CARTESIAN_POINT('Ctrl Pts',(-66.,-7.55933868851428,14.785783739095));
#60078=CARTESIAN_POINT('Ctrl Pts',(-50.,-7.55933868851428,14.785783739095));
#60079=CARTESIAN_POINT('Ctrl Pts',(-66.,-7.53562046609085,14.930434704726));
#60080=CARTESIAN_POINT('Ctrl Pts',(-50.,-7.53562046609085,14.930434704726));
#60081=CARTESIAN_POINT('Ctrl Pts',(-66.,-7.52122095657002,15.0665304258326));
#60082=CARTESIAN_POINT('Ctrl Pts',(-50.,-7.52122095657002,15.0665304258326));
#60083=CARTESIAN_POINT('Ctrl Pts',(-66.,-7.53097206121459,15.1821819332349));
#60084=CARTESIAN_POINT('Ctrl Pts',(-50.,-7.53097206121459,15.1821819332349));
#60085=CARTESIAN_POINT('Ctrl Pts',(-66.,-7.57990445630002,15.2653392284515));
#60086=CARTESIAN_POINT('Ctrl Pts',(-50.,-7.57990445630002,15.2653392284515));
#60087=CARTESIAN_POINT('Ctrl Pts',(-66.,-7.68063302567044,15.3058923428827));
#60088=CARTESIAN_POINT('Ctrl Pts',(-50.,-7.68063302567044,15.3058923428827));
#60089=CARTESIAN_POINT('Ctrl Pts',(-66.,-7.84265367474648,15.2962360745346));
#60090=CARTESIAN_POINT('Ctrl Pts',(-50.,-7.84265367474648,15.2962360745346));
#60091=CARTESIAN_POINT('Ctrl Pts',(-66.,-8.07304346101417,15.2307068698744));
#60092=CARTESIAN_POINT('Ctrl Pts',(-50.,-8.07304346101417,15.2307068698744));
#60093=CARTESIAN_POINT('Ctrl Pts',(-66.,-8.37673560935255,15.1053614600777));
#60094=CARTESIAN_POINT('Ctrl Pts',(-50.,-8.37673560935255,15.1053614600777));
#60095=CARTESIAN_POINT('Ctrl Pts',(-66.,-8.75694914086774,14.9176312927967));
#60096=CARTESIAN_POINT('Ctrl Pts',(-50.,-8.75694914086774,14.9176312927967));
#60097=CARTESIAN_POINT('Ctrl Pts',(-66.,-9.2155332156477,14.6660455751048));
#60098=CARTESIAN_POINT('Ctrl Pts',(-50.,-9.2155332156477,14.6660455751048));
#60099=CARTESIAN_POINT('Ctrl Pts',(-66.,-9.75333081843477,14.3499388300415));
#60100=CARTESIAN_POINT('Ctrl Pts',(-50.,-9.75333081843477,14.3499388300415));
#60101=CARTESIAN_POINT('Ctrl Pts',(-66.,-10.2470809354107,14.0453299943724));
#60102=CARTESIAN_POINT('Ctrl Pts',(-50.,-10.2470809354107,14.0453299943724));
#60103=CARTESIAN_POINT('Ctrl Pts',(-66.,-10.6530499103448,13.7878368005368));
#60104=CARTESIAN_POINT('Ctrl Pts',(-50.,-10.6530499103448,13.7878368005368));
#60105=CARTESIAN_POINT('Ctrl Pts',(-66.,-10.9395220989952,13.6032866948137));
#60106=CARTESIAN_POINT('Ctrl Pts',(-50.,-10.9395220989952,13.6032866948137));
#60107=CARTESIAN_POINT('Ctrl Pts',(-66.,-11.0867147464198,13.5077896464047));
#60108=CARTESIAN_POINT('Ctrl Pts',(-50.,-11.0867147464198,13.5077896464047));
#60109=CARTESIAN_POINT('',(-65.5,-7.52838879852371,15.102615240357));
#60110=CARTESIAN_POINT('Ctrl Pts',(-66.,-7.58608375346252,14.5117868743119));
#60111=CARTESIAN_POINT('Ctrl Pts',(-65.793328015403,-7.57979115389329,14.748283590041));
#60112=CARTESIAN_POINT('Ctrl Pts',(-65.6370761749494,-7.51827311592916,
14.9544948237843));
#60113=CARTESIAN_POINT('Ctrl Pts',(-65.5,-7.52838879852371,15.102615240357));
#60114=CARTESIAN_POINT('',(-66.,-6.93800739067721,12.2318420402206));
#60115=CARTESIAN_POINT('',(-50.5,-7.52838879852371,15.102615240357));
#60116=CARTESIAN_POINT('Ctrl Pts',(-50.5,-7.52838879852371,15.102615240357));
#60117=CARTESIAN_POINT('Ctrl Pts',(-50.4518618349125,-7.5248363912663,15.050598578319));
#60118=CARTESIAN_POINT('Ctrl Pts',(-50.401242359389,-7.52989331058026,14.9914717883454));
#60119=CARTESIAN_POINT('Ctrl Pts',(-50.2441129793808,-7.55393837142435,
14.8033116908419));
#60120=CARTESIAN_POINT('Ctrl Pts',(-50.1366827452945,-7.58192213578687,
14.6681942384838));
#60121=CARTESIAN_POINT('Ctrl Pts',(-50.,-7.58608375346252,14.5117868743119));
#60122=CARTESIAN_POINT('Ctrl Pts',(-65.5,-7.52838879852371,15.102615240357));
#60123=CARTESIAN_POINT('Ctrl Pts',(-60.5,-7.52838879852371,15.102615240357));
#60124=CARTESIAN_POINT('Ctrl Pts',(-55.5,-7.52838879852371,15.102615240357));
#60125=CARTESIAN_POINT('Ctrl Pts',(-50.5,-7.52838879852371,15.102615240357));
#60126=CARTESIAN_POINT('Origin',(-66.,0.,0.));
#60127=CARTESIAN_POINT('',(-66.,-8.11364170780697,11.4857618157149));
#60128=CARTESIAN_POINT('Ctrl Pts',(-66.,-11.0867147464198,13.5077896464047));
#60129=CARTESIAN_POINT('Ctrl Pts',(-50.,-11.0867147464198,13.5077896464047));
#60130=CARTESIAN_POINT('Ctrl Pts',(-66.,-11.0652737177917,13.5009374154504));
#60131=CARTESIAN_POINT('Ctrl Pts',(-50.,-11.0652737177917,13.5009374154504));
#60132=CARTESIAN_POINT('Ctrl Pts',(-66.,-11.0224815186161,13.4871155289992));
#60133=CARTESIAN_POINT('Ctrl Pts',(-50.,-11.0224815186161,13.4871155289992));
#60134=CARTESIAN_POINT('Ctrl Pts',(-66.,-10.9585627936384,13.4660304261943));
#60135=CARTESIAN_POINT('Ctrl Pts',(-50.,-10.9585627936384,13.4660304261943));
#60136=CARTESIAN_POINT('Ctrl Pts',(-66.,-10.8738776955157,13.4372114682508));
#60137=CARTESIAN_POINT('Ctrl Pts',(-50.,-10.8738776955157,13.4372114682508));
#60138=CARTESIAN_POINT('Ctrl Pts',(-66.,-10.7689250342954,13.4000073329881));
#60139=CARTESIAN_POINT('Ctrl Pts',(-50.,-10.7689250342954,13.4000073329881));
#60140=CARTESIAN_POINT('Ctrl Pts',(-66.,-10.6648807012342,13.3616182778297));
#60141=CARTESIAN_POINT('Ctrl Pts',(-50.,-10.6648807012342,13.3616182778297));
#60142=CARTESIAN_POINT('Ctrl Pts',(-66.,-10.5617482967368,13.322042678519));
#60143=CARTESIAN_POINT('Ctrl Pts',(-50.,-10.5617482967368,13.322042678519));
#60144=CARTESIAN_POINT('Ctrl Pts',(-66.,-10.4595290413216,13.2812841469428));
#60145=CARTESIAN_POINT('Ctrl Pts',(-50.,-10.4595290413216,13.2812841469428));
#60146=CARTESIAN_POINT('Ctrl Pts',(-66.,-10.3582192570447,13.2393551711326));
#60147=CARTESIAN_POINT('Ctrl Pts',(-50.,-10.3582192570447,13.2393551711326));
#60148=CARTESIAN_POINT('Ctrl Pts',(-66.,-10.2578173287328,13.1962705591997));
#60149=CARTESIAN_POINT('Ctrl Pts',(-50.,-10.2578173287328,13.1962705591997));
#60150=CARTESIAN_POINT('Ctrl Pts',(-66.,-10.1583316618534,13.1520397514165));
#60151=CARTESIAN_POINT('Ctrl Pts',(-50.,-10.1583316618534,13.1520397514165));
#60152=CARTESIAN_POINT('Ctrl Pts',(-66.,-10.0597889085,13.1066590789727));
#60153=CARTESIAN_POINT('Ctrl Pts',(-50.,-10.0597889085,13.1066590789727));
#60154=CARTESIAN_POINT('Ctrl Pts',(-66.,-9.9622405238402,13.0601053989445));
#60155=CARTESIAN_POINT('Ctrl Pts',(-50.,-9.9622405238402,13.0601053989445));
#60156=CARTESIAN_POINT('Ctrl Pts',(-66.,-9.86577401097532,13.012325887074));
#60157=CARTESIAN_POINT('Ctrl Pts',(-50.,-9.86577401097532,13.012325887074));
#60158=CARTESIAN_POINT('Ctrl Pts',(-66.,-9.77049535231301,12.9632518523934));
#60159=CARTESIAN_POINT('Ctrl Pts',(-50.,-9.77049535231301,12.9632518523934));
#60160=CARTESIAN_POINT('Ctrl Pts',(-66.,-9.67650437592402,12.9128185216976));
#60161=CARTESIAN_POINT('Ctrl Pts',(-50.,-9.67650437592402,12.9128185216976));
#60162=CARTESIAN_POINT('Ctrl Pts',(-66.,-9.58387033196931,12.8609845509879));
#60163=CARTESIAN_POINT('Ctrl Pts',(-50.,-9.58387033196931,12.8609845509879));
#60164=CARTESIAN_POINT('Ctrl Pts',(-66.,-9.49261168852801,12.8077483085937));
#60165=CARTESIAN_POINT('Ctrl Pts',(-50.,-9.49261168852801,12.8077483085937));
#60166=CARTESIAN_POINT('Ctrl Pts',(-66.,-9.40266201299437,12.7531750820743));
#60167=CARTESIAN_POINT('Ctrl Pts',(-50.,-9.40266201299437,12.7531750820743));
#60168=CARTESIAN_POINT('Ctrl Pts',(-66.,-9.31391109124575,12.69736527232));
#60169=CARTESIAN_POINT('Ctrl Pts',(-50.,-9.31391109124575,12.69736527232));
#60170=CARTESIAN_POINT('Ctrl Pts',(-66.,-9.22627089118454,12.6404031093252));
#60171=CARTESIAN_POINT('Ctrl Pts',(-50.,-9.22627089118454,12.6404031093252));
#60172=CARTESIAN_POINT('Ctrl Pts',(-66.,-9.13973729492348,12.5823087271131));
#60173=CARTESIAN_POINT('Ctrl Pts',(-50.,-9.13973729492348,12.5823087271131));
#60174=CARTESIAN_POINT('Ctrl Pts',(-66.,-9.05444479601274,12.5229957744206));
#60175=CARTESIAN_POINT('Ctrl Pts',(-50.,-9.05444479601274,12.5229957744206));
#60176=CARTESIAN_POINT('Ctrl Pts',(-66.,-8.9707478415549,12.4622081834688));
#60177=CARTESIAN_POINT('Ctrl Pts',(-50.,-8.9707478415549,12.4622081834688));
#60178=CARTESIAN_POINT('Ctrl Pts',(-66.,-8.88915113193907,12.3995752782536));
#60179=CARTESIAN_POINT('Ctrl Pts',(-50.,-8.88915113193907,12.3995752782536));
#60180=CARTESIAN_POINT('Ctrl Pts',(-66.,-8.81018880105177,12.334706907179));
#60181=CARTESIAN_POINT('Ctrl Pts',(-50.,-8.81018880105177,12.334706907179));
#60182=CARTESIAN_POINT('Ctrl Pts',(-66.,-8.73431624919877,12.2672787958196));
#60183=CARTESIAN_POINT('Ctrl Pts',(-50.,-8.73431624919877,12.2672787958196));
#60184=CARTESIAN_POINT('Ctrl Pts',(-66.,-8.66180575442286,12.1971147402934));
#60185=CARTESIAN_POINT('Ctrl Pts',(-50.,-8.66180575442286,12.1971147402934));
#60186=CARTESIAN_POINT('Ctrl Pts',(-66.,-8.59261438312223,12.1242911158748));
#60187=CARTESIAN_POINT('Ctrl Pts',(-50.,-8.59261438312223,12.1242911158748));
#60188=CARTESIAN_POINT('Ctrl Pts',(-66.,-8.52644368290816,12.0490873880617));
#60189=CARTESIAN_POINT('Ctrl Pts',(-50.,-8.52644368290816,12.0490873880617));
#60190=CARTESIAN_POINT('Ctrl Pts',(-66.,-8.46284859919381,11.9718971321485));
#60191=CARTESIAN_POINT('Ctrl Pts',(-50.,-8.46284859919381,11.9718971321485));
#60192=CARTESIAN_POINT('Ctrl Pts',(-66.,-8.40132990725019,11.8931522119833));
#60193=CARTESIAN_POINT('Ctrl Pts',(-50.,-8.40132990725019,11.8931522119833));
#60194=CARTESIAN_POINT('Ctrl Pts',(-66.,-8.34142932020866,11.8132449066089));
#60195=CARTESIAN_POINT('Ctrl Pts',(-50.,-8.34142932020866,11.8132449066089));
#60196=CARTESIAN_POINT('Ctrl Pts',(-66.,-8.28283244225497,11.732443384369));
#60197=CARTESIAN_POINT('Ctrl Pts',(-50.,-8.28283244225497,11.732443384369));
#60198=CARTESIAN_POINT('Ctrl Pts',(-66.,-8.22534976477564,11.6509086114121));
#60199=CARTESIAN_POINT('Ctrl Pts',(-50.,-8.22534976477564,11.6509086114121));
#60200=CARTESIAN_POINT('Ctrl Pts',(-66.,-8.18017633214654,11.5851604663126));
#60201=CARTESIAN_POINT('Ctrl Pts',(-50.,-8.18017633214654,11.5851604663126));
#60202=CARTESIAN_POINT('Ctrl Pts',(-66.,-8.14673761978747,11.5355697300868));
#60203=CARTESIAN_POINT('Ctrl Pts',(-50.,-8.14673761978747,11.5355697300868));
#60204=CARTESIAN_POINT('Ctrl Pts',(-66.,-8.12464103031309,11.502385137885));
#60205=CARTESIAN_POINT('Ctrl Pts',(-50.,-8.12464103031309,11.502385137885));
#60206=CARTESIAN_POINT('Ctrl Pts',(-66.,-8.11364170780698,11.4857618157149));
#60207=CARTESIAN_POINT('Ctrl Pts',(-50.,-8.11364170780698,11.4857618157149));
#60208=CARTESIAN_POINT('Origin',(-65.75,0.,0.));
#60209=CARTESIAN_POINT('',(-65.5,-6.80027886528895,15.4441520438742));
#60210=CARTESIAN_POINT('Origin',(-65.5,0.,0.));
#60211=CARTESIAN_POINT('Ctrl Pts',(-65.5,-6.80027886528895,15.4441520438742));
#60212=CARTESIAN_POINT('Ctrl Pts',(-65.6931595476699,-6.62246580329175,
15.3113905330037));
#60213=CARTESIAN_POINT('Ctrl Pts',(-65.8611256967037,-6.4758149961569,15.1913331461071));
#60214=CARTESIAN_POINT('Ctrl Pts',(-66.,-6.35845702927375,15.0900844665257));
#60215=CARTESIAN_POINT('Origin',(-58.,0.,0.));
#60216=CARTESIAN_POINT('',(-50.5,-6.80027886528895,15.4441520438742));
#60217=CARTESIAN_POINT('Origin',(-50.5,0.,0.));
#60218=CARTESIAN_POINT('Ctrl Pts',(-50.5,-6.80027886528895,15.4441520438742));
#60219=CARTESIAN_POINT('Ctrl Pts',(-55.5,-6.80027886528895,15.4441520438742));
#60220=CARTESIAN_POINT('Ctrl Pts',(-60.5,-6.80027886528895,15.4441520438742));
#60221=CARTESIAN_POINT('Ctrl Pts',(-65.5,-6.80027886528895,15.4441520438742));
#60222=CARTESIAN_POINT('Origin',(-50.25,0.,0.));
#60223=CARTESIAN_POINT('Ctrl Pts',(-50.,-6.35845702927375,15.0900844665257));
#60224=CARTESIAN_POINT('Ctrl Pts',(-50.1388743032885,-6.47581499615029,
15.1913331461014));
#60225=CARTESIAN_POINT('Ctrl Pts',(-50.306840452323,-6.62246580328526,15.3113905329989));
#60226=CARTESIAN_POINT('Ctrl Pts',(-50.5,-6.80027886528894,15.4441520438742));
#60227=CARTESIAN_POINT('Ctrl Pts',(-66.,-3.67810171359515,13.5729685048794));
#60228=CARTESIAN_POINT('Ctrl Pts',(-50.,-3.67810171359515,13.5729685048794));
#60229=CARTESIAN_POINT('Ctrl Pts',(-66.,-3.68513657707394,13.595256733151));
#60230=CARTESIAN_POINT('Ctrl Pts',(-50.,-3.68513657707394,13.595256733151));
#60231=CARTESIAN_POINT('Ctrl Pts',(-66.,-3.69899456508718,13.6399095715909));
#60232=CARTESIAN_POINT('Ctrl Pts',(-50.,-3.69899456508718,13.6399095715909));
#60233=CARTESIAN_POINT('Ctrl Pts',(-66.,-3.71914634329887,13.7071179779119));
#60234=CARTESIAN_POINT('Ctrl Pts',(-50.,-3.71914634329887,13.7071179779119));
#60235=CARTESIAN_POINT('Ctrl Pts',(-66.,-3.7447431715177,13.7971880673979));
#60236=CARTESIAN_POINT('Ctrl Pts',(-50.,-3.7447431715177,13.7971880673979));
#60237=CARTESIAN_POINT('Ctrl Pts',(-66.,-3.77456181293102,13.910540963737));
#60238=CARTESIAN_POINT('Ctrl Pts',(-50.,-3.77456181293102,13.910540963737));
#60239=CARTESIAN_POINT('Ctrl Pts',(-66.,-3.80204670961501,14.0246539387008));
#60240=CARTESIAN_POINT('Ctrl Pts',(-50.,-3.80204670961501,14.0246539387008));
#60241=CARTESIAN_POINT('Ctrl Pts',(-66.,-3.82690130950572,14.1395127300348));
#60242=CARTESIAN_POINT('Ctrl Pts',(-50.,-3.82690130950572,14.1395127300348));
#60243=CARTESIAN_POINT('Ctrl Pts',(-66.,-3.84863270462788,14.2550869169872));
#60244=CARTESIAN_POINT('Ctrl Pts',(-50.,-3.84863270462788,14.2550869169872));
#60245=CARTESIAN_POINT('Ctrl Pts',(-66.,-3.86661269999714,14.3713582537855));
#60246=CARTESIAN_POINT('Ctrl Pts',(-50.,-3.86661269999714,14.3713582537855));
#60247=CARTESIAN_POINT('Ctrl Pts',(-66.,-3.88015661753544,14.4883613559395));
#60248=CARTESIAN_POINT('Ctrl Pts',(-50.,-3.88015661753544,14.4883613559395));
#60249=CARTESIAN_POINT('Ctrl Pts',(-66.,-3.88860209359085,14.6062092864715));
#60250=CARTESIAN_POINT('Ctrl Pts',(-50.,-3.88860209359085,14.6062092864715));
#60251=CARTESIAN_POINT('Ctrl Pts',(-66.,-3.89137277258683,14.725152856237));
#60252=CARTESIAN_POINT('Ctrl Pts',(-50.,-3.89137277258683,14.725152856237));
#60253=CARTESIAN_POINT('Ctrl Pts',(-66.,-3.88814619886307,14.8454766736426));
#60254=CARTESIAN_POINT('Ctrl Pts',(-50.,-3.88814619886307,14.8454766736426));
#60255=CARTESIAN_POINT('Ctrl Pts',(-66.,-3.87911646405442,14.9672939298197));
#60256=CARTESIAN_POINT('Ctrl Pts',(-50.,-3.87911646405442,14.9672939298197));
#60257=CARTESIAN_POINT('Ctrl Pts',(-66.,-3.86515944096752,15.0904102873887));
#60258=CARTESIAN_POINT('Ctrl Pts',(-50.,-3.86515944096752,15.0904102873887));
#60259=CARTESIAN_POINT('Ctrl Pts',(-66.,-3.84820772362302,15.2140685453126));
#60260=CARTESIAN_POINT('Ctrl Pts',(-50.,-3.84820772362302,15.2140685453126));
#60261=CARTESIAN_POINT('Ctrl Pts',(-66.,-3.83091743061146,15.3370768226993));
#60262=CARTESIAN_POINT('Ctrl Pts',(-50.,-3.83091743061146,15.3370768226993));
#60263=CARTESIAN_POINT('Ctrl Pts',(-66.,-3.81540012098238,15.4584321984421));
#60264=CARTESIAN_POINT('Ctrl Pts',(-50.,-3.81540012098238,15.4584321984421));
#60265=CARTESIAN_POINT('Ctrl Pts',(-66.,-3.80229765686693,15.5777692855585));
#60266=CARTESIAN_POINT('Ctrl Pts',(-50.,-3.80229765686693,15.5777692855585));
#60267=CARTESIAN_POINT('Ctrl Pts',(-66.,-3.7894772918181,15.6959915606914));
#60268=CARTESIAN_POINT('Ctrl Pts',(-50.,-3.7894772918181,15.6959915606914));
#60269=CARTESIAN_POINT('Ctrl Pts',(-66.,-3.77157499875327,15.8155054601092));
#60270=CARTESIAN_POINT('Ctrl Pts',(-50.,-3.77157499875327,15.8155054601092));
#60271=CARTESIAN_POINT('Ctrl Pts',(-66.,-3.74294840184491,15.9388689441728));
#60272=CARTESIAN_POINT('Ctrl Pts',(-50.,-3.74294840184491,15.9388689441728));
#60273=CARTESIAN_POINT('Ctrl Pts',(-66.,-3.70020363548059,16.0676386536046));
#60274=CARTESIAN_POINT('Ctrl Pts',(-50.,-3.70020363548059,16.0676386536046));
#60275=CARTESIAN_POINT('Ctrl Pts',(-66.,-3.64477327324364,16.2011922392645));
#60276=CARTESIAN_POINT('Ctrl Pts',(-50.,-3.64477327324364,16.2011922392645));
#60277=CARTESIAN_POINT('Ctrl Pts',(-66.,-3.58582697007134,16.3354002467575));
#60278=CARTESIAN_POINT('Ctrl Pts',(-50.,-3.58582697007134,16.3354002467575));
#60279=CARTESIAN_POINT('Ctrl Pts',(-66.,-3.53803421809535,16.4636392581249));
#60280=CARTESIAN_POINT('Ctrl Pts',(-50.,-3.53803421809535,16.4636392581249));
#60281=CARTESIAN_POINT('Ctrl Pts',(-66.,-3.51871761353015,16.5780823618678));
#60282=CARTESIAN_POINT('Ctrl Pts',(-50.,-3.51871761353015,16.5780823618678));
#60283=CARTESIAN_POINT('Ctrl Pts',(-66.,-3.54543232907923,16.6707961095521));
#60284=CARTESIAN_POINT('Ctrl Pts',(-50.,-3.54543232907923,16.6707961095521));
#60285=CARTESIAN_POINT('Ctrl Pts',(-66.,-3.63291117576394,16.7351253498724));
#60286=CARTESIAN_POINT('Ctrl Pts',(-50.,-3.63291117576394,16.7351253498724));
#60287=CARTESIAN_POINT('Ctrl Pts',(-66.,-3.79224306450002,16.7660653478883));
#60288=CARTESIAN_POINT('Ctrl Pts',(-50.,-3.79224306450002,16.7660653478883));
#60289=CARTESIAN_POINT('Ctrl Pts',(-66.,-4.03169118248789,16.7598904736431));
#60290=CARTESIAN_POINT('Ctrl Pts',(-50.,-4.03169118248789,16.7598904736431));
#60291=CARTESIAN_POINT('Ctrl Pts',(-66.,-4.35701441935439,16.7140081864924));
#60292=CARTESIAN_POINT('Ctrl Pts',(-50.,-4.35701441935439,16.7140081864924));
#60293=CARTESIAN_POINT('Ctrl Pts',(-66.,-4.77196943773181,16.6267311678792));
#60294=CARTESIAN_POINT('Ctrl Pts',(-50.,-4.77196943773181,16.6267311678792));
#60295=CARTESIAN_POINT('Ctrl Pts',(-66.,-5.27871307427053,16.497094699955));
#60296=CARTESIAN_POINT('Ctrl Pts',(-50.,-5.27871307427053,16.497094699955));
#60297=CARTESIAN_POINT('Ctrl Pts',(-66.,-5.87822732718726,16.3246638547222));
#60298=CARTESIAN_POINT('Ctrl Pts',(-50.,-5.87822732718726,16.3246638547222));
#60299=CARTESIAN_POINT('Ctrl Pts',(-66.,-6.43221851326742,16.1524155266404));
#60300=CARTESIAN_POINT('Ctrl Pts',(-50.,-6.43221851326742,16.1524155266404));
#60301=CARTESIAN_POINT('Ctrl Pts',(-66.,-6.88946917964989,16.0039723335548));
#60302=CARTESIAN_POINT('Ctrl Pts',(-50.,-6.88946917964989,16.0039723335548));
#60303=CARTESIAN_POINT('Ctrl Pts',(-66.,-7.21283706267689,15.8964629450382));
#60304=CARTESIAN_POINT('Ctrl Pts',(-50.,-7.21283706267689,15.8964629450382));
#60305=CARTESIAN_POINT('Ctrl Pts',(-66.,-7.37915453260775,15.8405714348913));
#60306=CARTESIAN_POINT('Ctrl Pts',(-50.,-7.37915453260775,15.8405714348913));
#60307=CARTESIAN_POINT('',(-65.5,-3.53600294066089,16.5003729716524));
#60308=CARTESIAN_POINT('Ctrl Pts',(-66.,-3.73881834218223,15.9424547170178));
#60309=CARTESIAN_POINT('Ctrl Pts',(-65.7933280154032,-3.67390909465031,
16.1699565476581));
#60310=CARTESIAN_POINT('Ctrl Pts',(-65.6370761749492,-3.56304111052069,
16.3543903623781));
#60311=CARTESIAN_POINT('Ctrl Pts',(-65.5,-3.53600294066089,16.5003729716524));
#60312=CARTESIAN_POINT('',(-66.,-3.67810171359515,13.5729685048794));
#60313=CARTESIAN_POINT('',(-50.5,-3.53600294066089,16.5003729716524));
#60314=CARTESIAN_POINT('Ctrl Pts',(-50.5,-3.53600294066089,16.5003729716524));
#60315=CARTESIAN_POINT('Ctrl Pts',(-50.4518618349121,-3.54549815662287,
16.4491070609439));
#60316=CARTESIAN_POINT('Ctrl Pts',(-50.4012423593883,-3.5651004382447,16.3930954524971));
#60317=CARTESIAN_POINT('Ctrl Pts',(-50.2441129793802,-3.63518359270379,
16.2168265139271));
#60318=CARTESIAN_POINT('Ctrl Pts',(-50.1366827452941,-3.69589053963102,
16.0929133040005));
#60319=CARTESIAN_POINT('Ctrl Pts',(-50.,-3.73881834218223,15.9424547170178));
#60320=CARTESIAN_POINT('Ctrl Pts',(-65.5,-3.53600294066089,16.5003729716524));
#60321=CARTESIAN_POINT('Ctrl Pts',(-60.5,-3.53600294066089,16.5003729716524));
#60322=CARTESIAN_POINT('Ctrl Pts',(-55.5,-3.53600294066089,16.5003729716524));
#60323=CARTESIAN_POINT('Ctrl Pts',(-50.5,-3.53600294066089,16.5003729716524));
#60324=CARTESIAN_POINT('Origin',(-66.,0.,0.));
#60325=CARTESIAN_POINT('',(-66.,-5.00234392366024,13.1426961282463));
#60326=CARTESIAN_POINT('Ctrl Pts',(-66.,-7.37915453260775,15.8405714348913));
#60327=CARTESIAN_POINT('Ctrl Pts',(-50.,-7.37915453260775,15.8405714348913));
#60328=CARTESIAN_POINT('Ctrl Pts',(-66.,-7.36009119386413,15.8286023123826));
#60329=CARTESIAN_POINT('Ctrl Pts',(-50.,-7.36009119386413,15.8286023123826));
#60330=CARTESIAN_POINT('Ctrl Pts',(-66.,-7.32208075369696,15.8045726787264));
#60331=CARTESIAN_POINT('Ctrl Pts',(-50.,-7.32208075369696,15.8045726787264));
#60332=CARTESIAN_POINT('Ctrl Pts',(-66.,-7.26541380484018,15.7682540626965));
#60333=CARTESIAN_POINT('Ctrl Pts',(-50.,-7.26541380484018,15.7682540626965));
#60334=CARTESIAN_POINT('Ctrl Pts',(-66.,-7.19055622819912,15.7192801778145));
#60335=CARTESIAN_POINT('Ctrl Pts',(-50.,-7.19055622819912,15.7192801778145));
#60336=CARTESIAN_POINT('Ctrl Pts',(-66.,-7.09815314002604,15.6571442133981));
#60337=CARTESIAN_POINT('Ctrl Pts',(-50.,-7.09815314002604,15.6571442133981));
#60338=CARTESIAN_POINT('Ctrl Pts',(-66.,-7.00692452080779,15.594086447551));
#60339=CARTESIAN_POINT('Ctrl Pts',(-50.,-7.00692452080779,15.594086447551));
#60340=CARTESIAN_POINT('Ctrl Pts',(-66.,-6.91687426177195,15.5301062024295));
#60341=CARTESIAN_POINT('Ctrl Pts',(-50.,-6.91687426177195,15.5301062024295));
#60342=CARTESIAN_POINT('Ctrl Pts',(-66.,-6.82800264685238,15.4652072799773));
#60343=CARTESIAN_POINT('Ctrl Pts',(-50.,-6.82800264685238,15.4652072799773));
#60344=CARTESIAN_POINT('Ctrl Pts',(-66.,-6.74030300800744,15.3994008612236));
#60345=CARTESIAN_POINT('Ctrl Pts',(-50.,-6.74030300800744,15.3994008612236));
#60346=CARTESIAN_POINT('Ctrl Pts',(-66.,-6.65377009817984,15.3327008873786));
#60347=CARTESIAN_POINT('Ctrl Pts',(-50.,-6.65377009817984,15.3327008873786));
#60348=CARTESIAN_POINT('Ctrl Pts',(-66.,-6.56840971106354,15.2651185924859));
#60349=CARTESIAN_POINT('Ctrl Pts',(-50.,-6.56840971106354,15.2651185924859));
#60350=CARTESIAN_POINT('Ctrl Pts',(-66.,-6.48424857382376,15.1966570511038));
#60351=CARTESIAN_POINT('Ctrl Pts',(-50.,-6.48424857382376,15.1966570511038));
#60352=CARTESIAN_POINT('Ctrl Pts',(-66.,-6.40134228048028,15.1273066437657));
#60353=CARTESIAN_POINT('Ctrl Pts',(-50.,-6.40134228048028,15.1273066437657));
#60354=CARTESIAN_POINT('Ctrl Pts',(-66.,-6.31978872192241,15.0570379669215));
#60355=CARTESIAN_POINT('Ctrl Pts',(-50.,-6.31978872192241,15.0570379669215));
#60356=CARTESIAN_POINT('Ctrl Pts',(-66.,-6.23970763367462,14.9858108444093));
#60357=CARTESIAN_POINT('Ctrl Pts',(-50.,-6.23970763367462,14.9858108444093));
#60358=CARTESIAN_POINT('Ctrl Pts',(-66.,-6.16121181596629,14.913587364225));
#60359=CARTESIAN_POINT('Ctrl Pts',(-50.,-6.16121181596629,14.913587364225));
#60360=CARTESIAN_POINT('Ctrl Pts',(-66.,-6.08437862517161,14.8403447030824));
#60361=CARTESIAN_POINT('Ctrl Pts',(-50.,-6.08437862517161,14.8403447030824));
#60362=CARTESIAN_POINT('Ctrl Pts',(-66.,-6.00922635494104,14.7660858733973));
#60363=CARTESIAN_POINT('Ctrl Pts',(-50.,-6.00922635494104,14.7660858733973));
#60364=CARTESIAN_POINT('Ctrl Pts',(-66.,-5.93567442341548,14.6908575904833));
#60365=CARTESIAN_POINT('Ctrl Pts',(-50.,-5.93567442341548,14.6908575904833));
#60366=CARTESIAN_POINT('Ctrl Pts',(-66.,-5.86359111036561,14.614729691814));
#60367=CARTESIAN_POINT('Ctrl Pts',(-50.,-5.86359111036561,14.614729691814));
#60368=CARTESIAN_POINT('Ctrl Pts',(-66.,-5.79287020223623,14.5377618684515));
#60369=CARTESIAN_POINT('Ctrl Pts',(-50.,-5.79287020223623,14.5377618684515));
#60370=CARTESIAN_POINT('Ctrl Pts',(-66.,-5.72350270338309,14.4599725977946));
#60371=CARTESIAN_POINT('Ctrl Pts',(-50.,-5.72350270338309,14.4599725977946));
#60372=CARTESIAN_POINT('Ctrl Pts',(-66.,-5.6556403566801,14.3813116886496));
#60373=CARTESIAN_POINT('Ctrl Pts',(-50.,-5.6556403566801,14.3813116886496));
#60374=CARTESIAN_POINT('Ctrl Pts',(-66.,-5.5896901550893,14.301619265488));
#60375=CARTESIAN_POINT('Ctrl Pts',(-50.,-5.5896901550893,14.301619265488));
#60376=CARTESIAN_POINT('Ctrl Pts',(-66.,-5.52623312628269,14.2206618116565));
#60377=CARTESIAN_POINT('Ctrl Pts',(-50.,-5.52623312628269,14.2206618116565));
#60378=CARTESIAN_POINT('Ctrl Pts',(-66.,-5.46588365010489,14.1381942665852));
#60379=CARTESIAN_POINT('Ctrl Pts',(-50.,-5.46588365010489,14.1381942665852));
#60380=CARTESIAN_POINT('Ctrl Pts',(-66.,-5.40916346339393,14.0540157969766));
#60381=CARTESIAN_POINT('Ctrl Pts',(-50.,-5.40916346339393,14.0540157969766));
#60382=CARTESIAN_POINT('Ctrl Pts',(-66.,-5.35638011020072,13.9680234475133));
#60383=CARTESIAN_POINT('Ctrl Pts',(-50.,-5.35638011020072,13.9680234475133));
#60384=CARTESIAN_POINT('Ctrl Pts',(-66.,-5.30747301200313,13.8802805168475));
#60385=CARTESIAN_POINT('Ctrl Pts',(-50.,-5.30747301200313,13.8802805168475));
#60386=CARTESIAN_POINT('Ctrl Pts',(-66.,-5.2620835925999,13.7909834684638));
#60387=CARTESIAN_POINT('Ctrl Pts',(-50.,-5.2620835925999,13.7909834684638));
#60388=CARTESIAN_POINT('Ctrl Pts',(-66.,-5.21968290141691,13.7004028321899));
#60389=CARTESIAN_POINT('Ctrl Pts',(-50.,-5.21968290141691,13.7004028321899));
#60390=CARTESIAN_POINT('Ctrl Pts',(-66.,-5.17967999761633,13.6088327519355));
#60391=CARTESIAN_POINT('Ctrl Pts',(-50.,-5.17967999761633,13.6088327519355));
#60392=CARTESIAN_POINT('Ctrl Pts',(-66.,-5.14153343642338,13.5165392112663));
#60393=CARTESIAN_POINT('Ctrl Pts',(-50.,-5.14153343642338,13.5165392112663));
#60394=CARTESIAN_POINT('Ctrl Pts',(-66.,-5.10487200859133,13.4237037664646));
#60395=CARTESIAN_POINT('Ctrl Pts',(-50.,-5.10487200859133,13.4237037664646));
#60396=CARTESIAN_POINT('Ctrl Pts',(-66.,-5.06947212861492,13.3304351977558));
#60397=CARTESIAN_POINT('Ctrl Pts',(-50.,-5.06947212861492,13.3304351977558));
#60398=CARTESIAN_POINT('Ctrl Pts',(-66.,-5.04206880122609,13.2555184756737));
#60399=CARTESIAN_POINT('Ctrl Pts',(-50.,-5.04206880122609,13.2555184756737));
#60400=CARTESIAN_POINT('Ctrl Pts',(-66.,-5.02201334210169,13.1991698540138));
#60401=CARTESIAN_POINT('Ctrl Pts',(-50.,-5.02201334210169,13.1991698540138));
#60402=CARTESIAN_POINT('Ctrl Pts',(-66.,-5.00886363010872,13.1615326184551));
#60403=CARTESIAN_POINT('Ctrl Pts',(-50.,-5.00886363010872,13.1615326184551));
#60404=CARTESIAN_POINT('Ctrl Pts',(-66.,-5.00234392366025,13.1426961282463));
#60405=CARTESIAN_POINT('Ctrl Pts',(-50.,-5.00234392366025,13.1426961282463));
#60406=CARTESIAN_POINT('Origin',(-65.75,0.,0.));
#60407=CARTESIAN_POINT('',(-65.5,-2.74583117074985,16.6501061913052));
#60408=CARTESIAN_POINT('Origin',(-65.5,0.,0.));
#60409=CARTESIAN_POINT('Ctrl Pts',(-65.5,-2.74583117077843,16.6501061913406));
#60410=CARTESIAN_POINT('Ctrl Pts',(-65.5715932578482,-2.69423901044128,
16.5860614560832));
#60411=CARTESIAN_POINT('Ctrl Pts',(-65.6431740852859,-2.64390488478764,
16.5216686692745));
#60412=CARTESIAN_POINT('Ctrl Pts',(-65.7145580549966,-2.59494005965581,
16.4571219801265));
#60413=CARTESIAN_POINT('Ctrl Pts',(-65.774031663176,-2.55414497868363,16.4033448574024));
#60414=CARTESIAN_POINT('Ctrl Pts',(-65.8333686244976,-2.51429886362145,
16.3494616552359));
#60415=CARTESIAN_POINT('Ctrl Pts',(-65.8924622803263,-2.47551032558372,
16.2955807679008));
#60416=CARTESIAN_POINT('Ctrl Pts',(-65.9284062038969,-2.45191706117835,
16.2628075290626));
#60417=CARTESIAN_POINT('Ctrl Pts',(-65.9642601111668,-2.42871664894537,
16.2300349028932));
#60418=CARTESIAN_POINT('Ctrl Pts',(-66.,-2.40594300602613,16.1972856754381));
#60419=CARTESIAN_POINT('Origin',(-58.,0.,0.));
#60420=CARTESIAN_POINT('',(-50.5,-2.74583117074985,16.6501061913052));
#60421=CARTESIAN_POINT('Origin',(-50.5,0.,0.));
#60422=CARTESIAN_POINT('Ctrl Pts',(-50.5,-2.74583117074984,16.6501061913052));
#60423=CARTESIAN_POINT('Ctrl Pts',(-55.5,-2.74583117074984,16.6501061913052));
#60424=CARTESIAN_POINT('Ctrl Pts',(-60.5,-2.74583117074984,16.6501061913052));
#60425=CARTESIAN_POINT('Ctrl Pts',(-65.5,-2.74583117074984,16.6501061913052));
#60426=CARTESIAN_POINT('Origin',(-50.25,0.,0.));
#60427=CARTESIAN_POINT('Ctrl Pts',(-50.,-2.40594300602613,16.1972856754381));
#60428=CARTESIAN_POINT('Ctrl Pts',(-50.0590457046711,-2.44356723592708,
16.2513905223095));
#60429=CARTESIAN_POINT('Ctrl Pts',(-50.1184026134405,-2.482354056013,16.3055596366217));
#60430=CARTESIAN_POINT('Ctrl Pts',(-50.177962494421,-2.52215873348076,16.3596887934234));
#60431=CARTESIAN_POINT('Ctrl Pts',(-50.2399196509175,-2.56356554273836,
16.4159966399769));
#60432=CARTESIAN_POINT('Ctrl Pts',(-50.3020964476471,-2.6060736528862,16.4722610173791));
#60433=CARTESIAN_POINT('Ctrl Pts',(-50.3643710506945,-2.64958385609203,
16.5283547796601));
#60434=CARTESIAN_POINT('Ctrl Pts',(-50.4095447363725,-2.68114593994685,
16.5690449143504));
#60435=CARTESIAN_POINT('Ctrl Pts',(-50.4547698875302,-2.71323705109809,
16.6096449710267));
#60436=CARTESIAN_POINT('Ctrl Pts',(-50.5,-2.74583117077843,16.6501061913406));
#60437=CARTESIAN_POINT('Ctrl Pts',(-66.,-0.187087378736033,14.0612554404903));
#60438=CARTESIAN_POINT('Ctrl Pts',(-50.,-0.187087378736033,14.0612554404903));
#60439=CARTESIAN_POINT('Ctrl Pts',(-66.,-0.188358372068459,14.0845929424903));
#60440=CARTESIAN_POINT('Ctrl Pts',(-50.,-0.188358372068459,14.0845929424903));
#60441=CARTESIAN_POINT('Ctrl Pts',(-66.,-0.190676276552008,14.1312892713751));
#60442=CARTESIAN_POINT('Ctrl Pts',(-50.,-0.190676276552008,14.1312892713751));
#60443=CARTESIAN_POINT('Ctrl Pts',(-66.,-0.193480898610155,14.2013977454735));
#60444=CARTESIAN_POINT('Ctrl Pts',(-50.,-0.193480898610155,14.2013977454735));
#60445=CARTESIAN_POINT('Ctrl Pts',(-66.,-0.195874035010017,14.2950037897925));
#60446=CARTESIAN_POINT('Ctrl Pts',(-50.,-0.195874035010017,14.2950037897925));
#60447=CARTESIAN_POINT('Ctrl Pts',(-66.,-0.196566149970303,14.4122110910203));
#60448=CARTESIAN_POINT('Ctrl Pts',(-50.,-0.196566149970303,14.4122110910203));
#60449=CARTESIAN_POINT('Ctrl Pts',(-66.,-0.194808815215985,14.5295742128916));
#60450=CARTESIAN_POINT('Ctrl Pts',(-50.,-0.194808815215985,14.5295742128916));
#60451=CARTESIAN_POINT('Ctrl Pts',(-66.,-0.190318342289957,14.6470055917277));
#60452=CARTESIAN_POINT('Ctrl Pts',(-50.,-0.190318342289957,14.6470055917277));
#60453=CARTESIAN_POINT('Ctrl Pts',(-66.,-0.182624874160768,14.7643531812717));
#60454=CARTESIAN_POINT('Ctrl Pts',(-50.,-0.182624874160768,14.7643531812717));
#60455=CARTESIAN_POINT('Ctrl Pts',(-66.,-0.171124489283723,14.8814430832361));
#60456=CARTESIAN_POINT('Ctrl Pts',(-50.,-0.171124489283723,14.8814430832361));
#60457=CARTESIAN_POINT('Ctrl Pts',(-66.,-0.155145411474415,14.9981385531066));
#60458=CARTESIAN_POINT('Ctrl Pts',(-50.,-0.155145411474415,14.9981385531066));
#60459=CARTESIAN_POINT('Ctrl Pts',(-66.,-0.13401796882278,15.1143843786811));
#60460=CARTESIAN_POINT('Ctrl Pts',(-50.,-0.13401796882278,15.1143843786811));
#60461=CARTESIAN_POINT('Ctrl Pts',(-66.,-0.107121538899203,15.2302801573274));
#60462=CARTESIAN_POINT('Ctrl Pts',(-50.,-0.107121538899203,15.2302801573274));
#60463=CARTESIAN_POINT('Ctrl Pts',(-66.,-0.0740730173483893,15.3460213644938));
#60464=CARTESIAN_POINT('Ctrl Pts',(-50.,-0.0740730173483893,15.3460213644938));
#60465=CARTESIAN_POINT('Ctrl Pts',(-66.,-0.035032248569878,15.4617659038311));
#60466=CARTESIAN_POINT('Ctrl Pts',(-50.,-0.035032248569878,15.4617659038311));
#60467=CARTESIAN_POINT('Ctrl Pts',(-66.,0.00910408204356977,15.5775433641354));
#60468=CARTESIAN_POINT('Ctrl Pts',(-50.,0.00910408204356977,15.5775433641354));
#60469=CARTESIAN_POINT('Ctrl Pts',(-66.,0.0562757882257695,15.6931009498213));
#60470=CARTESIAN_POINT('Ctrl Pts',(-50.,0.0562757882257695,15.6931009498213));
#60471=CARTESIAN_POINT('Ctrl Pts',(-66.,0.103613789511375,15.8079447749594));
#60472=CARTESIAN_POINT('Ctrl Pts',(-50.,0.103613789511375,15.8079447749594));
#60473=CARTESIAN_POINT('Ctrl Pts',(-66.,0.148823449024451,15.9216285504355));
#60474=CARTESIAN_POINT('Ctrl Pts',(-50.,0.148823449024451,15.9216285504355));
#60475=CARTESIAN_POINT('Ctrl Pts',(-66.,0.191192201865526,16.0339579931922));
#60476=CARTESIAN_POINT('Ctrl Pts',(-50.,0.191192201865526,16.0339579931922));
#60477=CARTESIAN_POINT('Ctrl Pts',(-66.,0.233010475834533,16.1452778030188));
#60478=CARTESIAN_POINT('Ctrl Pts',(-50.,0.233010475834533,16.1452778030188));
#60479=CARTESIAN_POINT('Ctrl Pts',(-66.,0.280072233603551,16.2565848342734));
#60480=CARTESIAN_POINT('Ctrl Pts',(-50.,0.280072233603551,16.2565848342734));
#60481=CARTESIAN_POINT('Ctrl Pts',(-66.,0.338478724261455,16.3689534824806));
#60482=CARTESIAN_POINT('Ctrl Pts',(-50.,0.338478724261455,16.3689534824806));
#60483=CARTESIAN_POINT('Ctrl Pts',(-66.,0.411904309697133,16.4830474635755));
#60484=CARTESIAN_POINT('Ctrl Pts',(-50.,0.411904309697133,16.4830474635755));
#60485=CARTESIAN_POINT('Ctrl Pts',(-66.,0.498806651323343,16.5986202472239));
#60486=CARTESIAN_POINT('Ctrl Pts',(-50.,0.498806651323343,16.5986202472239));
#60487=CARTESIAN_POINT('Ctrl Pts',(-66.,0.589277222226854,16.7139525138855));
#60488=CARTESIAN_POINT('Ctrl Pts',(-50.,0.589277222226854,16.7139525138855));
#60489=CARTESIAN_POINT('Ctrl Pts',(-66.,0.667460222281906,16.8262770867996));
#60490=CARTESIAN_POINT('Ctrl Pts',(-50.,0.667460222281906,16.8262770867996));
#60491=CARTESIAN_POINT('Ctrl Pts',(-66.,0.714630802750556,16.9323209057825));
#60492=CARTESIAN_POINT('Ctrl Pts',(-50.,0.714630802750556,16.9323209057825));
#60493=CARTESIAN_POINT('Ctrl Pts',(-66.,0.711812350565616,17.0287655601902));
#60494=CARTESIAN_POINT('Ctrl Pts',(-50.,0.711812350565616,17.0287655601902));
#60495=CARTESIAN_POINT('Ctrl Pts',(-66.,0.643079844228511,17.112828883644));
#60496=CARTESIAN_POINT('Ctrl Pts',(-50.,0.643079844228511,17.112828883644));
#60497=CARTESIAN_POINT('Ctrl Pts',(-66.,0.496448124383368,17.1824210741591));
#60498=CARTESIAN_POINT('Ctrl Pts',(-50.,0.496448124383368,17.1824210741591));
#60499=CARTESIAN_POINT('Ctrl Pts',(-66.,0.262987080557083,17.2359885203873));
#60500=CARTESIAN_POINT('Ctrl Pts',(-50.,0.262987080557083,17.2359885203873));
#60501=CARTESIAN_POINT('Ctrl Pts',(-66.,-0.0635259894100476,17.2724523087275));
#60502=CARTESIAN_POINT('Ctrl Pts',(-50.,-0.0635259894100476,17.2724523087275));
#60503=CARTESIAN_POINT('Ctrl Pts',(-66.,-0.487149344747227,17.2911123748441));
#60504=CARTESIAN_POINT('Ctrl Pts',(-50.,-0.487149344747227,17.2911123748441));
#60505=CARTESIAN_POINT('Ctrl Pts',(-66.,-1.01021197668826,17.2915706927367));
#60506=CARTESIAN_POINT('Ctrl Pts',(-50.,-1.01021197668826,17.2915706927367));
#60507=CARTESIAN_POINT('Ctrl Pts',(-66.,-1.6337731943647,17.2736502114967));
#60508=CARTESIAN_POINT('Ctrl Pts',(-50.,-1.6337731943647,17.2736502114967));
#60509=CARTESIAN_POINT('Ctrl Pts',(-66.,-2.21319614589061,17.2445853869407));
#60510=CARTESIAN_POINT('Ctrl Pts',(-50.,-2.21319614589061,17.2445853869407));
#60511=CARTESIAN_POINT('Ctrl Pts',(-66.,-2.69299776270237,17.2145194263625));
#60512=CARTESIAN_POINT('Ctrl Pts',(-50.,-2.69299776270237,17.2145194263625));
#60513=CARTESIAN_POINT('Ctrl Pts',(-66.,-3.03294294675148,17.1908059653249));
#60514=CARTESIAN_POINT('Ctrl Pts',(-50.,-3.03294294675148,17.1908059653249));
#60515=CARTESIAN_POINT('Ctrl Pts',(-66.,-3.20793490087994,17.1780318625772));
#60516=CARTESIAN_POINT('Ctrl Pts',(-50.,-3.20793490087994,17.1780318625772));
#60517=CARTESIAN_POINT('',(-65.5,0.678562986472808,16.8613515850121));
#60518=CARTESIAN_POINT('Ctrl Pts',(-66.,0.343370775949386,16.3713994976063));
#60519=CARTESIAN_POINT('Ctrl Pts',(-65.815380499579,0.450072808997186,16.5538216515551));
#60520=CARTESIAN_POINT('Ctrl Pts',(-65.6764528558945,0.580559344874713,
16.6885936485503));
#60521=CARTESIAN_POINT('Ctrl Pts',(-65.5311665204831,0.663332916123189,
16.8307690367319));
#60522=CARTESIAN_POINT('Ctrl Pts',(-65.5154842698951,0.671503698056154,
16.8461388731867));
#60523=CARTESIAN_POINT('Ctrl Pts',(-65.5,0.678562986472805,16.8613515850121));
#60524=CARTESIAN_POINT('',(-66.,-0.187087378736033,14.0612554404903));
#60525=CARTESIAN_POINT('',(-50.5,0.678562986472808,16.8613515850121));
#60526=CARTESIAN_POINT('Ctrl Pts',(-50.5,0.678562986472804,16.8613515850121));
#60527=CARTESIAN_POINT('Ctrl Pts',(-50.4432410236137,0.652686533320046,
16.8055880290214));
#60528=CARTESIAN_POINT('Ctrl Pts',(-50.3823247550295,0.611185010004192,
16.7462340757651));
#60529=CARTESIAN_POINT('Ctrl Pts',(-50.2209638885107,0.493245381173695,
16.5887724832778));
#60530=CARTESIAN_POINT('Ctrl Pts',(-50.1226787683011,0.414273762685218,
16.4926181397662));
#60531=CARTESIAN_POINT('Ctrl Pts',(-50.,0.343370775949384,16.3713994976063));
#60532=CARTESIAN_POINT('Ctrl Pts',(-65.5,0.678562986472805,16.8613515850121));
#60533=CARTESIAN_POINT('Ctrl Pts',(-60.5,0.678562986472805,16.8613515850121));
#60534=CARTESIAN_POINT('Ctrl Pts',(-55.5,0.678562986472804,16.8613515850121));
#60535=CARTESIAN_POINT('Ctrl Pts',(-50.5,0.678562986472804,16.8613515850121));
#60536=CARTESIAN_POINT('Origin',(-66.,0.,0.));
#60537=CARTESIAN_POINT('',(-66.,-1.57673047345589,13.9738265075847));
#60538=CARTESIAN_POINT('Ctrl Pts',(-66.,-3.20793490087994,17.1780318625772));
#60539=CARTESIAN_POINT('Ctrl Pts',(-50.,-3.20793490087994,17.1780318625772));
#60540=CARTESIAN_POINT('Ctrl Pts',(-66.,-3.19244707170413,17.1616979125006));
#60541=CARTESIAN_POINT('Ctrl Pts',(-50.,-3.19244707170413,17.1616979125006));
#60542=CARTESIAN_POINT('Ctrl Pts',(-66.,-3.16160672629369,17.1289704018969));
#60543=CARTESIAN_POINT('Ctrl Pts',(-50.,-3.16160672629369,17.1289704018969));
#60544=CARTESIAN_POINT('Ctrl Pts',(-66.,-3.11575214636094,17.0797003048576));
#60545=CARTESIAN_POINT('Ctrl Pts',(-50.,-3.11575214636094,17.0797003048576));
#60546=CARTESIAN_POINT('Ctrl Pts',(-66.,-3.05542566804884,17.0136487023376));
#60547=CARTESIAN_POINT('Ctrl Pts',(-50.,-3.05542566804884,17.0136487023376));
#60548=CARTESIAN_POINT('Ctrl Pts',(-66.,-2.9813781787877,16.930485139932));
#60549=CARTESIAN_POINT('Ctrl Pts',(-50.,-2.9813781787877,16.930485139932));
#60550=CARTESIAN_POINT('Ctrl Pts',(-66.,-2.90869750307329,16.8467208147344));
#60551=CARTESIAN_POINT('Ctrl Pts',(-50.,-2.90869750307329,16.8467208147344));
#60552=CARTESIAN_POINT('Ctrl Pts',(-66.,-2.83738757845593,16.7623560379061));
#60553=CARTESIAN_POINT('Ctrl Pts',(-50.,-2.83738757845593,16.7623560379061));
#60554=CARTESIAN_POINT('Ctrl Pts',(-66.,-2.7674477344443,16.6773945625569));
#60555=CARTESIAN_POINT('Ctrl Pts',(-50.,-2.7674477344443,16.6773945625569));
#60556=CARTESIAN_POINT('Ctrl Pts',(-66.,-2.69886873187661,16.5918455601692));
#60557=CARTESIAN_POINT('Ctrl Pts',(-50.,-2.69886873187661,16.5918455601692));
#60558=CARTESIAN_POINT('Ctrl Pts',(-66.,-2.63164202150355,16.5057212290741));
#60559=CARTESIAN_POINT('Ctrl Pts',(-50.,-2.63164202150355,16.5057212290741));
#60560=CARTESIAN_POINT('Ctrl Pts',(-66.,-2.56577042120647,16.4190338912104));
#60561=CARTESIAN_POINT('Ctrl Pts',(-50.,-2.56577042120647,16.4190338912104));
#60562=CARTESIAN_POINT('Ctrl Pts',(-66.,-2.50127905385604,16.3317931713189));
#60563=CARTESIAN_POINT('Ctrl Pts',(-50.,-2.50127905385604,16.3317931713189));
#60564=CARTESIAN_POINT('Ctrl Pts',(-66.,-2.43822415914769,16.244003577817));
#60565=CARTESIAN_POINT('Ctrl Pts',(-50.,-2.43822415914769,16.244003577817));
#60566=CARTESIAN_POINT('Ctrl Pts',(-66.,-2.37670786491403,16.1556609753953));
#60567=CARTESIAN_POINT('Ctrl Pts',(-50.,-2.37670786491403,16.1556609753953));
#60568=CARTESIAN_POINT('Ctrl Pts',(-66.,-2.31685613637301,16.0667562271139));
#60569=CARTESIAN_POINT('Ctrl Pts',(-50.,-2.31685613637301,16.0667562271139));
#60570=CARTESIAN_POINT('Ctrl Pts',(-66.,-2.25878765825938,15.9772806643205));
#60571=CARTESIAN_POINT('Ctrl Pts',(-50.,-2.25878765825938,15.9772806643205));
#60572=CARTESIAN_POINT('Ctrl Pts',(-66.,-2.20258303257508,15.8872314185123));
#60573=CARTESIAN_POINT('Ctrl Pts',(-50.,-2.20258303257508,15.8872314185123));
#60574=CARTESIAN_POINT('Ctrl Pts',(-66.,-2.14825922908453,15.7966159569104));
#60575=CARTESIAN_POINT('Ctrl Pts',(-50.,-2.14825922908453,15.7966159569104));
#60576=CARTESIAN_POINT('Ctrl Pts',(-66.,-2.09572657992989,15.7054594872874));
#60577=CARTESIAN_POINT('Ctrl Pts',(-50.,-2.09572657992989,15.7054594872874));
#60578=CARTESIAN_POINT('Ctrl Pts',(-66.,-2.04484013524158,15.6137968955554));
#60579=CARTESIAN_POINT('Ctrl Pts',(-50.,-2.04484013524158,15.6137968955554));
#60580=CARTESIAN_POINT('Ctrl Pts',(-66.,-1.99548217379509,15.5216595832348));
#60581=CARTESIAN_POINT('Ctrl Pts',(-50.,-1.99548217379509,15.5216595832348));
#60582=CARTESIAN_POINT('Ctrl Pts',(-66.,-1.94763938741864,15.4290632100973));
#60583=CARTESIAN_POINT('Ctrl Pts',(-50.,-1.94763938741864,15.4290632100973));
#60584=CARTESIAN_POINT('Ctrl Pts',(-66.,-1.901471233747,15.3359968987161));
#60585=CARTESIAN_POINT('Ctrl Pts',(-50.,-1.901471233747,15.3359968987161));
#60586=CARTESIAN_POINT('Ctrl Pts',(-66.,-1.85741167873706,15.2424070113801));
#60587=CARTESIAN_POINT('Ctrl Pts',(-50.,-1.85741167873706,15.2424070113801));
#60588=CARTESIAN_POINT('Ctrl Pts',(-66.,-1.81608156923822,15.1482118634974));
#60589=CARTESIAN_POINT('Ctrl Pts',(-50.,-1.81608156923822,15.1482118634974));
#60590=CARTESIAN_POINT('Ctrl Pts',(-66.,-1.77813692730802,15.0533268835806));
#60591=CARTESIAN_POINT('Ctrl Pts',(-50.,-1.77813692730802,15.0533268835806));
#60592=CARTESIAN_POINT('Ctrl Pts',(-66.,-1.74413304367239,14.957687298555));
#60593=CARTESIAN_POINT('Ctrl Pts',(-50.,-1.74413304367239,14.957687298555));
#60594=CARTESIAN_POINT('Ctrl Pts',(-66.,-1.71439340426661,14.8612698707291));
#60595=CARTESIAN_POINT('Ctrl Pts',(-50.,-1.71439340426661,14.8612698707291));
#60596=CARTESIAN_POINT('Ctrl Pts',(-66.,-1.68884359201954,14.7641208448459));
#60597=CARTESIAN_POINT('Ctrl Pts',(-50.,-1.68884359201954,14.7641208448459));
#60598=CARTESIAN_POINT('Ctrl Pts',(-66.,-1.66708743757887,14.6663413378531));
#60599=CARTESIAN_POINT('Ctrl Pts',(-50.,-1.66708743757887,14.6663413378531));
#60600=CARTESIAN_POINT('Ctrl Pts',(-66.,-1.64854533029309,14.5680618357278));
#60601=CARTESIAN_POINT('Ctrl Pts',(-50.,-1.64854533029309,14.5680618357278));
#60602=CARTESIAN_POINT('Ctrl Pts',(-66.,-1.63257174420173,14.4694202802978));
#60603=CARTESIAN_POINT('Ctrl Pts',(-50.,-1.63257174420173,14.4694202802978));
#60604=CARTESIAN_POINT('Ctrl Pts',(-66.,-1.61857609759037,14.3705396469258));
#60605=CARTESIAN_POINT('Ctrl Pts',(-50.,-1.61857609759037,14.3705396469258));
#60606=CARTESIAN_POINT('Ctrl Pts',(-66.,-1.60615369222193,14.2715034719842));
#60607=CARTESIAN_POINT('Ctrl Pts',(-50.,-1.60615369222193,14.2715034719842));
#60608=CARTESIAN_POINT('Ctrl Pts',(-66.,-1.59506091439902,14.1723615147133));
#60609=CARTESIAN_POINT('Ctrl Pts',(-50.,-1.59506091439902,14.1723615147133));
#60610=CARTESIAN_POINT('Ctrl Pts',(-66.,-1.58714954409268,14.0929835088213));
#60611=CARTESIAN_POINT('Ctrl Pts',(-50.,-1.58714954409268,14.0929835088213));
#60612=CARTESIAN_POINT('Ctrl Pts',(-66.,-1.58173749645856,14.0334175928621));
#60613=CARTESIAN_POINT('Ctrl Pts',(-50.,-1.58173749645856,14.0334175928621));
#60614=CARTESIAN_POINT('Ctrl Pts',(-66.,-1.57836090671277,13.9936925998767));
#60615=CARTESIAN_POINT('Ctrl Pts',(-50.,-1.57836090671277,13.9936925998767));
#60616=CARTESIAN_POINT('Ctrl Pts',(-66.,-1.57673047345591,13.9738265075847));
#60617=CARTESIAN_POINT('Ctrl Pts',(-50.,-1.57673047345591,13.9738265075847));
#60618=CARTESIAN_POINT('Origin',(-65.75,0.,0.));
#60619=CARTESIAN_POINT('',(-65.5,1.48114719470812,16.8098729319293));
#60620=CARTESIAN_POINT('Origin',(-65.5,0.,0.));
#60621=CARTESIAN_POINT('Ctrl Pts',(-65.5,1.48114719470739,16.8098729319309));
#60622=CARTESIAN_POINT('Ctrl Pts',(-65.5830891893357,1.52065903745123,16.7229860401592));
#60623=CARTESIAN_POINT('Ctrl Pts',(-65.6667904343355,1.55870578833828,16.6354130562452));
#60624=CARTESIAN_POINT('Ctrl Pts',(-65.7503687595015,1.59493615732831,16.5479535315511));
#60625=CARTESIAN_POINT('Ctrl Pts',(-65.8133591842207,1.62224187715319,16.4820379655801));
#60626=CARTESIAN_POINT('Ctrl Pts',(-65.8762797883185,1.64851836527279,16.4161878541729));
#60627=CARTESIAN_POINT('Ctrl Pts',(-65.9388159306751,1.6735755621829,16.3507588674798));
#60628=CARTESIAN_POINT('Ctrl Pts',(-65.959255352681,1.68176530019086,16.3293739431778));
#60629=CARTESIAN_POINT('Ctrl Pts',(-65.9796537043586,1.68982432280954,16.3080340818493));
#60630=CARTESIAN_POINT('Ctrl Pts',(-66.,1.69774526472952,16.2867518559131));
#60631=CARTESIAN_POINT('Origin',(-58.,0.,0.));
#60632=CARTESIAN_POINT('',(-50.5,1.48114719470812,16.8098729319293));
#60633=CARTESIAN_POINT('Origin',(-50.5,0.,0.));
#60634=CARTESIAN_POINT('Ctrl Pts',(-50.5,1.48114719470812,16.8098729319293));
#60635=CARTESIAN_POINT('Ctrl Pts',(-55.5,1.48114719470812,16.8098729319293));
#60636=CARTESIAN_POINT('Ctrl Pts',(-60.5,1.48114719470812,16.8098729319293));
#60637=CARTESIAN_POINT('Ctrl Pts',(-65.5,1.48114719470812,16.8098729319293));
#60638=CARTESIAN_POINT('Origin',(-50.25,0.,0.));
#60639=CARTESIAN_POINT('Ctrl Pts',(-50.,1.69774526472952,16.2867518559131));
#60640=CARTESIAN_POINT('Ctrl Pts',(-50.0661278995916,1.67200125406601,16.3559216411457));
#60641=CARTESIAN_POINT('Ctrl Pts',(-50.132805681623,1.64480114704281,16.4256996735367));
#60642=CARTESIAN_POINT('Ctrl Pts',(-50.1996561856134,1.61638854466487,16.4956567269383));
#60643=CARTESIAN_POINT('Ctrl Pts',(-50.275508769232,1.58414990517748,16.5750341874825));
#60644=CARTESIAN_POINT('Ctrl Pts',(-50.3515837242552,1.55034920906213,16.6546411368507));
#60645=CARTESIAN_POINT('Ctrl Pts',(-50.4273300866396,1.51525802335958,16.7338710346662));
#60646=CARTESIAN_POINT('Ctrl Pts',(-50.4515931423099,1.5040176236171,16.7592499355262));
#60647=CARTESIAN_POINT('Ctrl Pts',(-50.4758224828177,1.49264445763884,16.7845903490235));
#60648=CARTESIAN_POINT('Ctrl Pts',(-50.5,1.48114719470371,16.809872931939));
#60649=CARTESIAN_POINT('Ctrl Pts',(-66.,3.31568234418832,13.6660219830951));
#60650=CARTESIAN_POINT('Ctrl Pts',(-50.,3.31568234418832,13.6660219830951));
#60651=CARTESIAN_POINT('Ctrl Pts',(-66.,3.32025508218772,13.6889423777435));
#60652=CARTESIAN_POINT('Ctrl Pts',(-50.,3.32025508218772,13.6889423777435));
#60653=CARTESIAN_POINT('Ctrl Pts',(-66.,3.32962290369722,13.7347480949923));
#60654=CARTESIAN_POINT('Ctrl Pts',(-50.,3.32962290369722,13.7347480949923));
#60655=CARTESIAN_POINT('Ctrl Pts',(-66.,3.34434166251121,13.8033514635997));
#60656=CARTESIAN_POINT('Ctrl Pts',(-50.,3.34434166251121,13.8033514635997));
#60657=CARTESIAN_POINT('Ctrl Pts',(-66.,3.36530258749166,13.8946118507282));
#60658=CARTESIAN_POINT('Ctrl Pts',(-50.,3.36530258749166,13.8946118507282));
#60659=CARTESIAN_POINT('Ctrl Pts',(-66.,3.39378048711278,14.0083089910501));
#60660=CARTESIAN_POINT('Ctrl Pts',(-50.,3.39378048711278,14.0083089910501));
#60661=CARTESIAN_POINT('Ctrl Pts',(-66.,3.42466963349977,14.1215479032503));
#60662=CARTESIAN_POINT('Ctrl Pts',(-50.,3.42466963349977,14.1215479032503));
#60663=CARTESIAN_POINT('Ctrl Pts',(-66.,3.45822302631379,14.2341732241738));
#60664=CARTESIAN_POINT('Ctrl Pts',(-50.,3.45822302631379,14.2341732241738));
#60665=CARTESIAN_POINT('Ctrl Pts',(-66.,3.49485794879717,14.3459208356842));
#60666=CARTESIAN_POINT('Ctrl Pts',(-50.,3.49485794879717,14.3459208356842));
#60667=CARTESIAN_POINT('Ctrl Pts',(-66.,3.53511610244324,14.4564721136477));
#60668=CARTESIAN_POINT('Ctrl Pts',(-50.,3.53511610244324,14.4564721136477));
#60669=CARTESIAN_POINT('Ctrl Pts',(-66.,3.57961415137445,14.5655275456869));
#60670=CARTESIAN_POINT('Ctrl Pts',(-50.,3.57961415137445,14.5655275456869));
#60671=CARTESIAN_POINT('Ctrl Pts',(-66.,3.62898699781003,14.6728671135607));
#60672=CARTESIAN_POINT('Ctrl Pts',(-50.,3.62898699781003,14.6728671135607));
#60673=CARTESIAN_POINT('Ctrl Pts',(-66.,3.68386053504292,14.7784329430806));
#60674=CARTESIAN_POINT('Ctrl Pts',(-50.,3.68386053504292,14.7784329430806));
#60675=CARTESIAN_POINT('Ctrl Pts',(-66.,3.74465444426779,14.8823190942953));
#60676=CARTESIAN_POINT('Ctrl Pts',(-50.,3.74465444426779,14.8823190942953));
#60677=CARTESIAN_POINT('Ctrl Pts',(-66.,3.81125317193191,14.9847182617076));
#60678=CARTESIAN_POINT('Ctrl Pts',(-50.,3.81125317193191,14.9847182617076));
#60679=CARTESIAN_POINT('Ctrl Pts',(-66.,3.88279556209739,15.0858821011164));
#60680=CARTESIAN_POINT('Ctrl Pts',(-50.,3.88279556209739,15.0858821011164));
#60681=CARTESIAN_POINT('Ctrl Pts',(-66.,3.95722328533246,15.1860781064647));
#60682=CARTESIAN_POINT('Ctrl Pts',(-50.,3.95722328533246,15.1860781064647));
#60683=CARTESIAN_POINT('Ctrl Pts',(-66.,4.03163457417435,15.2855414194547));
#60684=CARTESIAN_POINT('Ctrl Pts',(-50.,4.03163457417435,15.2855414194547));
#60685=CARTESIAN_POINT('Ctrl Pts',(-66.,4.10369589439471,15.3844104249513));
#60686=CARTESIAN_POINT('Ctrl Pts',(-50.,4.10369589439471,15.3844104249513));
#60687=CARTESIAN_POINT('Ctrl Pts',(-66.,4.17266875139903,15.482674151341));
#60688=CARTESIAN_POINT('Ctrl Pts',(-50.,4.17266875139903,15.482674151341));
#60689=CARTESIAN_POINT('Ctrl Pts',(-66.,4.24085733833789,15.5800968628044));
#60690=CARTESIAN_POINT('Ctrl Pts',(-50.,4.24085733833789,15.5800968628044));
#60691=CARTESIAN_POINT('Ctrl Pts',(-66.,4.31412149748944,15.6762031957635));
#60692=CARTESIAN_POINT('Ctrl Pts',(-50.,4.31412149748944,15.6762031957635));
#60693=CARTESIAN_POINT('Ctrl Pts',(-66.,4.3986379872848,15.7705164726843));
#60694=CARTESIAN_POINT('Ctrl Pts',(-50.,4.3986379872848,15.7705164726843));
#60695=CARTESIAN_POINT('Ctrl Pts',(-66.,4.4981307922185,15.862765781002));
#60696=CARTESIAN_POINT('Ctrl Pts',(-50.,4.4981307922185,15.862765781002));
#60697=CARTESIAN_POINT('Ctrl Pts',(-66.,4.61104471950514,15.9530958995951));
#60698=CARTESIAN_POINT('Ctrl Pts',(-50.,4.61104471950514,15.9530958995951));
#60699=CARTESIAN_POINT('Ctrl Pts',(-66.,4.72735495944251,16.0423056749486));
#60700=CARTESIAN_POINT('Ctrl Pts',(-50.,4.72735495944251,16.0423056749486));
#60701=CARTESIAN_POINT('Ctrl Pts',(-66.,4.83101568214621,16.1316580433923));
#60702=CARTESIAN_POINT('Ctrl Pts',(-50.,4.83101568214621,16.1316580433923));
#60703=CARTESIAN_POINT('Ctrl Pts',(-66.,4.9030763374662,16.2226394544667));
#60704=CARTESIAN_POINT('Ctrl Pts',(-50.,4.9030763374662,16.2226394544667));
#60705=CARTESIAN_POINT('Ctrl Pts',(-66.,4.92433124236172,16.3167550432627));
#60706=CARTESIAN_POINT('Ctrl Pts',(-50.,4.92433124236172,16.3167550432627));
#60707=CARTESIAN_POINT('Ctrl Pts',(-66.,4.87866379252586,16.4152704420741));
#60708=CARTESIAN_POINT('Ctrl Pts',(-50.,4.87866379252586,16.4152704420741));
#60709=CARTESIAN_POINT('Ctrl Pts',(-66.,4.75394565180326,16.5191420918161));
#60710=CARTESIAN_POINT('Ctrl Pts',(-50.,4.75394565180326,16.5191420918161));
#60711=CARTESIAN_POINT('Ctrl Pts',(-66.,4.54114089813183,16.629086018864));
#60712=CARTESIAN_POINT('Ctrl Pts',(-50.,4.54114089813183,16.629086018864));
#60713=CARTESIAN_POINT('Ctrl Pts',(-66.,4.23395401208117,16.7456047287692));
#60714=CARTESIAN_POINT('Ctrl Pts',(-50.,4.23395401208117,16.7456047287692));
#60715=CARTESIAN_POINT('Ctrl Pts',(-66.,3.82828013317778,16.8690293990345));
#60716=CARTESIAN_POINT('Ctrl Pts',(-50.,3.82828013317778,16.8690293990345));
#60717=CARTESIAN_POINT('Ctrl Pts',(-66.,3.32176445468909,16.9995537049453));
#60718=CARTESIAN_POINT('Ctrl Pts',(-50.,3.32176445468909,16.9995537049453));
#60719=CARTESIAN_POINT('Ctrl Pts',(-66.,2.7133369168573,17.1372695974412));
#60720=CARTESIAN_POINT('Ctrl Pts',(-50.,2.7133369168573,17.1372695974412));
#60721=CARTESIAN_POINT('Ctrl Pts',(-66.,2.14488947489857,17.2532145262309));
#60722=CARTESIAN_POINT('Ctrl Pts',(-50.,2.14488947489857,17.2532145262309));
#60723=CARTESIAN_POINT('Ctrl Pts',(-66.,1.67268460782871,17.3434149530381));
#60724=CARTESIAN_POINT('Ctrl Pts',(-50.,1.67268460782871,17.3434149530381));
#60725=CARTESIAN_POINT('Ctrl Pts',(-66.,1.33752212890223,17.4049874234484));
#60726=CARTESIAN_POINT('Ctrl Pts',(-50.,1.33752212890223,17.4049874234484));
#60727=CARTESIAN_POINT('Ctrl Pts',(-66.,1.16485107862945,17.4361333719554));
#60728=CARTESIAN_POINT('Ctrl Pts',(-50.,1.16485107862945,17.4361333719554));
#60729=CARTESIAN_POINT('',(-65.5,4.85049230558631,16.1628694665721));
#60730=CARTESIAN_POINT('Ctrl Pts',(-66.,4.40398464539872,15.7716690379646));
#60731=CARTESIAN_POINT('Ctrl Pts',(-65.7933280154034,4.57046489538325,15.9397601433951));
#60732=CARTESIAN_POINT('Ctrl Pts',(-65.637076174949,4.75647091834925,16.0479696685658));
#60733=CARTESIAN_POINT('Ctrl Pts',(-65.5,4.85049230558631,16.1628694665721));
#60734=CARTESIAN_POINT('',(-66.,3.31568234418832,13.6660219830951));
#60735=CARTESIAN_POINT('',(-50.5,4.85049230558631,16.1628694665721));
#60736=CARTESIAN_POINT('Ctrl Pts',(-50.5,4.85049230558631,16.1628694665721));
#60737=CARTESIAN_POINT('Ctrl Pts',(-50.4457232578825,4.81326355602069,16.1173736923571));
#60738=CARTESIAN_POINT('Ctrl Pts',(-50.3881125476901,4.76170358838096,16.0726383675736));
#60739=CARTESIAN_POINT('Ctrl Pts',(-50.2297317785044,4.61214589079611,15.951491103014));
#60740=CARTESIAN_POINT('Ctrl Pts',(-50.1279794591276,4.50707579435166,15.8757576922597));
#60741=CARTESIAN_POINT('Ctrl Pts',(-50.,4.40398464539871,15.7716690379646));
#60742=CARTESIAN_POINT('Ctrl Pts',(-65.5,4.85049230558631,16.1628694665721));
#60743=CARTESIAN_POINT('Ctrl Pts',(-60.5,4.85049230558631,16.1628694665721));
#60744=CARTESIAN_POINT('Ctrl Pts',(-55.5,4.85049230558631,16.1628694665721));
#60745=CARTESIAN_POINT('Ctrl Pts',(-50.5,4.85049230558631,16.1628694665721));
#60746=CARTESIAN_POINT('Origin',(-66.,0.,0.));
#60747=CARTESIAN_POINT('',(-66.,1.94795475120473,13.9269299753125));
#60748=CARTESIAN_POINT('Ctrl Pts',(-66.,1.16485107862945,17.4361333719554));
#60749=CARTESIAN_POINT('Ctrl Pts',(-50.,1.16485107862945,17.4361333719554));
#60750=CARTESIAN_POINT('Ctrl Pts',(-66.,1.17579024097006,17.4164609164663));
#60751=CARTESIAN_POINT('Ctrl Pts',(-50.,1.17579024097006,17.4164609164663));
#60752=CARTESIAN_POINT('Ctrl Pts',(-66.,1.19752267929878,17.3770919187696));
#60753=CARTESIAN_POINT('Ctrl Pts',(-50.,1.19752267929878,17.3770919187696));
#60754=CARTESIAN_POINT('Ctrl Pts',(-66.,1.22968367840899,17.3179661621208));
#60755=CARTESIAN_POINT('Ctrl Pts',(-50.,1.22968367840899,17.3179661621208));
#60756=CARTESIAN_POINT('Ctrl Pts',(-66.,1.2716885238945,17.2389871070698));
#60757=CARTESIAN_POINT('Ctrl Pts',(-50.,1.2716885238945,17.2389871070698));
#60758=CARTESIAN_POINT('Ctrl Pts',(-66.,1.32272773816582,17.1400214191551));
#60759=CARTESIAN_POINT('Ctrl Pts',(-50.,1.32272773816582,17.1400214191551));
#60760=CARTESIAN_POINT('Ctrl Pts',(-66.,1.37229367622044,17.040813755223));
#60761=CARTESIAN_POINT('Ctrl Pts',(-50.,1.37229367622044,17.040813755223));
#60762=CARTESIAN_POINT('Ctrl Pts',(-66.,1.42038260159604,16.9413653958879));
#60763=CARTESIAN_POINT('Ctrl Pts',(-50.,1.42038260159604,16.9413653958879));
#60764=CARTESIAN_POINT('Ctrl Pts',(-66.,1.46699609707973,16.8416798096044));
#60765=CARTESIAN_POINT('Ctrl Pts',(-50.,1.46699609707973,16.8416798096044));
#60766=CARTESIAN_POINT('Ctrl Pts',(-66.,1.51214539242291,16.7417635820299));
#60767=CARTESIAN_POINT('Ctrl Pts',(-50.,1.51214539242291,16.7417635820299));
#60768=CARTESIAN_POINT('Ctrl Pts',(-66.,1.55584180188614,16.6416264021506));
#60769=CARTESIAN_POINT('Ctrl Pts',(-50.,1.55584180188614,16.6416264021506));
#60770=CARTESIAN_POINT('Ctrl Pts',(-66.,1.59808566045853,16.5412809055674));
#60771=CARTESIAN_POINT('Ctrl Pts',(-50.,1.59808566045853,16.5412809055674));
#60772=CARTESIAN_POINT('Ctrl Pts',(-66.,1.63885502812633,16.4407426624463));
#60773=CARTESIAN_POINT('Ctrl Pts',(-50.,1.63885502812633,16.4407426624463));
#60774=CARTESIAN_POINT('Ctrl Pts',(-66.,1.67809655326534,16.3400300258078));
#60775=CARTESIAN_POINT('Ctrl Pts',(-50.,1.67809655326534,16.3400300258078));
#60776=CARTESIAN_POINT('Ctrl Pts',(-66.,1.71571028816699,16.2391643884201));
#60777=CARTESIAN_POINT('Ctrl Pts',(-50.,1.71571028816699,16.2391643884201));
#60778=CARTESIAN_POINT('Ctrl Pts',(-66.,1.75157195277774,16.1381682266729));
#60779=CARTESIAN_POINT('Ctrl Pts',(-50.,1.75157195277774,16.1381682266729));
#60780=CARTESIAN_POINT('Ctrl Pts',(-66.,1.78556443525587,16.0370626599488));
#60781=CARTESIAN_POINT('Ctrl Pts',(-50.,1.78556443525587,16.0370626599488));
#60782=CARTESIAN_POINT('Ctrl Pts',(-66.,1.8176089524919,15.9358649547671));
#60783=CARTESIAN_POINT('Ctrl Pts',(-50.,1.8176089524919,15.9358649547671));
#60784=CARTESIAN_POINT('Ctrl Pts',(-66.,1.84769092488014,15.8345865639611));
#60785=CARTESIAN_POINT('Ctrl Pts',(-50.,1.84769092488014,15.8345865639611));
#60786=CARTESIAN_POINT('Ctrl Pts',(-66.,1.87590347211591,15.7332296038656));
#60787=CARTESIAN_POINT('Ctrl Pts',(-50.,1.87590347211591,15.7332296038656));
#60788=CARTESIAN_POINT('Ctrl Pts',(-66.,1.90239566597564,15.6317918168208));
#60789=CARTESIAN_POINT('Ctrl Pts',(-50.,1.90239566597564,15.6317918168208));
#60790=CARTESIAN_POINT('Ctrl Pts',(-66.,1.92728933849566,15.5302743417326));
#60791=CARTESIAN_POINT('Ctrl Pts',(-50.,1.92728933849566,15.5302743417326));
#60792=CARTESIAN_POINT('Ctrl Pts',(-66.,1.95060127417394,15.4286890367845));
#60793=CARTESIAN_POINT('Ctrl Pts',(-50.,1.95060127417394,15.4286890367845));
#60794=CARTESIAN_POINT('Ctrl Pts',(-66.,1.97217431992445,15.3270650217851));
#60795=CARTESIAN_POINT('Ctrl Pts',(-50.,1.97217431992445,15.3270650217851));
#60796=CARTESIAN_POINT('Ctrl Pts',(-66.,1.99157480447254,15.2254582670956));
#60797=CARTESIAN_POINT('Ctrl Pts',(-50.,1.99157480447254,15.2254582670956));
#60798=CARTESIAN_POINT('Ctrl Pts',(-66.,2.00818107188229,15.1239440527286));
#60799=CARTESIAN_POINT('Ctrl Pts',(-50.,2.00818107188229,15.1239440527286));
#60800=CARTESIAN_POINT('Ctrl Pts',(-66.,2.02133667816179,15.022603610217));
#60801=CARTESIAN_POINT('Ctrl Pts',(-50.,2.02133667816179,15.022603610217));
#60802=CARTESIAN_POINT('Ctrl Pts',(-66.,2.03048766965571,14.9215122966393));
#60803=CARTESIAN_POINT('Ctrl Pts',(-50.,2.03048766965571,14.9215122966393));
#60804=CARTESIAN_POINT('Ctrl Pts',(-66.,2.03531494435546,14.8207280520398));
#60805=CARTESIAN_POINT('Ctrl Pts',(-50.,2.03531494435546,14.8207280520398));
#60806=CARTESIAN_POINT('Ctrl Pts',(-66.,2.03590208198289,14.7202771615244));
#60807=CARTESIAN_POINT('Ctrl Pts',(-50.,2.03590208198289,14.7202771615244));
#60808=CARTESIAN_POINT('Ctrl Pts',(-66.,2.03265795226397,14.6201590419547));
#60809=CARTESIAN_POINT('Ctrl Pts',(-50.,2.03265795226397,14.6201590419547));
#60810=CARTESIAN_POINT('Ctrl Pts',(-66.,2.02617640685866,14.5203559365434));
#60811=CARTESIAN_POINT('Ctrl Pts',(-50.,2.02617640685866,14.5203559365434));
#60812=CARTESIAN_POINT('Ctrl Pts',(-66.,2.01711699607993,14.4208409176437));
#60813=CARTESIAN_POINT('Ctrl Pts',(-50.,2.01711699607993,14.4208409176437));
#60814=CARTESIAN_POINT('Ctrl Pts',(-66.,2.00608233016073,14.3215862254212));
#60815=CARTESIAN_POINT('Ctrl Pts',(-50.,2.00608233016073,14.3215862254212));
#60816=CARTESIAN_POINT('Ctrl Pts',(-66.,1.99348516764985,14.2225721274408));
#60817=CARTESIAN_POINT('Ctrl Pts',(-50.,1.99348516764985,14.2225721274408));
#60818=CARTESIAN_POINT('Ctrl Pts',(-66.,1.97957384329226,14.1237862354018));
#60819=CARTESIAN_POINT('Ctrl Pts',(-50.,1.97957384329226,14.1237862354018));
#60820=CARTESIAN_POINT('Ctrl Pts',(-66.,1.96749615602378,14.044934557742));
#60821=CARTESIAN_POINT('Ctrl Pts',(-50.,1.96749615602378,14.044934557742));
#60822=CARTESIAN_POINT('Ctrl Pts',(-66.,1.95792473331065,13.9858940930512));
#60823=CARTESIAN_POINT('Ctrl Pts',(-50.,1.95792473331065,13.9858940930512));
#60824=CARTESIAN_POINT('Ctrl Pts',(-66.,1.9513160372573,13.9465774100468));
#60825=CARTESIAN_POINT('Ctrl Pts',(-50.,1.9513160372573,13.9465774100468));
#60826=CARTESIAN_POINT('Ctrl Pts',(-66.,1.94795475120472,13.9269299753125));
#60827=CARTESIAN_POINT('Ctrl Pts',(-50.,1.94795475120472,13.9269299753125));
#60828=CARTESIAN_POINT('Origin',(-65.75,0.,0.));
#60829=CARTESIAN_POINT('',(-65.5,5.61505963464423,15.9134135338522));
#60830=CARTESIAN_POINT('Origin',(-65.5,0.,0.));
#60831=CARTESIAN_POINT('Ctrl Pts',(-65.5,5.61505963464423,15.9134135338522));
#60832=CARTESIAN_POINT('Ctrl Pts',(-65.6931595476746,5.65379827034173,15.6949131405067));
#60833=CARTESIAN_POINT('Ctrl Pts',(-65.861125696709,5.67851717118329,15.507005686362));
#60834=CARTESIAN_POINT('Ctrl Pts',(-66.,5.69475795663189,15.3528615187976));
#60835=CARTESIAN_POINT('Origin',(-58.,0.,0.));
#60836=CARTESIAN_POINT('',(-50.5,5.61505963464423,15.9134135338522));
#60837=CARTESIAN_POINT('Origin',(-50.5,0.,0.));
#60838=CARTESIAN_POINT('Ctrl Pts',(-50.5,5.61505963464423,15.9134135338522));
#60839=CARTESIAN_POINT('Ctrl Pts',(-55.5,5.61505963464423,15.9134135338522));
#60840=CARTESIAN_POINT('Ctrl Pts',(-60.5,5.61505963464423,15.9134135338522));
#60841=CARTESIAN_POINT('Ctrl Pts',(-65.5,5.61505963464423,15.9134135338522));
#60842=CARTESIAN_POINT('Origin',(-50.25,0.,0.));
#60843=CARTESIAN_POINT('Ctrl Pts',(-50.,5.69475795663189,15.3528615187977));
#60844=CARTESIAN_POINT('Ctrl Pts',(-50.1388743032898,5.67851717118344,15.5070056863606));
#60845=CARTESIAN_POINT('Ctrl Pts',(-50.3068404523242,5.65379827034194,15.6949131405054));
#60846=CARTESIAN_POINT('Ctrl Pts',(-50.5,5.61505963464423,15.9134135338522));
#60847=CARTESIAN_POINT('Ctrl Pts',(-66.,6.61011555120064,12.4121021043889));
#60848=CARTESIAN_POINT('Ctrl Pts',(-50.,6.61011555120064,12.4121021043889));
#60849=CARTESIAN_POINT('Ctrl Pts',(-66.,6.62024469858602,12.4331652189947));
#60850=CARTESIAN_POINT('Ctrl Pts',(-50.,6.62024469858602,12.4331652189947));
#60851=CARTESIAN_POINT('Ctrl Pts',(-66.,6.64070963141069,12.4752021829311));
#60852=CARTESIAN_POINT('Ctrl Pts',(-50.,6.64070963141069,12.4752021829311));
#60853=CARTESIAN_POINT('Ctrl Pts',(-66.,6.67202693734873,12.5379898440923));
#60854=CARTESIAN_POINT('Ctrl Pts',(-50.,6.67202693734873,12.5379898440923));
#60855=CARTESIAN_POINT('Ctrl Pts',(-66.,6.71502487170408,12.6211703482748));
#60856=CARTESIAN_POINT('Ctrl Pts',(-50.,6.71502487170408,12.6211703482748));
#60857=CARTESIAN_POINT('Ctrl Pts',(-66.,6.77088341473902,12.7242133182155));
#60858=CARTESIAN_POINT('Ctrl Pts',(-50.,6.77088341473902,12.7242133182155));
#60859=CARTESIAN_POINT('Ctrl Pts',(-66.,6.82896349408885,12.8262128034276));
#60860=CARTESIAN_POINT('Ctrl Pts',(-50.,6.82896349408885,12.8262128034276));
#60861=CARTESIAN_POINT('Ctrl Pts',(-66.,6.88947152371961,12.9269554033179));
#60862=CARTESIAN_POINT('Ctrl Pts',(-50.,6.88947152371961,12.9269554033179));
#60863=CARTESIAN_POINT('Ctrl Pts',(-66.,6.95274599364373,13.0260815233846));
#60864=CARTESIAN_POINT('Ctrl Pts',(-50.,6.95274599364373,13.0260815233846));
#60865=CARTESIAN_POINT('Ctrl Pts',(-66.,7.01923234820612,13.1231478339735));
#60866=CARTESIAN_POINT('Ctrl Pts',(-50.,7.01923234820612,13.1231478339735));
#60867=CARTESIAN_POINT('Ctrl Pts',(-66.,7.08945339219251,13.2177108743086));
#60868=CARTESIAN_POINT('Ctrl Pts',(-50.,7.08945339219251,13.2177108743086));
#60869=CARTESIAN_POINT('Ctrl Pts',(-66.,7.16396936488986,13.3093996446649));
#60870=CARTESIAN_POINT('Ctrl Pts',(-50.,7.16396936488986,13.3093996446649));
#60871=CARTESIAN_POINT('Ctrl Pts',(-66.,7.24337210327696,13.3980024357456));
#60872=CARTESIAN_POINT('Ctrl Pts',(-50.,7.24337210327696,13.3980024357456));
#60873=CARTESIAN_POINT('Ctrl Pts',(-66.,7.32809149527493,13.4835059820612));
#60874=CARTESIAN_POINT('Ctrl Pts',(-50.,7.32809149527493,13.4835059820612));
#60875=CARTESIAN_POINT('Ctrl Pts',(-66.,7.41806353883254,13.5661256612623));
#60876=CARTESIAN_POINT('Ctrl Pts',(-50.,7.41806353883254,13.5661256612623));
#60877=CARTESIAN_POINT('Ctrl Pts',(-66.,7.51251671706145,13.646319383691));
#60878=CARTESIAN_POINT('Ctrl Pts',(-50.,7.51251671706145,13.646319383691));
#60879=CARTESIAN_POINT('Ctrl Pts',(-66.,7.60952388977251,13.7248581251904));
#60880=CARTESIAN_POINT('Ctrl Pts',(-50.,7.60952388977251,13.7248581251904));
#60881=CARTESIAN_POINT('Ctrl Pts',(-66.,7.70633293122716,13.8026912802767));
#60882=CARTESIAN_POINT('Ctrl Pts',(-50.,7.70633293122716,13.8026912802767));
#60883=CARTESIAN_POINT('Ctrl Pts',(-66.,7.80071803438238,13.8805332125637));
#60884=CARTESIAN_POINT('Ctrl Pts',(-50.,7.80071803438238,13.8805332125637));
#60885=CARTESIAN_POINT('Ctrl Pts',(-66.,7.89196117727994,13.9585569512687));
#60886=CARTESIAN_POINT('Ctrl Pts',(-50.,7.89196117727994,13.9585569512687));
#60887=CARTESIAN_POINT('Ctrl Pts',(-66.,7.9822355374912,14.0359611371119));
#60888=CARTESIAN_POINT('Ctrl Pts',(-50.,7.9822355374912,14.0359611371119));
#60889=CARTESIAN_POINT('Ctrl Pts',(-66.,8.07709864145905,14.1108280574212));
#60890=CARTESIAN_POINT('Ctrl Pts',(-50.,8.07709864145905,14.1108280574212));
#60891=CARTESIAN_POINT('Ctrl Pts',(-66.,8.18241464850812,14.1811599130068));
#60892=CARTESIAN_POINT('Ctrl Pts',(-50.,8.18241464850812,14.1811599130068));
#60893=CARTESIAN_POINT('Ctrl Pts',(-66.,8.30172317409692,14.2457681852364));
#60894=CARTESIAN_POINT('Ctrl Pts',(-50.,8.30172317409692,14.2457681852364));
#60895=CARTESIAN_POINT('Ctrl Pts',(-66.,8.43355388972419,14.3051798652122));
#60896=CARTESIAN_POINT('Ctrl Pts',(-50.,8.43355388972419,14.3051798652122));
#60897=CARTESIAN_POINT('Ctrl Pts',(-66.,8.56839559856102,14.3626617709815));
#60898=CARTESIAN_POINT('Ctrl Pts',(-50.,8.56839559856102,14.3626617709815));
#60899=CARTESIAN_POINT('Ctrl Pts',(-66.,8.69102065946842,14.4234275970304));
#60900=CARTESIAN_POINT('Ctrl Pts',(-50.,8.69102065946842,14.4234275970304));
#60901=CARTESIAN_POINT('Ctrl Pts',(-66.,8.78344355364544,14.4936299035323));
#60902=CARTESIAN_POINT('Ctrl Pts',(-50.,8.78344355364544,14.4936299035323));
#60903=CARTESIAN_POINT('Ctrl Pts',(-66.,8.82743629177677,14.5795027981396));
#60904=CARTESIAN_POINT('Ctrl Pts',(-50.,8.82743629177677,14.5795027981396));
#60905=CARTESIAN_POINT('Ctrl Pts',(-66.,8.80770335226846,14.686280187487));
#60906=CARTESIAN_POINT('Ctrl Pts',(-50.,8.80770335226846,14.686280187487));
#60907=CARTESIAN_POINT('Ctrl Pts',(-66.,8.71273529013126,14.8179046586894));
#60908=CARTESIAN_POINT('Ctrl Pts',(-50.,8.71273529013126,14.8179046586894));
#60909=CARTESIAN_POINT('Ctrl Pts',(-66.,8.53395813192898,14.9773168852751));
#60910=CARTESIAN_POINT('Ctrl Pts',(-50.,8.53395813192898,14.9773168852751));
#60911=CARTESIAN_POINT('Ctrl Pts',(-66.,8.2653991115997,15.1665692176762));
#60912=CARTESIAN_POINT('Ctrl Pts',(-50.,8.2653991115997,15.1665692176762));
#60913=CARTESIAN_POINT('Ctrl Pts',(-66.,7.90316469090577,15.3870032661332));
#60914=CARTESIAN_POINT('Ctrl Pts',(-50.,7.90316469090577,15.3870032661332));
#60915=CARTESIAN_POINT('Ctrl Pts',(-66.,7.44502220878323,15.639392237887));
#60916=CARTESIAN_POINT('Ctrl Pts',(-50.,7.44502220878323,15.639392237887));
#60917=CARTESIAN_POINT('Ctrl Pts',(-66.,6.889958090638,15.9240913081097));
#60918=CARTESIAN_POINT('Ctrl Pts',(-50.,6.889958090638,15.9240913081097));
#60919=CARTESIAN_POINT('Ctrl Pts',(-66.,6.36820380162818,16.1777607439535));
#60920=CARTESIAN_POINT('Ctrl Pts',(-50.,6.36820380162818,16.1777607439535));
#60921=CARTESIAN_POINT('Ctrl Pts',(-66.,5.93326605274623,16.3825599335959));
#60922=CARTESIAN_POINT('Ctrl Pts',(-50.,5.93326605274623,16.3825599335959));
#60923=CARTESIAN_POINT('Ctrl Pts',(-66.,5.62394577013471,16.5255495106905));
#60924=CARTESIAN_POINT('Ctrl Pts',(-50.,5.62394577013471,16.5255495106905));
#60925=CARTESIAN_POINT('Ctrl Pts',(-66.,5.46444518084595,16.5986584959607));
#60926=CARTESIAN_POINT('Ctrl Pts',(-50.,5.46444518084595,16.5986584959607));
#60927=CARTESIAN_POINT('',(-65.5,8.71764735427698,14.4488148166716));
#60928=CARTESIAN_POINT('Ctrl Pts',(-66.,8.1878799628551,14.1809466085264));
#60929=CARTESIAN_POINT('Ctrl Pts',(-65.7933280154035,8.3909324876934,14.3023548681979));
#60930=CARTESIAN_POINT('Ctrl Pts',(-65.637076174949,8.59800540401177,14.3609069752887));
#60931=CARTESIAN_POINT('Ctrl Pts',(-65.5,8.71764735427698,14.4488148166716));
#60932=CARTESIAN_POINT('',(-66.,6.61011555120064,12.4121021043889));
#60933=CARTESIAN_POINT('',(-50.5,8.71764735427698,14.4488148166716));
#60934=CARTESIAN_POINT('Ctrl Pts',(-50.5,8.71764735427698,14.4488148166716));
#60935=CARTESIAN_POINT('Ctrl Pts',(-50.4518618349118,8.67563170892152,14.4179434987156));
#60936=CARTESIAN_POINT('Ctrl Pts',(-50.4012423593878,8.62299967613232,14.3905314785402));
#60937=CARTESIAN_POINT('Ctrl Pts',(-50.2441129793791,8.45124686345708,14.3100121728929));
#60938=CARTESIAN_POINT('Ctrl Pts',(-50.1366827452935,8.32216897443961,14.2612400951623));
#60939=CARTESIAN_POINT('Ctrl Pts',(-50.,8.1878799628551,14.1809466085264));
#60940=CARTESIAN_POINT('Ctrl Pts',(-65.5,8.71764735427698,14.4488148166716));
#60941=CARTESIAN_POINT('Ctrl Pts',(-60.5,8.71764735427698,14.4488148166716));
#60942=CARTESIAN_POINT('Ctrl Pts',(-55.5,8.71764735427698,14.4488148166716));
#60943=CARTESIAN_POINT('Ctrl Pts',(-50.5,8.71764735427698,14.4488148166716));
#60944=CARTESIAN_POINT('Origin',(-66.,0.,0.));
#60945=CARTESIAN_POINT('',(-66.,5.35024281477072,13.004953213026));
#60946=CARTESIAN_POINT('Ctrl Pts',(-66.,5.46444518084595,16.5986584959607));
#60947=CARTESIAN_POINT('Ctrl Pts',(-50.,5.46444518084595,16.5986584959607));
#60948=CARTESIAN_POINT('Ctrl Pts',(-66.,5.47014832855009,16.5768836277878));
#60949=CARTESIAN_POINT('Ctrl Pts',(-50.,5.47014832855009,16.5768836277878));
#60950=CARTESIAN_POINT('Ctrl Pts',(-66.,5.48140733077057,16.5333468419125));
#60951=CARTESIAN_POINT('Ctrl Pts',(-50.,5.48140733077057,16.5333468419125));
#60952=CARTESIAN_POINT('Ctrl Pts',(-66.,5.49785395520425,16.4680805143936));
#60953=CARTESIAN_POINT('Ctrl Pts',(-50.,5.49785395520425,16.4680805143936));
#60954=CARTESIAN_POINT('Ctrl Pts',(-66.,5.51889784893831,16.3811365513052));
#60955=CARTESIAN_POINT('Ctrl Pts',(-50.,5.51889784893831,16.3811365513052));
#60956=CARTESIAN_POINT('Ctrl Pts',(-66.,5.54372180667804,16.2725871160234));
#60957=CARTESIAN_POINT('Ctrl Pts',(-50.,5.54372180667804,16.2725871160234));
#60958=CARTESIAN_POINT('Ctrl Pts',(-66.,5.56705859689412,16.1641696957418));
#60959=CARTESIAN_POINT('Ctrl Pts',(-50.,5.56705859689412,16.1641696957418));
#60960=CARTESIAN_POINT('Ctrl Pts',(-66.,5.58890491898793,16.0558864600624));
#60961=CARTESIAN_POINT('Ctrl Pts',(-50.,5.58890491898793,16.0558864600624));
#60962=CARTESIAN_POINT('Ctrl Pts',(-66.,5.60926316858998,15.9477403748489));
#60963=CARTESIAN_POINT('Ctrl Pts',(-50.,5.60926316858998,15.9477403748489));
#60964=CARTESIAN_POINT('Ctrl Pts',(-66.,5.62814586043475,15.8397350261322));
#60965=CARTESIAN_POINT('Ctrl Pts',(-50.,5.62814586043475,15.8397350261322));
#60966=CARTESIAN_POINT('Ctrl Pts',(-66.,5.64556636287744,15.7318769847593));
#60967=CARTESIAN_POINT('Ctrl Pts',(-50.,5.64556636287744,15.7318769847593));
#60968=CARTESIAN_POINT('Ctrl Pts',(-66.,5.66152814272899,15.624178406052));
#60969=CARTESIAN_POINT('Ctrl Pts',(-50.,5.66152814272899,15.624178406052));
#60970=CARTESIAN_POINT('Ctrl Pts',(-66.,5.67601382140434,15.5166598272703));
#60971=CARTESIAN_POINT('Ctrl Pts',(-50.,5.67601382140434,15.5166598272703));
#60972=CARTESIAN_POINT('Ctrl Pts',(-66.,5.68897628762929,15.4093522928504));
#60973=CARTESIAN_POINT('Ctrl Pts',(-50.,5.68897628762929,15.4093522928504));
#60974=CARTESIAN_POINT('Ctrl Pts',(-66.,5.70032405390141,15.3023013794516));
#60975=CARTESIAN_POINT('Ctrl Pts',(-50.,5.70032405390141,15.3023013794516));
#60976=CARTESIAN_POINT('Ctrl Pts',(-66.,5.70994233430443,15.195559764519));
#60977=CARTESIAN_POINT('Ctrl Pts',(-50.,5.70994233430443,15.195559764519));
#60978=CARTESIAN_POINT('Ctrl Pts',(-66.,5.71772294845736,15.0891770284618));
#60979=CARTESIAN_POINT('Ctrl Pts',(-50.,5.71772294845736,15.0891770284618));
#60980=CARTESIAN_POINT('Ctrl Pts',(-66.,5.72359388237569,14.9831894879022));
#60981=CARTESIAN_POINT('Ctrl Pts',(-50.,5.72359388237569,14.9831894879022));
#60982=CARTESIAN_POINT('Ctrl Pts',(-66.,5.72754386270271,14.8776118616624));
#60983=CARTESIAN_POINT('Ctrl Pts',(-50.,5.72754386270271,14.8776118616624));
#60984=CARTESIAN_POINT('Ctrl Pts',(-66.,5.72966360991829,14.772423041662));
#60985=CARTESIAN_POINT('Ctrl Pts',(-50.,5.72966360991829,14.772423041662));
#60986=CARTESIAN_POINT('Ctrl Pts',(-66.,5.73009695097776,14.6675837685266));
#60987=CARTESIAN_POINT('Ctrl Pts',(-50.,5.73009695097776,14.6675837685266));
#60988=CARTESIAN_POINT('Ctrl Pts',(-66.,5.72896217357436,14.5630648469857));
#60989=CARTESIAN_POINT('Ctrl Pts',(-50.,5.72896217357436,14.5630648469857));
#60990=CARTESIAN_POINT('Ctrl Pts',(-66.,5.72627848390049,14.4588735885414));
#60991=CARTESIAN_POINT('Ctrl Pts',(-50.,5.72627848390049,14.4588735885414));
#60992=CARTESIAN_POINT('Ctrl Pts',(-66.,5.72190090792526,14.3550772805332));
#60993=CARTESIAN_POINT('Ctrl Pts',(-50.,5.72190090792526,14.3550772805332));
#60994=CARTESIAN_POINT('Ctrl Pts',(-66.,5.71542331821735,14.2518379845708));
#60995=CARTESIAN_POINT('Ctrl Pts',(-50.,5.71542331821735,14.2518379845708));
#60996=CARTESIAN_POINT('Ctrl Pts',(-66.,5.70626231068308,14.1493832151514));
#60997=CARTESIAN_POINT('Ctrl Pts',(-50.,5.70626231068308,14.1493832151514));
#60998=CARTESIAN_POINT('Ctrl Pts',(-66.,5.6938022661864,14.0479549027521));
#60999=CARTESIAN_POINT('Ctrl Pts',(-50.,5.6938022661864,14.0479549027521));
#61000=CARTESIAN_POINT('Ctrl Pts',(-66.,5.67752537508807,13.9477637996424));
#61001=CARTESIAN_POINT('Ctrl Pts',(-50.,5.67752537508807,13.9477637996424));
#61002=CARTESIAN_POINT('Ctrl Pts',(-66.,5.65713696965892,13.8489453830157));
#61003=CARTESIAN_POINT('Ctrl Pts',(-50.,5.65713696965892,13.8489453830157));
#61004=CARTESIAN_POINT('Ctrl Pts',(-66.,5.63272454065023,13.7515043267519));
#61005=CARTESIAN_POINT('Ctrl Pts',(-50.,5.63272454065023,13.7515043267519));
#61006=CARTESIAN_POINT('Ctrl Pts',(-66.,5.60468396737303,13.6553383842666));
#61007=CARTESIAN_POINT('Ctrl Pts',(-50.,5.60468396737303,13.6553383842666));
#61008=CARTESIAN_POINT('Ctrl Pts',(-66.,5.57358602861192,13.5602826717323));
#61009=CARTESIAN_POINT('Ctrl Pts',(-50.,5.57358602861192,13.5602826717323));
#61010=CARTESIAN_POINT('Ctrl Pts',(-66.,5.54006285706051,13.466147083991));
#61011=CARTESIAN_POINT('Ctrl Pts',(-50.,5.54006285706051,13.466147083991));
#61012=CARTESIAN_POINT('Ctrl Pts',(-66.,5.50469122725311,13.3727548702637));
#61013=CARTESIAN_POINT('Ctrl Pts',(-50.,5.50469122725311,13.3727548702637));
#61014=CARTESIAN_POINT('Ctrl Pts',(-66.,5.46786602291259,13.2799842691689));
#61015=CARTESIAN_POINT('Ctrl Pts',(-50.,5.46786602291259,13.2799842691689));
#61016=CARTESIAN_POINT('Ctrl Pts',(-66.,5.42982469604617,13.1877615232676));
#61017=CARTESIAN_POINT('Ctrl Pts',(-50.,5.42982469604617,13.1877615232676));
#61018=CARTESIAN_POINT('Ctrl Pts',(-66.,5.39851683671257,13.1143907147436));
#61019=CARTESIAN_POINT('Ctrl Pts',(-50.,5.39851683671257,13.1143907147436));
#61020=CARTESIAN_POINT('Ctrl Pts',(-66.,5.37456335134248,13.0595854308535));
#61021=CARTESIAN_POINT('Ctrl Pts',(-50.,5.37456335134248,13.0595854308535));
#61022=CARTESIAN_POINT('Ctrl Pts',(-66.,5.35838461816811,13.0231474696198));
#61023=CARTESIAN_POINT('Ctrl Pts',(-50.,5.35838461816811,13.0231474696198));
#61024=CARTESIAN_POINT('Ctrl Pts',(-66.,5.35024281477071,13.004953213026));
#61025=CARTESIAN_POINT('Ctrl Pts',(-50.,5.35024281477071,13.004953213026));
#61026=CARTESIAN_POINT('Origin',(-65.75,0.,0.));
#61027=CARTESIAN_POINT('',(-65.5,9.39615722699085,14.0170558380021));
#61028=CARTESIAN_POINT('Origin',(-65.5,0.,0.));
#61029=CARTESIAN_POINT('Ctrl Pts',(-65.5,9.39615722699085,14.0170558380021));
#61030=CARTESIAN_POINT('Ctrl Pts',(-65.693159547678,9.37933997904567,13.7957861293633));
#61031=CARTESIAN_POINT('Ctrl Pts',(-65.861125696713,9.3565516065934,13.6076347927665));
#61032=CARTESIAN_POINT('Ctrl Pts',(-66.,9.33394806226437,13.4542944285812));
#61033=CARTESIAN_POINT('Origin',(-58.,0.,0.));
#61034=CARTESIAN_POINT('',(-50.5,9.39615722699085,14.0170558380021));
#61035=CARTESIAN_POINT('Origin',(-50.5,0.,0.));
#61036=CARTESIAN_POINT('Ctrl Pts',(-50.5,9.39615722699085,14.0170558380021));
#61037=CARTESIAN_POINT('Ctrl Pts',(-55.5,9.39615722699085,14.0170558380021));
#61038=CARTESIAN_POINT('Ctrl Pts',(-60.5,9.39615722699085,14.0170558380021));
#61039=CARTESIAN_POINT('Ctrl Pts',(-65.5,9.39615722699085,14.0170558380021));
#61040=CARTESIAN_POINT('Origin',(-50.25,0.,0.));
#61041=CARTESIAN_POINT('Ctrl Pts',(-50.,9.33394806226437,13.4542944285812));
#61042=CARTESIAN_POINT('Ctrl Pts',(-50.1388743032948,9.35655160659466,13.6076347927751));
#61043=CARTESIAN_POINT('Ctrl Pts',(-50.3068404523291,9.3793399790463,13.7957861293714));
#61044=CARTESIAN_POINT('Ctrl Pts',(-50.5,9.39615722699085,14.0170558380021));
#61045=CARTESIAN_POINT('Ctrl Pts',(-66.,9.48921088782658,10.3782842019456));
#61046=CARTESIAN_POINT('Ctrl Pts',(-50.,9.48921088782658,10.3782842019456));
#61047=CARTESIAN_POINT('Ctrl Pts',(-66.,9.5042599930153,10.3961665635534));
#61048=CARTESIAN_POINT('Ctrl Pts',(-50.,9.5042599930153,10.3961665635534));
#61049=CARTESIAN_POINT('Ctrl Pts',(-66.,9.53453615016101,10.4317934371322));
#61050=CARTESIAN_POINT('Ctrl Pts',(-50.,9.53453615016101,10.4317934371322));
#61051=CARTESIAN_POINT('Ctrl Pts',(-66.,9.58048422171402,10.4848202111794));
#61052=CARTESIAN_POINT('Ctrl Pts',(-50.,9.58048422171402,10.4848202111794));
#61053=CARTESIAN_POINT('Ctrl Pts',(-66.,9.64281744709338,10.5546942954216));
#61054=CARTESIAN_POINT('Ctrl Pts',(-50.,9.64281744709338,10.5546942954216));
#61055=CARTESIAN_POINT('Ctrl Pts',(-66.,9.72254683584991,10.6406085262144));
#61056=CARTESIAN_POINT('Ctrl Pts',(-50.,9.72254683584991,10.6406085262144));
#61057=CARTESIAN_POINT('Ctrl Pts',(-66.,9.80416846317344,10.7249595816546));
#61058=CARTESIAN_POINT('Ctrl Pts',(-50.,9.80416846317344,10.7249595816546));
#61059=CARTESIAN_POINT('Ctrl Pts',(-66.,9.88782918758628,10.8074894324552));
#61060=CARTESIAN_POINT('Ctrl Pts',(-50.,9.88782918758628,10.8074894324552));
#61061=CARTESIAN_POINT('Ctrl Pts',(-66.,9.97376743729857,10.8877656023939));
#61062=CARTESIAN_POINT('Ctrl Pts',(-50.,9.97376743729857,10.8877656023939));
#61063=CARTESIAN_POINT('Ctrl Pts',(-66.,10.0623044106004,10.9652479123292));
#61064=CARTESIAN_POINT('Ctrl Pts',(-50.,10.0623044106004,10.9652479123292));
#61065=CARTESIAN_POINT('Ctrl Pts',(-66.,10.1538362031934,11.0393768173572));
#61066=CARTESIAN_POINT('Ctrl Pts',(-50.,10.1538362031934,11.0393768173572));
#61067=CARTESIAN_POINT('Ctrl Pts',(-66.,10.2488131895374,11.1096536475468));
#61068=CARTESIAN_POINT('Ctrl Pts',(-50.,10.2488131895374,11.1096536475468));
#61069=CARTESIAN_POINT('Ctrl Pts',(-66.,10.347755963003,11.1757261609666));
#61070=CARTESIAN_POINT('Ctrl Pts',(-50.,10.347755963003,11.1757261609666));
#61071=CARTESIAN_POINT('Ctrl Pts',(-66.,10.4510776067987,11.237474600108));
#61072=CARTESIAN_POINT('Ctrl Pts',(-50.,10.4510776067987,11.237474600108));
#61073=CARTESIAN_POINT('Ctrl Pts',(-66.,10.558769691859,11.2951234927996));
#61074=CARTESIAN_POINT('Ctrl Pts',(-50.,10.558769691859,11.2951234927996));
#61075=CARTESIAN_POINT('Ctrl Pts',(-66.,10.6701988175887,11.3493082317362));
#61076=CARTESIAN_POINT('Ctrl Pts',(-50.,10.6701988175887,11.3493082317362));
#61077=CARTESIAN_POINT('Ctrl Pts',(-66.,10.7836901223469,11.4012548314131));
#61078=CARTESIAN_POINT('Ctrl Pts',(-50.,10.7836901223469,11.4012548314131));
#61079=CARTESIAN_POINT('Ctrl Pts',(-66.,10.896814048301,11.4525672852113));
#61080=CARTESIAN_POINT('Ctrl Pts',(-50.,10.896814048301,11.4525672852113));
#61081=CARTESIAN_POINT('Ctrl Pts',(-66.,11.0075923712357,11.5044910494005));
#61082=CARTESIAN_POINT('Ctrl Pts',(-50.,11.0075923712357,11.5044910494005));
#61083=CARTESIAN_POINT('Ctrl Pts',(-66.,11.1153726577894,11.5573722819667));
#61084=CARTESIAN_POINT('Ctrl Pts',(-50.,11.1153726577894,11.5573722819667));
#61085=CARTESIAN_POINT('Ctrl Pts',(-66.,11.2220605212152,11.6098943525204));
#61086=CARTESIAN_POINT('Ctrl Pts',(-50.,11.2220605212152,11.6098943525204));
#61087=CARTESIAN_POINT('Ctrl Pts',(-66.,11.3325619722949,11.6588176962357));
#61088=CARTESIAN_POINT('Ctrl Pts',(-50.,11.3325619722949,11.6588176962357));
#61089=CARTESIAN_POINT('Ctrl Pts',(-66.,11.4520601045496,11.7007489213372));
#61090=CARTESIAN_POINT('Ctrl Pts',(-50.,11.4520601045496,11.7007489213372));
#61091=CARTESIAN_POINT('Ctrl Pts',(-66.,11.5836877573447,11.7336565821219));
#61092=CARTESIAN_POINT('Ctrl Pts',(-50.,11.5836877573447,11.7336565821219));
#61093=CARTESIAN_POINT('Ctrl Pts',(-66.,11.7261518526103,11.7584167691267));
#61094=CARTESIAN_POINT('Ctrl Pts',(-50.,11.7261518526103,11.7584167691267));
#61095=CARTESIAN_POINT('Ctrl Pts',(-66.,11.8710524298673,11.7805590057687));
#61096=CARTESIAN_POINT('Ctrl Pts',(-50.,11.8710524298673,11.7805590057687));
#61097=CARTESIAN_POINT('Ctrl Pts',(-66.,12.0049368454181,11.8089201490911));
#61098=CARTESIAN_POINT('Ctrl Pts',(-50.,12.0049368454181,11.8089201490911));
#61099=CARTESIAN_POINT('Ctrl Pts',(-66.,12.1119147081034,11.8539322819168));
#61100=CARTESIAN_POINT('Ctrl Pts',(-50.,12.1119147081034,11.8539322819168));
#61101=CARTESIAN_POINT('Ctrl Pts',(-66.,12.1758810539398,11.9261667725489));
#61102=CARTESIAN_POINT('Ctrl Pts',(-50.,12.1758810539398,11.9261667725489));
#61103=CARTESIAN_POINT('Ctrl Pts',(-66.,12.183322517921,12.0344969363598));
#61104=CARTESIAN_POINT('Ctrl Pts',(-50.,12.183322517921,12.0344969363598));
#61105=CARTESIAN_POINT('Ctrl Pts',(-66.,12.1240717269814,12.1856037794161));
#61106=CARTESIAN_POINT('Ctrl Pts',(-50.,12.1240717269814,12.1856037794161));
#61107=CARTESIAN_POINT('Ctrl Pts',(-66.,11.9905553905945,12.384467849066));
#61108=CARTESIAN_POINT('Ctrl Pts',(-50.,11.9905553905945,12.384467849066));
#61109=CARTESIAN_POINT('Ctrl Pts',(-66.,11.7774987869249,12.6345623838968));
#61110=CARTESIAN_POINT('Ctrl Pts',(-50.,11.7774987869249,12.6345623838968));
#61111=CARTESIAN_POINT('Ctrl Pts',(-66.,11.4814643452976,12.9381551285812));
#61112=CARTESIAN_POINT('Ctrl Pts',(-50.,11.4814643452976,12.9381551285812));
#61113=CARTESIAN_POINT('Ctrl Pts',(-66.,11.1004818366232,13.2965502388611));
#61114=CARTESIAN_POINT('Ctrl Pts',(-50.,11.1004818366232,13.2965502388611));
#61115=CARTESIAN_POINT('Ctrl Pts',(-66.,10.6336578580906,13.7103437971785));
#61116=CARTESIAN_POINT('Ctrl Pts',(-50.,10.6336578580906,13.7103437971785));
#61117=CARTESIAN_POINT('Ctrl Pts',(-66.,10.1913804628862,14.0857987564915));
#61118=CARTESIAN_POINT('Ctrl Pts',(-50.,10.1913804628862,14.0857987564915));
#61119=CARTESIAN_POINT('Ctrl Pts',(-66.,9.82103857054357,14.392328422685));
#61120=CARTESIAN_POINT('Ctrl Pts',(-50.,9.82103857054357,14.392328422685));
#61121=CARTESIAN_POINT('Ctrl Pts',(-66.,9.55699621520391,14.6077505454562));
#61122=CARTESIAN_POINT('Ctrl Pts',(-50.,9.55699621520391,14.6077505454562));
#61123=CARTESIAN_POINT('Ctrl Pts',(-66.,9.42068809552632,14.7182288610691));
#61124=CARTESIAN_POINT('Ctrl Pts',(-50.,9.42068809552632,14.7182288610691));
#61125=CARTESIAN_POINT('',(-65.5,12.0370405584342,11.8268879928158));
#61126=CARTESIAN_POINT('Ctrl Pts',(-66.,11.4573006693292,11.699183149801));
#61127=CARTESIAN_POINT('Ctrl Pts',(-65.7933280154038,11.6841669321105,11.7662800362502));
#61128=CARTESIAN_POINT('Ctrl Pts',(-65.6370761749488,11.8992955888885,11.7714956810329));
#61129=CARTESIAN_POINT('Ctrl Pts',(-65.5,12.0370405584342,11.8268879928158));
#61130=CARTESIAN_POINT('',(-66.,9.48921088782658,10.3782842019456));
#61131=CARTESIAN_POINT('',(-50.5,12.0370405584342,11.8268879928158));
#61132=CARTESIAN_POINT('Ctrl Pts',(-50.5,12.0370405584342,11.8268879928158));
#61133=CARTESIAN_POINT('Ctrl Pts',(-50.451861834912,11.98866752726,11.8074354201845));
#61134=CARTESIAN_POINT('Ctrl Pts',(-50.4012423593881,11.9308719343602,11.7939736533257));
#61135=CARTESIAN_POINT('Ctrl Pts',(-50.2441129793797,11.7444907150908,11.7586971973344));
#61136=CARTESIAN_POINT('Ctrl Pts',(-50.1366827452942,11.607338922807,11.7435577497667));
#61137=CARTESIAN_POINT('Ctrl Pts',(-50.,11.4573006693292,11.699183149801));
#61138=CARTESIAN_POINT('Ctrl Pts',(-65.5,12.0370405584342,11.8268879928158));
#61139=CARTESIAN_POINT('Ctrl Pts',(-60.5,12.0370405584342,11.8268879928158));
#61140=CARTESIAN_POINT('Ctrl Pts',(-55.5,12.0370405584342,11.8268879928158));
#61141=CARTESIAN_POINT('Ctrl Pts',(-50.5,12.0370405584342,11.8268879928158));
#61142=CARTESIAN_POINT('Origin',(-66.,0.,0.));
#61143=CARTESIAN_POINT('',(-66.,8.41635544546802,11.2658274114927));
#61144=CARTESIAN_POINT('Ctrl Pts',(-66.,9.42068809552632,14.7182288610691));
#61145=CARTESIAN_POINT('Ctrl Pts',(-50.,9.42068809552632,14.7182288610691));
#61146=CARTESIAN_POINT('Ctrl Pts',(-66.,9.42079687884903,14.695719775262));
#61147=CARTESIAN_POINT('Ctrl Pts',(-50.,9.42079687884903,14.695719775262));
#61148=CARTESIAN_POINT('Ctrl Pts',(-66.,9.42087500044404,14.6507507775818));
#61149=CARTESIAN_POINT('Ctrl Pts',(-50.,9.42087500044404,14.6507507775818));
#61150=CARTESIAN_POINT('Ctrl Pts',(-66.,9.42057384830158,14.5834448025836));
#61151=CARTESIAN_POINT('Ctrl Pts',(-50.,9.42057384830158,14.5834448025836));
#61152=CARTESIAN_POINT('Ctrl Pts',(-66.,9.41933452504685,14.4939989404162));
#61153=CARTESIAN_POINT('Ctrl Pts',(-50.,9.41933452504685,14.4939989404162));
#61154=CARTESIAN_POINT('Ctrl Pts',(-66.,9.41638344569407,14.3826863180029));
#61155=CARTESIAN_POINT('Ctrl Pts',(-50.,9.41638344569407,14.3826863180029));
#61156=CARTESIAN_POINT('Ctrl Pts',(-66.,9.41202475171563,14.2718714066195));
#61157=CARTESIAN_POINT('Ctrl Pts',(-50.,9.41202475171563,14.2718714066195));
#61158=CARTESIAN_POINT('Ctrl Pts',(-66.,9.40625578576533,14.1615571285314));
#61159=CARTESIAN_POINT('Ctrl Pts',(-50.,9.40625578576533,14.1615571285314));
#61160=CARTESIAN_POINT('Ctrl Pts',(-66.,9.39907960579085,14.0517457606552));
#61161=CARTESIAN_POINT('Ctrl Pts',(-50.,9.39907960579085,14.0517457606552));
#61162=CARTESIAN_POINT('Ctrl Pts',(-66.,9.39050922516292,13.9424376640721));
#61163=CARTESIAN_POINT('Ctrl Pts',(-50.,9.39050922516292,13.9424376640721));
#61164=CARTESIAN_POINT('Ctrl Pts',(-66.,9.38055922634845,13.8336358786192));
#61165=CARTESIAN_POINT('Ctrl Pts',(-50.,9.38055922634845,13.8336358786192));
#61166=CARTESIAN_POINT('Ctrl Pts',(-66.,9.36923599014777,13.7253513155756));
#61167=CARTESIAN_POINT('Ctrl Pts',(-50.,9.36923599014777,13.7253513155756));
#61168=CARTESIAN_POINT('Ctrl Pts',(-66.,9.35652779136491,13.6176081888639));
#61169=CARTESIAN_POINT('Ctrl Pts',(-50.,9.35652779136491,13.6176081888639));
#61170=CARTESIAN_POINT('Ctrl Pts',(-66.,9.34239671925027,13.5104482836997));
#61171=CARTESIAN_POINT('Ctrl Pts',(-50.,9.34239671925027,13.5104482836997));
#61172=CARTESIAN_POINT('Ctrl Pts',(-66.,9.32676549500383,13.4039384968844));
#61173=CARTESIAN_POINT('Ctrl Pts',(-50.,9.32676549500383,13.4039384968844));
#61174=CARTESIAN_POINT('Ctrl Pts',(-66.,9.30953603926783,13.2981583970009));
#61175=CARTESIAN_POINT('Ctrl Pts',(-50.,9.30953603926783,13.2981583970009));
#61176=CARTESIAN_POINT('Ctrl Pts',(-66.,9.29061590049322,13.1931829101653));
#61177=CARTESIAN_POINT('Ctrl Pts',(-50.,9.29061590049322,13.1931829101653));
#61178=CARTESIAN_POINT('Ctrl Pts',(-66.,9.26994435872398,13.0890651211961));
#61179=CARTESIAN_POINT('Ctrl Pts',(-50.,9.26994435872398,13.0890651211961));
#61180=CARTESIAN_POINT('Ctrl Pts',(-66.,9.24751415519882,12.9858220900665));
#61181=CARTESIAN_POINT('Ctrl Pts',(-50.,9.24751415519882,12.9858220900665));
#61182=CARTESIAN_POINT('Ctrl Pts',(-66.,9.22340791088078,12.8834108105793));
#61183=CARTESIAN_POINT('Ctrl Pts',(-50.,9.22340791088078,12.8834108105793));
#61184=CARTESIAN_POINT('Ctrl Pts',(-66.,9.19775517072751,12.7817574884561));
#61185=CARTESIAN_POINT('Ctrl Pts',(-50.,9.19775517072751,12.7817574884561));
#61186=CARTESIAN_POINT('Ctrl Pts',(-66.,9.17066324563836,12.6808044286968));
#61187=CARTESIAN_POINT('Ctrl Pts',(-50.,9.17066324563836,12.6808044286968));
#61188=CARTESIAN_POINT('Ctrl Pts',(-66.,9.14215255670447,12.580553936713));
#61189=CARTESIAN_POINT('Ctrl Pts',(-50.,9.14215255670447,12.580553936713));
#61190=CARTESIAN_POINT('Ctrl Pts',(-66.,9.11209941820162,12.4811072394643));
#61191=CARTESIAN_POINT('Ctrl Pts',(-50.,9.11209941820162,12.4811072394643));
#61192=CARTESIAN_POINT('Ctrl Pts',(-66.,9.08015076502197,12.3827223068819));
#61193=CARTESIAN_POINT('Ctrl Pts',(-50.,9.08015076502197,12.3827223068819));
#61194=CARTESIAN_POINT('Ctrl Pts',(-66.,9.04579810233888,12.2857645923749));
#61195=CARTESIAN_POINT('Ctrl Pts',(-50.,9.04579810233888,12.2857645923749));
#61196=CARTESIAN_POINT('Ctrl Pts',(-66.,9.00850531748659,12.1906215239832));
#61197=CARTESIAN_POINT('Ctrl Pts',(-50.,9.00850531748659,12.1906215239832));
#61198=CARTESIAN_POINT('Ctrl Pts',(-66.,8.96782328072592,12.0976260068268));
#61199=CARTESIAN_POINT('Ctrl Pts',(-50.,8.96782328072592,12.0976260068268));
#61200=CARTESIAN_POINT('Ctrl Pts',(-66.,8.9235002736643,12.0069825427185));
#61201=CARTESIAN_POINT('Ctrl Pts',(-50.,8.9235002736643,12.0069825427185));
#61202=CARTESIAN_POINT('Ctrl Pts',(-66.,8.87562220071675,11.9186739006343));
#61203=CARTESIAN_POINT('Ctrl Pts',(-50.,8.87562220071675,11.9186739006343));
#61204=CARTESIAN_POINT('Ctrl Pts',(-66.,8.82454707622628,11.8325025950734));
#61205=CARTESIAN_POINT('Ctrl Pts',(-50.,8.82454707622628,11.8325025950734));
#61206=CARTESIAN_POINT('Ctrl Pts',(-66.,8.77078674197194,11.7481669754252));
#61207=CARTESIAN_POINT('Ctrl Pts',(-50.,8.77078674197194,11.7481669754252));
#61208=CARTESIAN_POINT('Ctrl Pts',(-66.,8.71490619380604,11.6653257040265));
#61209=CARTESIAN_POINT('Ctrl Pts',(-50.,8.71490619380604,11.6653257040265));
#61210=CARTESIAN_POINT('Ctrl Pts',(-66.,8.657420129699,11.5836641450553));
#61211=CARTESIAN_POINT('Ctrl Pts',(-50.,8.657420129699,11.5836641450553));
#61212=CARTESIAN_POINT('Ctrl Pts',(-66.,8.59868074655117,11.5029661588994));
#61213=CARTESIAN_POINT('Ctrl Pts',(-50.,8.59868074655117,11.5029661588994));
#61214=CARTESIAN_POINT('Ctrl Pts',(-66.,8.53889969364915,11.4231012534324));
#61215=CARTESIAN_POINT('Ctrl Pts',(-50.,8.53889969364915,11.4231012534324));
#61216=CARTESIAN_POINT('Ctrl Pts',(-66.,8.49032885019461,11.3598214717827));
#61217=CARTESIAN_POINT('Ctrl Pts',(-50.,8.49032885019461,11.3598214717827));
#61218=CARTESIAN_POINT('Ctrl Pts',(-66.,8.45349838774813,11.3126949862398));
#61219=CARTESIAN_POINT('Ctrl Pts',(-50.,8.45349838774813,11.3126949862398));
#61220=CARTESIAN_POINT('Ctrl Pts',(-66.,8.4287661867593,11.2814252778905));
#61221=CARTESIAN_POINT('Ctrl Pts',(-50.,8.4287661867593,11.2814252778905));
#61222=CARTESIAN_POINT('Ctrl Pts',(-66.,8.416355445468,11.2658274114927));
#61223=CARTESIAN_POINT('Ctrl Pts',(-50.,8.416355445468,11.2658274114927));
#61224=CARTESIAN_POINT('Origin',(-65.75,0.,0.));
#61225=CARTESIAN_POINT('',(-65.5,12.5868597041166,11.239954972725));
#61226=CARTESIAN_POINT('Origin',(-65.5,0.,0.));
#61227=CARTESIAN_POINT('Ctrl Pts',(-65.5,12.5868597041166,11.239954972725));
#61228=CARTESIAN_POINT('Ctrl Pts',(-65.6931595476683,12.5155432620696,11.0298191383741));
#61229=CARTESIAN_POINT('Ctrl Pts',(-65.8611256967109,12.446679493572,10.853246159768));
#61230=CARTESIAN_POINT('Ctrl Pts',(-66.,12.3866518832851,10.7103445379834));
#61231=CARTESIAN_POINT('Origin',(-58.,0.,0.));
#61232=CARTESIAN_POINT('',(-50.5,12.5868597041166,11.239954972725));
#61233=CARTESIAN_POINT('Origin',(-50.5,0.,0.));
#61234=CARTESIAN_POINT('Ctrl Pts',(-50.5,12.5868597041166,11.239954972725));
#61235=CARTESIAN_POINT('Ctrl Pts',(-55.5,12.5868597041166,11.239954972725));
#61236=CARTESIAN_POINT('Ctrl Pts',(-60.5,12.5868597041166,11.239954972725));
#61237=CARTESIAN_POINT('Ctrl Pts',(-65.5,12.5868597041166,11.239954972725));
#61238=CARTESIAN_POINT('Origin',(-50.25,0.,0.));
#61239=CARTESIAN_POINT('Ctrl Pts',(-50.,12.3866518832851,10.7103445379834));
#61240=CARTESIAN_POINT('Ctrl Pts',(-50.138874303285,12.4466794935702,10.8532461597638));
#61241=CARTESIAN_POINT('Ctrl Pts',(-50.3068404523221,12.515543262066,11.0298191383637));
#61242=CARTESIAN_POINT('Ctrl Pts',(-50.5,12.5868597041166,11.239954972725));
#61243=CARTESIAN_POINT('Ctrl Pts',(-66.,11.7720642054939,7.69236053443469));
#61244=CARTESIAN_POINT('Ctrl Pts',(-50.,11.7720642054939,7.69236053443469));
#61245=CARTESIAN_POINT('Ctrl Pts',(-66.,11.7910876778603,7.70593852849788));
#61246=CARTESIAN_POINT('Ctrl Pts',(-50.,11.7910876778603,7.70593852849788));
#61247=CARTESIAN_POINT('Ctrl Pts',(-66.,11.8292726970256,7.73291674422561));
#61248=CARTESIAN_POINT('Ctrl Pts',(-50.,11.8292726970256,7.73291674422561));
#61249=CARTESIAN_POINT('Ctrl Pts',(-66.,11.8869644478727,7.77285076392682));
#61250=CARTESIAN_POINT('Ctrl Pts',(-50.,11.8869644478727,7.77285076392682));
#61251=CARTESIAN_POINT('Ctrl Pts',(-66.,11.96471633848,7.82502798253687));
#61252=CARTESIAN_POINT('Ctrl Pts',(-50.,11.96471633848,7.82502798253687));
#61253=CARTESIAN_POINT('Ctrl Pts',(-66.,12.0633068822383,7.88841516709048));
#61254=CARTESIAN_POINT('Ctrl Pts',(-50.,12.0633068822383,7.88841516709048));
#61255=CARTESIAN_POINT('Ctrl Pts',(-66.,12.1633414705075,7.94981770572398));
#61256=CARTESIAN_POINT('Ctrl Pts',(-50.,12.1633414705075,7.94981770572398));
#61257=CARTESIAN_POINT('Ctrl Pts',(-66.,12.2648981787049,8.00894915338555));
#61258=CARTESIAN_POINT('Ctrl Pts',(-50.,12.2648981787049,8.00894915338555));
#61259=CARTESIAN_POINT('Ctrl Pts',(-66.,12.3681003919172,8.06533132620399));
#61260=CARTESIAN_POINT('Ctrl Pts',(-50.,12.3681003919172,8.06533132620399));
#61261=CARTESIAN_POINT('Ctrl Pts',(-66.,12.4731248803097,8.11836113699226));
#61262=CARTESIAN_POINT('Ctrl Pts',(-50.,12.4731248803097,8.11836113699226));
#61263=CARTESIAN_POINT('Ctrl Pts',(-66.,12.5802161423503,8.16739811498339));
#61264=CARTESIAN_POINT('Ctrl Pts',(-50.,12.5802161423503,8.16739811498339));
#61265=CARTESIAN_POINT('Ctrl Pts',(-66.,12.6896863889879,8.21184725330542));
#61266=CARTESIAN_POINT('Ctrl Pts',(-50.,12.6896863889879,8.21184725330542));
#61267=CARTESIAN_POINT('Ctrl Pts',(-66.,12.8019522591891,8.25123791004828));
#61268=CARTESIAN_POINT('Ctrl Pts',(-50.,12.8019522591891,8.25123791004828));
#61269=CARTESIAN_POINT('Ctrl Pts',(-66.,12.9173840759125,8.28535136048938));
#61270=CARTESIAN_POINT('Ctrl Pts',(-50.,12.9173840759125,8.28535136048938));
#61271=CARTESIAN_POINT('Ctrl Pts',(-66.,13.0360295127074,8.31440717472604));
#61272=CARTESIAN_POINT('Ctrl Pts',(-50.,13.0360295127074,8.31440717472604));
#61273=CARTESIAN_POINT('Ctrl Pts',(-66.,13.1574330841607,8.33917830374554));
#61274=CARTESIAN_POINT('Ctrl Pts',(-50.,13.1574330841607,8.33917830374554));
#61275=CARTESIAN_POINT('Ctrl Pts',(-66.,13.2802774448963,8.36126876569594));
#61276=CARTESIAN_POINT('Ctrl Pts',(-50.,13.2802774448963,8.36126876569594));
#61277=CARTESIAN_POINT('Ctrl Pts',(-66.,13.4026082630414,8.38283636801991));
#61278=CARTESIAN_POINT('Ctrl Pts',(-50.,13.4026082630414,8.38283636801991));
#61279=CARTESIAN_POINT('Ctrl Pts',(-66.,13.5228191963114,8.40557940304509));
#61280=CARTESIAN_POINT('Ctrl Pts',(-50.,13.5228191963114,8.40557940304509));
#61281=CARTESIAN_POINT('Ctrl Pts',(-66.,13.640364394729,8.42999540714673));
#61282=CARTESIAN_POINT('Ctrl Pts',(-50.,13.640364394729,8.42999540714673));
#61283=CARTESIAN_POINT('Ctrl Pts',(-66.,13.7567621705396,8.45433520755552));
#61284=CARTESIAN_POINT('Ctrl Pts',(-50.,13.7567621705396,8.45433520755552));
#61285=CARTESIAN_POINT('Ctrl Pts',(-66.,13.875958756164,8.47424094106369));
#61286=CARTESIAN_POINT('Ctrl Pts',(-50.,13.875958756164,8.47424094106369));
#61287=CARTESIAN_POINT('Ctrl Pts',(-66.,14.0021305064914,8.48513684259561));
#61288=CARTESIAN_POINT('Ctrl Pts',(-50.,14.0021305064914,8.48513684259561));
#61289=CARTESIAN_POINT('Ctrl Pts',(-66.,14.137806636975,8.48427618258244));
#61290=CARTESIAN_POINT('Ctrl Pts',(-50.,14.137806636975,8.48427618258244));
#61291=CARTESIAN_POINT('Ctrl Pts',(-66.,14.2819525688271,8.47282910300502));
#61292=CARTESIAN_POINT('Ctrl Pts',(-50.,14.2819525688271,8.47282910300502));
#61293=CARTESIAN_POINT('Ctrl Pts',(-66.,14.4278073783281,8.45824039235802));
#61294=CARTESIAN_POINT('Ctrl Pts',(-50.,14.4278073783281,8.45824039235802));
#61295=CARTESIAN_POINT('Ctrl Pts',(-66.,14.5645386983009,8.45241481801397));
#61296=CARTESIAN_POINT('Ctrl Pts',(-50.,14.5645386983009,8.45241481801397));
#61297=CARTESIAN_POINT('Ctrl Pts',(-66.,14.6793497169449,8.4694084993151));
#61298=CARTESIAN_POINT('Ctrl Pts',(-50.,14.6793497169449,8.4694084993151));
#61299=CARTESIAN_POINT('Ctrl Pts',(-66.,14.7592704297256,8.52346582726567));
#61300=CARTESIAN_POINT('Ctrl Pts',(-50.,14.7592704297256,8.52346582726567));
#61301=CARTESIAN_POINT('Ctrl Pts',(-66.,14.7934187226467,8.62654198293735));
#61302=CARTESIAN_POINT('Ctrl Pts',(-50.,14.7934187226467,8.62654198293735));
#61303=CARTESIAN_POINT('Ctrl Pts',(-66.,14.7736081480085,8.78763659916624));
#61304=CARTESIAN_POINT('Ctrl Pts',(-50.,14.7736081480085,8.78763659916624));
#61305=CARTESIAN_POINT('Ctrl Pts',(-66.,14.693741955891,9.01345715101332));
#61306=CARTESIAN_POINT('Ctrl Pts',(-50.,14.693741955891,9.01345715101332));
#61307=CARTESIAN_POINT('Ctrl Pts',(-66.,14.5495748988569,9.30867952886707));
#61308=CARTESIAN_POINT('Ctrl Pts',(-50.,14.5495748988569,9.30867952886707));
#61309=CARTESIAN_POINT('Ctrl Pts',(-66.,14.3383413690023,9.67635512109445));
#61310=CARTESIAN_POINT('Ctrl Pts',(-50.,14.3383413690023,9.67635512109445));
#61311=CARTESIAN_POINT('Ctrl Pts',(-66.,14.0584573659516,10.1182370870364));
#61312=CARTESIAN_POINT('Ctrl Pts',(-50.,14.0584573659516,10.1182370870364));
#61313=CARTESIAN_POINT('Ctrl Pts',(-66.,13.7092057944614,10.6351249623533));
#61314=CARTESIAN_POINT('Ctrl Pts',(-50.,13.7092057944614,10.6351249623533));
#61315=CARTESIAN_POINT('Ctrl Pts',(-66.,13.3741952083856,11.108774229215));
#61316=CARTESIAN_POINT('Ctrl Pts',(-50.,13.3741952083856,11.108774229215));
#61317=CARTESIAN_POINT('Ctrl Pts',(-66.,13.0917191157004,11.4977739856956));
#61318=CARTESIAN_POINT('Ctrl Pts',(-50.,13.0917191157004,11.4977739856956));
#61319=CARTESIAN_POINT('Ctrl Pts',(-66.,12.8895454398984,11.7720928899025));
#61320=CARTESIAN_POINT('Ctrl Pts',(-50.,12.8895454398984,11.7720928899025));
#61321=CARTESIAN_POINT('Ctrl Pts',(-66.,12.7849945302975,11.9129987769773));
#61322=CARTESIAN_POINT('Ctrl Pts',(-50.,12.7849945302975,11.9129987769773));
#61323=CARTESIAN_POINT('',(-65.5,14.6001022351665,8.46183430012001));
#61324=CARTESIAN_POINT('Ctrl Pts',(-66.,14.0068170377451,8.48231698718778));
#61325=CARTESIAN_POINT('Ctrl Pts',(-65.7933280154031,14.2432421968242,8.490886556274));
#61326=CARTESIAN_POINT('Ctrl Pts',(-65.6370761749492,14.4529092693668,8.44243802060488));
#61327=CARTESIAN_POINT('Ctrl Pts',(-65.5,14.6001022351665,8.46183430012001));
#61328=CARTESIAN_POINT('',(-66.,11.7720642054939,7.69236053443469));
#61329=CARTESIAN_POINT('',(-50.5,14.6001022351665,8.46183430012001));
#61330=CARTESIAN_POINT('Ctrl Pts',(-50.5,14.6001022351664,8.46183430012001));
#61331=CARTESIAN_POINT('Ctrl Pts',(-50.4518618349121,14.5484112736258,8.45502274949325));
#61332=CARTESIAN_POINT('Ctrl Pts',(-50.4012423593883,14.4890836302746,8.4563570882716));
#61333=CARTESIAN_POINT('Ctrl Pts',(-50.2441129793798,14.2997850218794,8.46854003140394));
#61334=CARTESIAN_POINT('Ctrl Pts',(-50.1366827452942,14.1631770778471,8.48798448116852));
#61335=CARTESIAN_POINT('Ctrl Pts',(-50.,14.0068170377451,8.48231698718778));
#61336=CARTESIAN_POINT('Ctrl Pts',(-65.5,14.6001022351665,8.46183430012001));
#61337=CARTESIAN_POINT('Ctrl Pts',(-60.5,14.6001022351665,8.46183430012001));
#61338=CARTESIAN_POINT('Ctrl Pts',(-55.5,14.6001022351665,8.46183430012001));
#61339=CARTESIAN_POINT('Ctrl Pts',(-50.5,14.6001022351665,8.46183430012001));
#61340=CARTESIAN_POINT('Origin',(-66.,0.,0.));
#61341=CARTESIAN_POINT('',(-66.,10.9536375103364,8.81882824088046));
#61342=CARTESIAN_POINT('Ctrl Pts',(-66.,12.7849945302975,11.9129987769773));
#61343=CARTESIAN_POINT('Ctrl Pts',(-50.,12.7849945302975,11.9129987769773));
#61344=CARTESIAN_POINT('Ctrl Pts',(-66.,12.7795021139826,11.8911698021799));
#61345=CARTESIAN_POINT('Ctrl Pts',(-50.,12.7795021139826,11.8911698021799));
#61346=CARTESIAN_POINT('Ctrl Pts',(-66.,12.768394446285,11.8475941602033));
#61347=CARTESIAN_POINT('Ctrl Pts',(-50.,12.768394446285,11.8475941602033));
#61348=CARTESIAN_POINT('Ctrl Pts',(-66.,12.7513644400631,11.782477619669));
#61349=CARTESIAN_POINT('Ctrl Pts',(-50.,12.7513644400631,11.782477619669));
#61350=CARTESIAN_POINT('Ctrl Pts',(-66.,12.7279197710576,11.6961500709014));
#61351=CARTESIAN_POINT('Ctrl Pts',(-50.,12.7279197710576,11.6961500709014));
#61352=CARTESIAN_POINT('Ctrl Pts',(-66.,12.6973790817813,11.5890684428021));
#61353=CARTESIAN_POINT('Ctrl Pts',(-50.,12.6973790817813,11.5890684428021));
#61354=CARTESIAN_POINT('Ctrl Pts',(-66.,12.6655987763812,11.4828189487479));
#61355=CARTESIAN_POINT('Ctrl Pts',(-50.,12.6655987763812,11.4828189487479));
#61356=CARTESIAN_POINT('Ctrl Pts',(-66.,12.6325770077342,11.3774050800509));
#61357=CARTESIAN_POINT('Ctrl Pts',(-50.,12.6325770077342,11.3774050800509));
#61358=CARTESIAN_POINT('Ctrl Pts',(-66.,12.5983173039631,11.2728282816136));
#61359=CARTESIAN_POINT('Ctrl Pts',(-50.,12.5983173039631,11.2728282816136));
#61360=CARTESIAN_POINT('Ctrl Pts',(-66.,12.562832359397,11.1690856668796));
#61361=CARTESIAN_POINT('Ctrl Pts',(-50.,12.562832359397,11.1690856668796));
#61362=CARTESIAN_POINT('Ctrl Pts',(-66.,12.5261370543444,11.0661765536716));
#61363=CARTESIAN_POINT('Ctrl Pts',(-50.,12.5261370543444,11.0661765536716));
#61364=CARTESIAN_POINT('Ctrl Pts',(-66.,12.488240282666,10.9641099236305));
#61365=CARTESIAN_POINT('Ctrl Pts',(-50.,12.488240282666,10.9641099236305));
#61366=CARTESIAN_POINT('Ctrl Pts',(-66.,12.4491367092919,10.8629121458916));
#61367=CARTESIAN_POINT('Ctrl Pts',(-50.,12.4491367092919,10.8629121458916));
#61368=CARTESIAN_POINT('Ctrl Pts',(-66.,12.4088000060691,10.7626331209311));
#61369=CARTESIAN_POINT('Ctrl Pts',(-50.,12.4088000060691,10.7626331209311));
#61370=CARTESIAN_POINT('Ctrl Pts',(-66.,12.3671719586111,10.6633568623205));
#61371=CARTESIAN_POINT('Ctrl Pts',(-50.,12.3671719586111,10.6633568623205));
#61372=CARTESIAN_POINT('Ctrl Pts',(-66.,12.3241773568055,10.5651848301937));
#61373=CARTESIAN_POINT('Ctrl Pts',(-50.,12.3241773568055,10.5651848301937));
#61374=CARTESIAN_POINT('Ctrl Pts',(-66.,12.2797452870059,10.4682125884904));
#61375=CARTESIAN_POINT('Ctrl Pts',(-50.,12.2797452870059,10.4682125884904));
#61376=CARTESIAN_POINT('Ctrl Pts',(-66.,12.2338301385431,10.3725066547111));
#61377=CARTESIAN_POINT('Ctrl Pts',(-50.,12.2338301385431,10.3725066547111));
#61378=CARTESIAN_POINT('Ctrl Pts',(-66.,12.1864291233458,10.2780853580389));
#61379=CARTESIAN_POINT('Ctrl Pts',(-50.,12.1864291233458,10.2780853580389));
#61380=CARTESIAN_POINT('Ctrl Pts',(-66.,12.1376115714812,10.1848864963973));
#61381=CARTESIAN_POINT('Ctrl Pts',(-50.,12.1376115714812,10.1848864963973));
#61382=CARTESIAN_POINT('Ctrl Pts',(-66.,12.0874846061232,10.0928063773702));
#61383=CARTESIAN_POINT('Ctrl Pts',(-50.,12.0874846061232,10.0928063773702));
#61384=CARTESIAN_POINT('Ctrl Pts',(-66.,12.0361378186387,10.0017624314164));
#61385=CARTESIAN_POINT('Ctrl Pts',(-50.,12.0361378186387,10.0017624314164));
#61386=CARTESIAN_POINT('Ctrl Pts',(-66.,11.9835915618855,9.91175181299999));
#61387=CARTESIAN_POINT('Ctrl Pts',(-50.,11.9835915618855,9.91175181299999));
#61388=CARTESIAN_POINT('Ctrl Pts',(-66.,11.9297512100749,9.82290332823825));
#61389=CARTESIAN_POINT('Ctrl Pts',(-50.,11.9297512100749,9.82290332823825));
#61390=CARTESIAN_POINT('Ctrl Pts',(-66.,11.8743389448017,9.73555464618448));
#61391=CARTESIAN_POINT('Ctrl Pts',(-50.,11.8743389448017,9.73555464618448));
#61392=CARTESIAN_POINT('Ctrl Pts',(-66.,11.8169531311064,9.65018619637799));
#61393=CARTESIAN_POINT('Ctrl Pts',(-50.,11.8169531311064,9.65018619637799));
#61394=CARTESIAN_POINT('Ctrl Pts',(-66.,11.7571708487241,9.56730656089267));
#61395=CARTESIAN_POINT('Ctrl Pts',(-50.,11.7571708487241,9.56730656089267));
#61396=CARTESIAN_POINT('Ctrl Pts',(-66.,11.6946398682888,9.48734988004618));
#61397=CARTESIAN_POINT('Ctrl Pts',(-50.,11.6946398682888,9.48734988004618));
#61398=CARTESIAN_POINT('Ctrl Pts',(-66.,11.629167237137,9.41057683066949));
#61399=CARTESIAN_POINT('Ctrl Pts',(-50.,11.629167237137,9.41057683066949));
#61400=CARTESIAN_POINT('Ctrl Pts',(-66.,11.5608318756571,9.3369493595236));
#61401=CARTESIAN_POINT('Ctrl Pts',(-50.,11.5608318756571,9.3369493595236));
#61402=CARTESIAN_POINT('Ctrl Pts',(-66.,11.4899314378663,9.26618715093123));
#61403=CARTESIAN_POINT('Ctrl Pts',(-50.,11.4899314378663,9.26618715093123));
#61404=CARTESIAN_POINT('Ctrl Pts',(-66.,11.4168866676366,9.19787074131628));
#61405=CARTESIAN_POINT('Ctrl Pts',(-50.,11.4168866676366,9.19787074131628));
#61406=CARTESIAN_POINT('Ctrl Pts',(-66.,11.3421599232118,9.13152900801114));
#61407=CARTESIAN_POINT('Ctrl Pts',(-50.,11.3421599232118,9.13152900801114));
#61408=CARTESIAN_POINT('Ctrl Pts',(-66.,11.2661714856319,9.06672919987649));
#61409=CARTESIAN_POINT('Ctrl Pts',(-50.,11.2661714856319,9.06672919987649));
#61410=CARTESIAN_POINT('Ctrl Pts',(-66.,11.1892087351483,9.00317437991606));
#61411=CARTESIAN_POINT('Ctrl Pts',(-50.,11.1892087351483,9.00317437991606));
#61412=CARTESIAN_POINT('Ctrl Pts',(-66.,11.1114442196238,8.9406855206164));
#61413=CARTESIAN_POINT('Ctrl Pts',(-50.,11.1114442196238,8.9406855206164));
#61414=CARTESIAN_POINT('Ctrl Pts',(-66.,11.0486622767737,8.89147286724882));
#61415=CARTESIAN_POINT('Ctrl Pts',(-50.,11.0486622767737,8.89147286724882));
#61416=CARTESIAN_POINT('Ctrl Pts',(-66.,11.0012690306593,8.85498631045878));
#61417=CARTESIAN_POINT('Ctrl Pts',(-50.,11.0012690306593,8.85498631045878));
#61418=CARTESIAN_POINT('Ctrl Pts',(-66.,10.9695373770028,8.83084964577152));
#61419=CARTESIAN_POINT('Ctrl Pts',(-50.,10.9695373770028,8.83084964577152));
#61420=CARTESIAN_POINT('Ctrl Pts',(-66.,10.9536375103364,8.81882824088047));
#61421=CARTESIAN_POINT('Ctrl Pts',(-50.,10.9536375103364,8.81882824088047));
#61422=CARTESIAN_POINT('Origin',(-65.75,0.,0.));
#61423=CARTESIAN_POINT('',(-65.5,14.9866834948009,7.75660639884882));
#61424=CARTESIAN_POINT('Origin',(-65.5,0.,0.));
#61425=CARTESIAN_POINT('Ctrl Pts',(-65.5,14.9866834948009,7.75660639884882));
#61426=CARTESIAN_POINT('Ctrl Pts',(-65.6931595476747,14.8653489329845,7.57080804606636));
#61427=CARTESIAN_POINT('Ctrl Pts',(-65.8611256967097,14.7547367322848,7.41690815510283));
#61428=CARTESIAN_POINT('Ctrl Pts',(-66.,14.66105681156,7.29342431017219));
#61429=CARTESIAN_POINT('Origin',(-58.,0.,0.));
#61430=CARTESIAN_POINT('',(-50.5,14.9866834948009,7.75660639884882));
#61431=CARTESIAN_POINT('Origin',(-50.5,0.,0.));
#61432=CARTESIAN_POINT('Ctrl Pts',(-50.5,14.9866834948009,7.75660639884881));
#61433=CARTESIAN_POINT('Ctrl Pts',(-55.5,14.9866834948009,7.75660639884881));
#61434=CARTESIAN_POINT('Ctrl Pts',(-60.5,14.9866834948009,7.75660639884881));
#61435=CARTESIAN_POINT('Ctrl Pts',(-65.5,14.9866834948009,7.75660639884881));
#61436=CARTESIAN_POINT('Origin',(-50.25,0.,0.));
#61437=CARTESIAN_POINT('Ctrl Pts',(-50.,14.66105681156,7.29342431017219));
#61438=CARTESIAN_POINT('Ctrl Pts',(-50.1388743032983,14.7547367322901,7.41690815510991));
#61439=CARTESIAN_POINT('Ctrl Pts',(-50.3068404523272,14.8653489329857,7.57080804606814));
#61440=CARTESIAN_POINT('Ctrl Pts',(-50.5,14.9866834948009,7.75660639884881));
#61441=CARTESIAN_POINT('Ctrl Pts',(-66.,13.3152354345065,4.52309756402217));
#61442=CARTESIAN_POINT('Ctrl Pts',(-50.,13.3152354345065,4.52309756402217));
#61443=CARTESIAN_POINT('Ctrl Pts',(-66.,13.3370379593182,4.53151803523741));
#61444=CARTESIAN_POINT('Ctrl Pts',(-50.,13.3370379593182,4.53151803523741));
#61445=CARTESIAN_POINT('Ctrl Pts',(-66.,13.3807325353144,4.54815245260096));
#61446=CARTESIAN_POINT('Ctrl Pts',(-50.,13.3807325353144,4.54815245260096));
#61447=CARTESIAN_POINT('Ctrl Pts',(-66.,13.4465429805744,4.57248451663122));
#61448=CARTESIAN_POINT('Ctrl Pts',(-50.,13.4465429805744,4.57248451663122));
#61449=CARTESIAN_POINT('Ctrl Pts',(-66.,13.5348280991712,4.60368638306948));
#61450=CARTESIAN_POINT('Ctrl Pts',(-50.,13.5348280991712,4.60368638306948));
#61451=CARTESIAN_POINT('Ctrl Pts',(-66.,13.6460849914764,4.64056367145667));
#61452=CARTESIAN_POINT('Ctrl Pts',(-50.,13.6460849914764,4.64056367145667));
#61453=CARTESIAN_POINT('Ctrl Pts',(-66.,13.7582469996088,4.67515954595839));
#61454=CARTESIAN_POINT('Ctrl Pts',(-50.,13.7582469996088,4.67515954595839));
#61455=CARTESIAN_POINT('Ctrl Pts',(-66.,13.8713185101153,4.70717714415409));
#61456=CARTESIAN_POINT('Ctrl Pts',(-50.,13.8713185101153,4.70717714415409));
#61457=CARTESIAN_POINT('Ctrl Pts',(-66.,13.9853001122203,4.73612262057495));
#61458=CARTESIAN_POINT('Ctrl Pts',(-50.,13.9853001122203,4.73612262057495));
#61459=CARTESIAN_POINT('Ctrl Pts',(-66.,14.1002130408447,4.76136787417443));
#61460=CARTESIAN_POINT('Ctrl Pts',(-50.,14.1002130408447,4.76136787417443));
#61461=CARTESIAN_POINT('Ctrl Pts',(-66.,14.2161348344847,4.78223175145606));
#61462=CARTESIAN_POINT('Ctrl Pts',(-50.,14.2161348344847,4.78223175145606));
#61463=CARTESIAN_POINT('Ctrl Pts',(-66.,14.3332199232164,4.79806029507722));
#61464=CARTESIAN_POINT('Ctrl Pts',(-50.,14.3332199232164,4.79806029507722));
#61465=CARTESIAN_POINT('Ctrl Pts',(-66.,14.4517548126435,4.80829403531135));
#61466=CARTESIAN_POINT('Ctrl Pts',(-50.,14.4517548126435,4.80829403531135));
#61467=CARTESIAN_POINT('Ctrl Pts',(-66.,14.5720437967212,4.81262902350044));
#61468=CARTESIAN_POINT('Ctrl Pts',(-50.,14.5720437967212,4.81262902350044));
#61469=CARTESIAN_POINT('Ctrl Pts',(-66.,14.6941876561096,4.81126607561379));
#61470=CARTESIAN_POINT('Ctrl Pts',(-50.,14.6941876561096,4.81126607561379));
#61471=CARTESIAN_POINT('Ctrl Pts',(-66.,14.8179374404009,4.80506713357809));
#61472=CARTESIAN_POINT('Ctrl Pts',(-50.,14.8179374404009,4.80506713357809));
#61473=CARTESIAN_POINT('Ctrl Pts',(-66.,14.9424160941388,4.79591343283465));
#61474=CARTESIAN_POINT('Ctrl Pts',(-50.,14.9424160941388,4.79591343283465));
#61475=CARTESIAN_POINT('Ctrl Pts',(-66.,15.0662673092696,4.78638101191027));
#61476=CARTESIAN_POINT('Ctrl Pts',(-50.,15.0662673092696,4.78638101191027));
#61477=CARTESIAN_POINT('Ctrl Pts',(-66.,15.1883575578327,4.77851428923771));
#61478=CARTESIAN_POINT('Ctrl Pts',(-50.,15.1883575578327,4.77851428923771));
#61479=CARTESIAN_POINT('Ctrl Pts',(-66.,15.3082818709966,4.77293091754137));
#61480=CARTESIAN_POINT('Ctrl Pts',(-50.,15.3082818709966,4.77293091754137));
#61481=CARTESIAN_POINT('Ctrl Pts',(-66.,15.4270758588568,4.76755908862997));
#61482=CARTESIAN_POINT('Ctrl Pts',(-50.,15.4270758588568,4.76755908862997));
#61483=CARTESIAN_POINT('Ctrl Pts',(-66.,15.5474780191768,4.75719646148653));
#61484=CARTESIAN_POINT('Ctrl Pts',(-50.,15.5474780191768,4.75719646148653));
#61485=CARTESIAN_POINT('Ctrl Pts',(-66.,15.6723955524765,4.73637240988335));
#61486=CARTESIAN_POINT('Ctrl Pts',(-50.,15.6723955524765,4.73637240988335));
#61487=CARTESIAN_POINT('Ctrl Pts',(-66.,15.8035951303885,4.70179750750619));
#61488=CARTESIAN_POINT('Ctrl Pts',(-50.,15.8035951303885,4.70179750750619));
#61489=CARTESIAN_POINT('Ctrl Pts',(-66.,15.9403656797971,4.65486242345584));
#61490=CARTESIAN_POINT('Ctrl Pts',(-50.,15.9403656797971,4.65486242345584));
#61491=CARTESIAN_POINT('Ctrl Pts',(-66.,16.0780101274447,4.60445942786333));
#61492=CARTESIAN_POINT('Ctrl Pts',(-50.,16.0780101274447,4.60445942786333));
#61493=CARTESIAN_POINT('Ctrl Pts',(-66.,16.208997020143,4.56481317811384));
#61494=CARTESIAN_POINT('Ctrl Pts',(-50.,16.208997020143,4.56481317811384));
#61495=CARTESIAN_POINT('Ctrl Pts',(-66.,16.3244271961989,4.55272063239585));
#61496=CARTESIAN_POINT('Ctrl Pts',(-50.,16.3244271961989,4.55272063239585));
#61497=CARTESIAN_POINT('Ctrl Pts',(-66.,16.4152805636122,4.5852041769408));
#61498=CARTESIAN_POINT('Ctrl Pts',(-50.,16.4152805636122,4.5852041769408));
#61499=CARTESIAN_POINT('Ctrl Pts',(-66.,16.4739900226401,4.67654967052486));
#61500=CARTESIAN_POINT('Ctrl Pts',(-50.,16.4739900226401,4.67654967052486));
#61501=CARTESIAN_POINT('Ctrl Pts',(-66.,16.4948644355662,4.83750989272408));
#61502=CARTESIAN_POINT('Ctrl Pts',(-50.,16.4948644355662,4.83750989272408));
#61503=CARTESIAN_POINT('Ctrl Pts',(-66.,16.473666674296,5.07609779098593));
#61504=CARTESIAN_POINT('Ctrl Pts',(-50.,16.473666674296,5.07609779098593));
#61505=CARTESIAN_POINT('Ctrl Pts',(-66.,16.4074477103004,5.39789810411011));
#61506=CARTESIAN_POINT('Ctrl Pts',(-50.,16.4074477103004,5.39789810411011));
#61507=CARTESIAN_POINT('Ctrl Pts',(-66.,16.2942876717617,5.80655413420453));
#61508=CARTESIAN_POINT('Ctrl Pts',(-50.,16.2942876717617,5.80655413420453));
#61509=CARTESIAN_POINT('Ctrl Pts',(-66.,16.1330883155878,6.30415788676021));
#61510=CARTESIAN_POINT('Ctrl Pts',(-50.,16.1330883155878,6.30415788676021));
#61511=CARTESIAN_POINT('Ctrl Pts',(-66.,15.9233539118341,6.89166211288976));
#61512=CARTESIAN_POINT('Ctrl Pts',(-50.,15.9233539118341,6.89166211288976));
#61513=CARTESIAN_POINT('Ctrl Pts',(-66.,15.7166600820928,7.43374456190315));
#61514=CARTESIAN_POINT('Ctrl Pts',(-50.,15.7166600820928,7.43374456190315));
#61515=CARTESIAN_POINT('Ctrl Pts',(-66.,15.5397988008428,7.88077212333004));
#61516=CARTESIAN_POINT('Ctrl Pts',(-50.,15.5397988008428,7.88077212333004));
#61517=CARTESIAN_POINT('Ctrl Pts',(-66.,15.412197120172,8.19675134334703));
#61518=CARTESIAN_POINT('Ctrl Pts',(-50.,15.412197120172,8.19675134334703));
#61519=CARTESIAN_POINT('Ctrl Pts',(-66.,15.3459727388094,8.35923116678319));
#61520=CARTESIAN_POINT('Ctrl Pts',(-50.,15.3459727388094,8.35923116678319));
#61521=CARTESIAN_POINT('',(-65.5,16.2457857930433,4.56509243789802));
#61522=CARTESIAN_POINT('Ctrl Pts',(-66.,15.6762335782098,4.73247565248983));
#61523=CARTESIAN_POINT('Ctrl Pts',(-65.7933280154031,15.90736217133,4.68197944667057));
#61524=CARTESIAN_POINT('Ctrl Pts',(-65.6370761749492,16.0983935063691,4.58291093022731));
#61525=CARTESIAN_POINT('Ctrl Pts',(-65.5,16.2457857930433,4.56509243789802));
#61526=CARTESIAN_POINT('',(-66.,13.3152354345065,4.52309756402217));
#61527=CARTESIAN_POINT('',(-50.5,16.2457857930433,4.56509243789802));
#61528=CARTESIAN_POINT('Ctrl Pts',(-50.5,16.2457857930433,4.56509243789802));
#61529=CARTESIAN_POINT('Ctrl Pts',(-50.4518618349122,16.1940248343557,4.57134990405274));
#61530=CARTESIAN_POINT('Ctrl Pts',(-50.4012423593884,16.1368929145766,4.58739650705545));
#61531=CARTESIAN_POINT('Ctrl Pts',(-50.2441129793799,15.9565712448129,4.64627335018861));
#61532=CARTESIAN_POINT('Ctrl Pts',(-50.1366827452942,15.8290907285646,4.69907993099531));
#61533=CARTESIAN_POINT('Ctrl Pts',(-50.,15.6762335782097,4.73247565248984));
#61534=CARTESIAN_POINT('Ctrl Pts',(-65.5,16.2457857930433,4.56509243789802));
#61535=CARTESIAN_POINT('Ctrl Pts',(-60.5,16.2457857930433,4.56509243789802));
#61536=CARTESIAN_POINT('Ctrl Pts',(-55.5,16.2457857930433,4.56509243789803));
#61537=CARTESIAN_POINT('Ctrl Pts',(-50.5,16.2457857930433,4.56509243789803));
#61538=CARTESIAN_POINT('Origin',(-66.,0.,0.));
#61539=CARTESIAN_POINT('',(-66.,12.8026622457696,5.81770965851215));
#61540=CARTESIAN_POINT('Ctrl Pts',(-66.,15.3459727388094,8.35923116678319));
#61541=CARTESIAN_POINT('Ctrl Pts',(-50.,15.3459727388094,8.35923116678319));
#61542=CARTESIAN_POINT('Ctrl Pts',(-66.,15.3352242315735,8.33945389776334));
#61543=CARTESIAN_POINT('Ctrl Pts',(-50.,15.3352242315735,8.33945389776334));
#61544=CARTESIAN_POINT('Ctrl Pts',(-66.,15.3136287101959,8.3000096293358));
#61545=CARTESIAN_POINT('Ctrl Pts',(-50.,15.3136287101959,8.3000096293358));
#61546=CARTESIAN_POINT('Ctrl Pts',(-66.,15.2809399078174,8.24117403498916));
#61547=CARTESIAN_POINT('Ctrl Pts',(-50.,15.2809399078174,8.24117403498916));
#61548=CARTESIAN_POINT('Ctrl Pts',(-66.,15.2367630078382,8.1633890770009));
#61549=CARTESIAN_POINT('Ctrl Pts',(-50.,15.2367630078382,8.1633890770009));
#61550=CARTESIAN_POINT('Ctrl Pts',(-66.,15.1805516924665,8.0672667757277));
#61551=CARTESIAN_POINT('Ctrl Pts',(-50.,15.1805516924665,8.0672667757277));
#61552=CARTESIAN_POINT('Ctrl Pts',(-66.,15.1233466491127,7.97225874547238));
#61553=CARTESIAN_POINT('Ctrl Pts',(-50.,15.1233466491127,7.97225874547238));
#61554=CARTESIAN_POINT('Ctrl Pts',(-66.,15.0651469569388,7.87836882722194));
#61555=CARTESIAN_POINT('Ctrl Pts',(-50.,15.0651469569388,7.87836882722194));
#61556=CARTESIAN_POINT('Ctrl Pts',(-66.,15.0059563925574,7.78559754307594));
#61557=CARTESIAN_POINT('Ctrl Pts',(-50.,15.0059563925574,7.78559754307594));
#61558=CARTESIAN_POINT('Ctrl Pts',(-66.,14.9457865336247,7.69393894021329));
#61559=CARTESIAN_POINT('Ctrl Pts',(-50.,14.9457865336247,7.69393894021329));
#61560=CARTESIAN_POINT('Ctrl Pts',(-66.,14.8846516233064,7.60338865730635));
#61561=CARTESIAN_POINT('Ctrl Pts',(-50.,14.8846516233064,7.60338865730635));
#61562=CARTESIAN_POINT('Ctrl Pts',(-66.,14.8225625096892,7.513953182008));
#61563=CARTESIAN_POINT('Ctrl Pts',(-50.,14.8225625096892,7.513953182008));
#61564=CARTESIAN_POINT('Ctrl Pts',(-66.,14.7595205830519,7.42565938179662));
#61565=CARTESIAN_POINT('Ctrl Pts',(-50.,14.7595205830519,7.42565938179662));
#61566=CARTESIAN_POINT('Ctrl Pts',(-66.,14.6955127521324,7.33856213697858));
#61567=CARTESIAN_POINT('Ctrl Pts',(-50.,14.6955127521324,7.33856213697858));
#61568=CARTESIAN_POINT('Ctrl Pts',(-66.,14.6305035247819,7.2527572990137));
#61569=CARTESIAN_POINT('Ctrl Pts',(-50.,14.6305035247819,7.2527572990137));
#61570=CARTESIAN_POINT('Ctrl Pts',(-66.,14.5644452858612,7.16836184447367));
#61571=CARTESIAN_POINT('Ctrl Pts',(-50.,14.5644452858612,7.16836184447367));
#61572=CARTESIAN_POINT('Ctrl Pts',(-66.,14.497293115392,7.08548597048793));
#61573=CARTESIAN_POINT('Ctrl Pts',(-50.,14.497293115392,7.08548597048793));
#61574=CARTESIAN_POINT('Ctrl Pts',(-66.,14.4290193778776,7.00420544769957));
#61575=CARTESIAN_POINT('Ctrl Pts',(-50.,14.4290193778776,7.00420544769957));
#61576=CARTESIAN_POINT('Ctrl Pts',(-66.,14.3596259311217,6.92453872281182));
#61577=CARTESIAN_POINT('Ctrl Pts',(-50.,14.3596259311217,6.92453872281182));
#61578=CARTESIAN_POINT('Ctrl Pts',(-66.,14.2891644580326,6.84640830625432));
#61579=CARTESIAN_POINT('Ctrl Pts',(-50.,14.2891644580326,6.84640830625432));
#61580=CARTESIAN_POINT('Ctrl Pts',(-66.,14.2177129290574,6.76968712284877));
#61581=CARTESIAN_POINT('Ctrl Pts',(-50.,14.2177129290574,6.76968712284877));
#61582=CARTESIAN_POINT('Ctrl Pts',(-66.,14.1453375866756,6.69427291666095));
#61583=CARTESIAN_POINT('Ctrl Pts',(-50.,14.1453375866756,6.69427291666095));
#61584=CARTESIAN_POINT('Ctrl Pts',(-66.,14.0720574366665,6.62015787000295));
#61585=CARTESIAN_POINT('Ctrl Pts',(-50.,14.0720574366665,6.62015787000295));
#61586=CARTESIAN_POINT('Ctrl Pts',(-66.,13.9978128588633,6.54749027478764));
#61587=CARTESIAN_POINT('Ctrl Pts',(-50.,13.9978128588633,6.54749027478764));
#61588=CARTESIAN_POINT('Ctrl Pts',(-66.,13.9224187379158,6.47666628220192));
#61589=CARTESIAN_POINT('Ctrl Pts',(-50.,13.9224187379158,6.47666628220192));
#61590=CARTESIAN_POINT('Ctrl Pts',(-66.,13.845605534933,6.40825111076043));
#61591=CARTESIAN_POINT('Ctrl Pts',(-50.,13.845605534933,6.40825111076043));
#61592=CARTESIAN_POINT('Ctrl Pts',(-66.,13.7670900956865,6.342842540489));
#61593=CARTESIAN_POINT('Ctrl Pts',(-50.,13.7670900956865,6.342842540489));
#61594=CARTESIAN_POINT('Ctrl Pts',(-66.,13.6866392230503,6.28094866827011));
#61595=CARTESIAN_POINT('Ctrl Pts',(-50.,13.6866392230503,6.28094866827011));
#61596=CARTESIAN_POINT('Ctrl Pts',(-66.,13.6041308540151,6.22286996666888));
#61597=CARTESIAN_POINT('Ctrl Pts',(-50.,13.6041308540151,6.22286996666888));
#61598=CARTESIAN_POINT('Ctrl Pts',(-66.,13.5196319660845,6.16854995125629));
#61599=CARTESIAN_POINT('Ctrl Pts',(-50.,13.5196319660845,6.16854995125629));
#61600=CARTESIAN_POINT('Ctrl Pts',(-66.,13.4333611502533,6.11764308944358));
#61601=CARTESIAN_POINT('Ctrl Pts',(-50.,13.4333611502533,6.11764308944358));
#61602=CARTESIAN_POINT('Ctrl Pts',(-66.,13.3456216156017,6.06963846112818));
#61603=CARTESIAN_POINT('Ctrl Pts',(-50.,13.3456216156017,6.06963846112818));
#61604=CARTESIAN_POINT('Ctrl Pts',(-66.,13.2567440310958,6.02396476100794));
#61605=CARTESIAN_POINT('Ctrl Pts',(-50.,13.2567440310958,6.02396476100794));
#61606=CARTESIAN_POINT('Ctrl Pts',(-66.,13.1670278530422,5.98009831397194));
#61607=CARTESIAN_POINT('Ctrl Pts',(-50.,13.1670278530422,5.98009831397194));
#61608=CARTESIAN_POINT('Ctrl Pts',(-66.,13.0766775878848,5.93768004328337));
#61609=CARTESIAN_POINT('Ctrl Pts',(-50.,13.0766775878848,5.93768004328337));
#61610=CARTESIAN_POINT('Ctrl Pts',(-66.,12.9858158402462,5.89649363499879));
#61611=CARTESIAN_POINT('Ctrl Pts',(-50.,12.9858158402462,5.89649363499879));
#61612=CARTESIAN_POINT('Ctrl Pts',(-66.,12.9127676183656,5.86444032191588));
#61613=CARTESIAN_POINT('Ctrl Pts',(-50.,12.9127676183656,5.86444032191588));
#61614=CARTESIAN_POINT('Ctrl Pts',(-66.,12.8577894805368,5.84088627843006));
#61615=CARTESIAN_POINT('Ctrl Pts',(-50.,12.8577894805368,5.84088627843006));
#61616=CARTESIAN_POINT('Ctrl Pts',(-66.,12.8210521907127,5.82539925281556));
#61617=CARTESIAN_POINT('Ctrl Pts',(-50.,12.8210521907127,5.82539925281556));
#61618=CARTESIAN_POINT('Ctrl Pts',(-66.,12.8026622457696,5.81770965851216));
#61619=CARTESIAN_POINT('Ctrl Pts',(-50.,12.8026622457696,5.81770965851216));
#61620=CARTESIAN_POINT('Origin',(-65.75,0.,0.));
#61621=CARTESIAN_POINT('',(-65.5,16.4448388443404,3.78588171813012));
#61622=CARTESIAN_POINT('Origin',(-65.5,0.,0.));
#61623=CARTESIAN_POINT('Ctrl Pts',(-65.5,16.4448388443404,3.78588171813013));
#61624=CARTESIAN_POINT('Ctrl Pts',(-65.6940750045237,16.2803340862868,3.63538534543884));
#61625=CARTESIAN_POINT('Ctrl Pts',(-65.8621879567711,16.1347706485061,3.51380187308767));
#61626=CARTESIAN_POINT('Ctrl Pts',(-66.,16.0142536207693,3.41823140961461));
#61627=CARTESIAN_POINT('Origin',(-58.,0.,0.));
#61628=CARTESIAN_POINT('',(-50.5,16.4448388443404,3.78588171813012));
#61629=CARTESIAN_POINT('Origin',(-50.5,0.,0.));
#61630=CARTESIAN_POINT('Ctrl Pts',(-50.5,16.4448388443404,3.78588171813013));
#61631=CARTESIAN_POINT('Ctrl Pts',(-55.5,16.4448388443404,3.78588171813013));
#61632=CARTESIAN_POINT('Ctrl Pts',(-60.5,16.4448388443404,3.78588171813012));
#61633=CARTESIAN_POINT('Ctrl Pts',(-65.5,16.4448388443404,3.78588171813012));
#61634=CARTESIAN_POINT('Origin',(-50.25,0.,0.));
#61635=CARTESIAN_POINT('Ctrl Pts',(-50.,16.0142536207693,3.41823140961462));
#61636=CARTESIAN_POINT('Ctrl Pts',(-50.1378120432265,16.134770648504,3.51380187308599));
#61637=CARTESIAN_POINT('Ctrl Pts',(-50.3059249954773,16.2803340862876,3.6353853454396));
#61638=CARTESIAN_POINT('Ctrl Pts',(-50.5,16.4448388443404,3.78588171813012));
#61639=CARTESIAN_POINT('Ctrl Pts',(-66.,14.0217614511585,1.06963173887291));
#61640=CARTESIAN_POINT('Ctrl Pts',(-50.,14.0217614511585,1.06963173887291));
#61641=CARTESIAN_POINT('Ctrl Pts',(-66.,14.0449730955977,1.07236559806543));
#61642=CARTESIAN_POINT('Ctrl Pts',(-50.,14.0449730955977,1.07236559806543));
#61643=CARTESIAN_POINT('Ctrl Pts',(-66.,14.0914317375174,1.07761101544474));
#61644=CARTESIAN_POINT('Ctrl Pts',(-50.,14.0914317375174,1.07761101544474));
#61645=CARTESIAN_POINT('Ctrl Pts',(-66.,14.1612257648809,1.08481225073396));
#61646=CARTESIAN_POINT('Ctrl Pts',(-50.,14.1612257648809,1.08481225073396));
#61647=CARTESIAN_POINT('Ctrl Pts',(-66.,14.2544968327758,1.09307823697967));
#61648=CARTESIAN_POINT('Ctrl Pts',(-50.,14.2544968327758,1.09307823697967));
#61649=CARTESIAN_POINT('Ctrl Pts',(-66.,14.3714293939101,1.1011284935459));
#61650=CARTESIAN_POINT('Ctrl Pts',(-50.,14.3714293939101,1.1011284935459));
#61651=CARTESIAN_POINT('Ctrl Pts',(-66.,14.4886712704316,1.10674391788617));
#61652=CARTESIAN_POINT('Ctrl Pts',(-50.,14.4886712704316,1.10674391788617));
#61653=CARTESIAN_POINT('Ctrl Pts',(-66.,14.6061528843942,1.10963588316888));
#61654=CARTESIAN_POINT('Ctrl Pts',(-50.,14.6061528843942,1.10963588316888));
#61655=CARTESIAN_POINT('Ctrl Pts',(-66.,14.7237519921366,1.10932591245462));
#61656=CARTESIAN_POINT('Ctrl Pts',(-50.,14.7237519921366,1.10932591245462));
#61657=CARTESIAN_POINT('Ctrl Pts',(-66.,14.8413329590673,1.10520035673609));
#61658=CARTESIAN_POINT('Ctrl Pts',(-50.,14.8413329590673,1.10520035673609));
#61659=CARTESIAN_POINT('Ctrl Pts',(-66.,14.9588014916819,1.09658017916666));
#61660=CARTESIAN_POINT('Ctrl Pts',(-50.,14.9588014916819,1.09658017916666));
#61661=CARTESIAN_POINT('Ctrl Pts',(-66.,15.0761445357738,1.08279356247792));
#61662=CARTESIAN_POINT('Ctrl Pts',(-50.,15.0761445357738,1.08279356247792));
#61663=CARTESIAN_POINT('Ctrl Pts',(-66.,15.1935004613832,1.06322736266735));
#61664=CARTESIAN_POINT('Ctrl Pts',(-50.,15.1935004613832,1.06322736266735));
#61665=CARTESIAN_POINT('Ctrl Pts',(-66.,15.3110884135537,1.03751150535353));
#61666=CARTESIAN_POINT('Ctrl Pts',(-50.,15.3110884135537,1.03751150535353));
#61667=CARTESIAN_POINT('Ctrl Pts',(-66.,15.4290559476364,1.00581543437186));
#61668=CARTESIAN_POINT('Ctrl Pts',(-50.,15.4290559476364,1.00581543437186));
#61669=CARTESIAN_POINT('Ctrl Pts',(-66.,15.5473762906989,0.969035923607179));
#61670=CARTESIAN_POINT('Ctrl Pts',(-50.,15.5473762906989,0.969035923607179));
#61671=CARTESIAN_POINT('Ctrl Pts',(-66.,15.6656677858244,0.929213220852553));
#61672=CARTESIAN_POINT('Ctrl Pts',(-50.,15.6656677858244,0.929213220852553));
#61673=CARTESIAN_POINT('Ctrl Pts',(-66.,15.7832573706013,0.889179733744299));
#61674=CARTESIAN_POINT('Ctrl Pts',(-50.,15.7832573706013,0.889179733744299));
#61675=CARTESIAN_POINT('Ctrl Pts',(-66.,15.8995555551237,0.851197548491309));
#61676=CARTESIAN_POINT('Ctrl Pts',(-50.,15.8995555551237,0.851197548491309));
#61677=CARTESIAN_POINT('Ctrl Pts',(-66.,16.014323697387,0.815965624774873));
#61678=CARTESIAN_POINT('Ctrl Pts',(-50.,16.014323697387,0.815965624774873));
#61679=CARTESIAN_POINT('Ctrl Pts',(-66.,16.1280496341459,0.78121969830999));
#61680=CARTESIAN_POINT('Ctrl Pts',(-50.,16.1280496341459,0.78121969830999));
#61681=CARTESIAN_POINT('Ctrl Pts',(-66.,16.2420920586203,0.741239832489433));
#61682=CARTESIAN_POINT('Ctrl Pts',(-50.,16.2420920586203,0.741239832489433));
#61683=CARTESIAN_POINT('Ctrl Pts',(-66.,16.3579063468606,0.690004279498882));
#61684=CARTESIAN_POINT('Ctrl Pts',(-50.,16.3579063468606,0.690004279498882));
#61685=CARTESIAN_POINT('Ctrl Pts',(-66.,16.4763856202025,0.623887603031702));
#61686=CARTESIAN_POINT('Ctrl Pts',(-50.,16.4763856202025,0.623887603031702));
#61687=CARTESIAN_POINT('Ctrl Pts',(-66.,16.5971869905414,0.544413618454469));
#61688=CARTESIAN_POINT('Ctrl Pts',(-50.,16.5971869905414,0.544413618454469));
#61689=CARTESIAN_POINT('Ctrl Pts',(-66.,16.717972369469,0.461363343498776));
#61690=CARTESIAN_POINT('Ctrl Pts',(-50.,16.717972369469,0.461363343498776));
#61691=CARTESIAN_POINT('Ctrl Pts',(-66.,16.8349844466884,0.390387538024311));
#61692=CARTESIAN_POINT('Ctrl Pts',(-50.,16.8349844466884,0.390387538024311));
#61693=CARTESIAN_POINT('Ctrl Pts',(-66.,16.9437808776721,0.349968584407931));
#61694=CARTESIAN_POINT('Ctrl Pts',(-50.,16.9437808776721,0.349968584407931));
#61695=CARTESIAN_POINT('Ctrl Pts',(-66.,17.0398582485081,0.358837284977383));
#61696=CARTESIAN_POINT('Ctrl Pts',(-50.,17.0398582485081,0.358837284977383));
#61697=CARTESIAN_POINT('Ctrl Pts',(-66.,17.119439942414,0.432712543166702));
#61698=CARTESIAN_POINT('Ctrl Pts',(-50.,17.119439942414,0.432712543166702));
#61699=CARTESIAN_POINT('Ctrl Pts',(-66.,17.1796877267693,0.583424648605184));
#61700=CARTESIAN_POINT('Ctrl Pts',(-50.,17.1796877267693,0.583424648605184));
#61701=CARTESIAN_POINT('Ctrl Pts',(-66.,17.2184903296471,0.819788538169111));
#61702=CARTESIAN_POINT('Ctrl Pts',(-50.,17.2184903296471,0.819788538169111));
#61703=CARTESIAN_POINT('Ctrl Pts',(-66.,17.234380239734,1.14794688939137));
#61704=CARTESIAN_POINT('Ctrl Pts',(-50.,17.234380239734,1.14794688939137));
#61705=CARTESIAN_POINT('Ctrl Pts',(-66.,17.2264039539062,1.57190599605025));
#61706=CARTESIAN_POINT('Ctrl Pts',(-50.,17.2264039539062,1.57190599605025));
#61707=CARTESIAN_POINT('Ctrl Pts',(-66.,17.1940179930072,2.09396526138803));
#61708=CARTESIAN_POINT('Ctrl Pts',(-50.,17.1940179930072,2.09396526138803));
#61709=CARTESIAN_POINT('Ctrl Pts',(-66.,17.1369791409271,2.71517078711311));
#61710=CARTESIAN_POINT('Ctrl Pts',(-50.,17.1369791409271,2.71517078711311));
#61711=CARTESIAN_POINT('Ctrl Pts',(-66.,17.0715894010097,3.29162538436688));
#61712=CARTESIAN_POINT('Ctrl Pts',(-50.,17.0715894010097,3.29162538436688));
#61713=CARTESIAN_POINT('Ctrl Pts',(-66.,17.0114557759461,3.76859236500326));
#61714=CARTESIAN_POINT('Ctrl Pts',(-50.,17.0114557759461,3.76859236500326));
#61715=CARTESIAN_POINT('Ctrl Pts',(-66.,16.9664437732891,4.10637776434634));
#61716=CARTESIAN_POINT('Ctrl Pts',(-50.,16.9664437732891,4.10637776434634));
#61717=CARTESIAN_POINT('Ctrl Pts',(-66.,16.942707041602,4.28022231927839));
#61718=CARTESIAN_POINT('Ctrl Pts',(-50.,16.942707041602,4.28022231927839));
#61719=CARTESIAN_POINT('',(-65.5,16.8706868817224,0.381509028567348));
#61720=CARTESIAN_POINT('Ctrl Pts',(-66.,16.3606547098013,0.685275467717999));
#61721=CARTESIAN_POINT('Ctrl Pts',(-65.7933280154031,16.5719640774255,0.578886349316897));
#61722=CARTESIAN_POINT('Ctrl Pts',(-65.6370761749493,16.7323564736163,0.435422691336213));
#61723=CARTESIAN_POINT('Ctrl Pts',(-65.5,16.8706868817224,0.381509028567346));
#61724=CARTESIAN_POINT('',(-66.,14.0217614511585,1.06963173887291));
#61725=CARTESIAN_POINT('',(-50.5,16.8706868817224,0.381509028567348));
#61726=CARTESIAN_POINT('Ctrl Pts',(-50.5,16.8706868817224,0.381509028567348));
#61727=CARTESIAN_POINT('Ctrl Pts',(-50.4879795588757,16.8585564547758,0.386236808645463));
#61728=CARTESIAN_POINT('Ctrl Pts',(-50.4758389600911,16.8462886142405,0.391627729214028));
#61729=CARTESIAN_POINT('Ctrl Pts',(-50.3319788807996,16.7007416155469,0.461359015551984));
#61730=CARTESIAN_POINT('Ctrl Pts',(-50.189657660532,16.5545679796152,0.587644860737737));
#61731=CARTESIAN_POINT('Ctrl Pts',(-50.,16.3606547098013,0.685275467717997));
#61732=CARTESIAN_POINT('Ctrl Pts',(-65.5,16.8706868817224,0.381509028567347));
#61733=CARTESIAN_POINT('Ctrl Pts',(-60.5,16.8706868817224,0.381509028567347));
#61734=CARTESIAN_POINT('Ctrl Pts',(-55.5,16.8706868817224,0.381509028567347));
#61735=CARTESIAN_POINT('Ctrl Pts',(-50.5,16.8706868817224,0.381509028567347));
#61736=CARTESIAN_POINT('Origin',(-66.,0.,0.));
#61737=CARTESIAN_POINT('',(-66.,13.847248627403,2.45104298226008));
#61738=CARTESIAN_POINT('Ctrl Pts',(-66.,16.942707041602,4.28022231927839));
#61739=CARTESIAN_POINT('Ctrl Pts',(-50.,16.942707041602,4.28022231927839));
#61740=CARTESIAN_POINT('Ctrl Pts',(-66.,16.9273778116851,4.26373943458434));
#61741=CARTESIAN_POINT('Ctrl Pts',(-50.,16.9273778116851,4.26373943458434));
#61742=CARTESIAN_POINT('Ctrl Pts',(-66.,16.8966513626585,4.23090496815705));
#61743=CARTESIAN_POINT('Ctrl Pts',(-50.,16.8966513626585,4.23090496815705));
#61744=CARTESIAN_POINT('Ctrl Pts',(-66.,16.8503577217978,4.18204717677295));
#61745=CARTESIAN_POINT('Ctrl Pts',(-50.,16.8503577217978,4.18204717677295));
#61746=CARTESIAN_POINT('Ctrl Pts',(-66.,16.7882243879419,4.11769232454756));
#61747=CARTESIAN_POINT('Ctrl Pts',(-50.,16.7882243879419,4.11769232454756));
#61748=CARTESIAN_POINT('Ctrl Pts',(-66.,16.7098744101503,4.03856906780257));
#61749=CARTESIAN_POINT('Ctrl Pts',(-50.,16.7098744101503,4.03856906780257));
#61750=CARTESIAN_POINT('Ctrl Pts',(-66.,16.6308390321023,3.96077220530218));
#61751=CARTESIAN_POINT('Ctrl Pts',(-50.,16.6308390321023,3.96077220530218));
#61752=CARTESIAN_POINT('Ctrl Pts',(-66.,16.5511183171041,3.88430568636484));
#61753=CARTESIAN_POINT('Ctrl Pts',(-50.,16.5511183171041,3.88430568636484));
#61754=CARTESIAN_POINT('Ctrl Pts',(-66.,16.4707160529602,3.80916907748197));
#61755=CARTESIAN_POINT('Ctrl Pts',(-50.,16.4707160529602,3.80916907748197));
#61756=CARTESIAN_POINT('Ctrl Pts',(-66.,16.3896419731869,3.73535373360533));
#61757=CARTESIAN_POINT('Ctrl Pts',(-50.,16.3896419731869,3.73535373360533));
#61758=CARTESIAN_POINT('Ctrl Pts',(-66.,16.3079087888565,3.66285188829513));
#61759=CARTESIAN_POINT('Ctrl Pts',(-50.,16.3079087888565,3.66285188829513));
#61760=CARTESIAN_POINT('Ctrl Pts',(-66.,16.2255286206571,3.59166712757322));
#61761=CARTESIAN_POINT('Ctrl Pts',(-50.,16.2255286206571,3.59166712757322));
#61762=CARTESIAN_POINT('Ctrl Pts',(-66.,16.1425094968592,3.52182512907851));
#61763=CARTESIAN_POINT('Ctrl Pts',(-50.,16.1425094968592,3.52182512907851));
#61764=CARTESIAN_POINT('Ctrl Pts',(-66.,16.058852385664,3.4533823046161));
#61765=CARTESIAN_POINT('Ctrl Pts',(-50.,16.058852385664,3.4533823046161));
#61766=CARTESIAN_POINT('Ctrl Pts',(-66.,15.9745467472627,3.38644032083441));
#61767=CARTESIAN_POINT('Ctrl Pts',(-50.,15.9745467472627,3.38644032083441));
#61768=CARTESIAN_POINT('Ctrl Pts',(-66.,15.8895755533235,3.32112432067463));
#61769=CARTESIAN_POINT('Ctrl Pts',(-50.,15.8895755533235,3.32112432067463));
#61770=CARTESIAN_POINT('Ctrl Pts',(-66.,15.8039227000236,3.2575522103651));
#61771=CARTESIAN_POINT('Ctrl Pts',(-50.,15.8039227000236,3.2575522103651));
#61772=CARTESIAN_POINT('Ctrl Pts',(-66.,15.7175802634788,3.19580425274334));
#61773=CARTESIAN_POINT('Ctrl Pts',(-50.,15.7175802634788,3.19580425274334));
#61774=CARTESIAN_POINT('Ctrl Pts',(-66.,15.6305546306352,3.13589785295852));
#61775=CARTESIAN_POINT('Ctrl Pts',(-50.,15.6305546306352,3.13589785295852));
#61776=CARTESIAN_POINT('Ctrl Pts',(-66.,15.542876589815,3.07774510290095));
#61777=CARTESIAN_POINT('Ctrl Pts',(-50.,15.542876589815,3.07774510290095));
#61778=CARTESIAN_POINT('Ctrl Pts',(-66.,15.4545900595684,3.02120352923108));
#61779=CARTESIAN_POINT('Ctrl Pts',(-50.,15.4545900595684,3.02120352923108));
#61780=CARTESIAN_POINT('Ctrl Pts',(-66.,15.3657337712291,2.96615761473811));
#61781=CARTESIAN_POINT('Ctrl Pts',(-50.,15.3657337712291,2.96615761473811));
#61782=CARTESIAN_POINT('Ctrl Pts',(-66.,15.2763241892947,2.9125950607961));
#61783=CARTESIAN_POINT('Ctrl Pts',(-50.,15.2763241892947,2.9125950607961));
#61784=CARTESIAN_POINT('Ctrl Pts',(-66.,15.1863404453747,2.86067432738731));
#61785=CARTESIAN_POINT('Ctrl Pts',(-50.,15.1863404453747,2.86067432738731));
#61786=CARTESIAN_POINT('Ctrl Pts',(-66.,15.0957017586521,2.81082515619622));
#61787=CARTESIAN_POINT('Ctrl Pts',(-50.,15.0957017586521,2.81082515619622));
#61788=CARTESIAN_POINT('Ctrl Pts',(-66.,15.0042876224246,2.76366203995482));
#61789=CARTESIAN_POINT('Ctrl Pts',(-50.,15.0042876224246,2.76366203995482));
#61790=CARTESIAN_POINT('Ctrl Pts',(-66.,14.9119724401214,2.71983439592332));
#61791=CARTESIAN_POINT('Ctrl Pts',(-50.,14.9119724401214,2.71983439592332));
#61792=CARTESIAN_POINT('Ctrl Pts',(-66.,14.8186566994895,2.67989235195328));
#61793=CARTESIAN_POINT('Ctrl Pts',(-50.,14.8186566994895,2.67989235195328));
#61794=CARTESIAN_POINT('Ctrl Pts',(-66.,14.7242968968419,2.64415729654763));
#61795=CARTESIAN_POINT('Ctrl Pts',(-50.,14.7242968968419,2.64415729654763));
#61796=CARTESIAN_POINT('Ctrl Pts',(-66.,14.6289438583545,2.61255786321175));
#61797=CARTESIAN_POINT('Ctrl Pts',(-50.,14.6289438583545,2.61255786321175));
#61798=CARTESIAN_POINT('Ctrl Pts',(-66.,14.5327233771235,2.58470501352874));
#61799=CARTESIAN_POINT('Ctrl Pts',(-50.,14.5327233771235,2.58470501352874));
#61800=CARTESIAN_POINT('Ctrl Pts',(-66.,14.4358020756955,2.56002847385863));
#61801=CARTESIAN_POINT('Ctrl Pts',(-50.,14.4358020756955,2.56002847385863));
#61802=CARTESIAN_POINT('Ctrl Pts',(-66.,14.338358156612,2.53789265347798));
#61803=CARTESIAN_POINT('Ctrl Pts',(-50.,14.338358156612,2.53789265347798));
#61804=CARTESIAN_POINT('Ctrl Pts',(-66.,14.2405514355047,2.51771585773738));
#61805=CARTESIAN_POINT('Ctrl Pts',(-50.,14.2405514355047,2.51771585773738));
#61806=CARTESIAN_POINT('Ctrl Pts',(-66.,14.1424906951186,2.49909943227153));
#61807=CARTESIAN_POINT('Ctrl Pts',(-50.,14.1424906951186,2.49909943227153));
#61808=CARTESIAN_POINT('Ctrl Pts',(-66.,14.0442408931361,2.48180336850756));
#61809=CARTESIAN_POINT('Ctrl Pts',(-50.,14.0442408931361,2.48180336850756));
#61810=CARTESIAN_POINT('Ctrl Pts',(-66.,13.9655162806582,2.46892342325417));
#61811=CARTESIAN_POINT('Ctrl Pts',(-50.,13.9655162806582,2.46892342325417));
#61812=CARTESIAN_POINT('Ctrl Pts',(-66.,13.9064077297103,2.45978188025048));
#61813=CARTESIAN_POINT('Ctrl Pts',(-50.,13.9064077297103,2.45978188025048));
#61814=CARTESIAN_POINT('Ctrl Pts',(-66.,13.8669731427486,2.45391760048539));
#61815=CARTESIAN_POINT('Ctrl Pts',(-50.,13.8669731427486,2.45391760048539));
#61816=CARTESIAN_POINT('Ctrl Pts',(-66.,13.847248627403,2.45104298226009));
#61817=CARTESIAN_POINT('Ctrl Pts',(-50.,13.847248627403,2.45104298226009));
#61818=CARTESIAN_POINT('Origin',(-65.75,0.,0.));
#61819=CARTESIAN_POINT('Origin',(-65.5,0.,0.));
#61820=CARTESIAN_POINT('Origin',(-58.,0.,0.));
#61821=CARTESIAN_POINT('Origin',(-50.5,0.,0.));
#61822=CARTESIAN_POINT('Origin',(-50.25,0.,0.));
#61823=CARTESIAN_POINT('Origin',(-35.75,0.,0.));
#61824=CARTESIAN_POINT('Origin',(-21.5,0.,0.));
#61825=CARTESIAN_POINT('Origin',(-21.25,0.,0.));
#61826=CARTESIAN_POINT('',(0.,0.,0.));
#61827=CARTESIAN_POINT('Origin',(-15.8,0.,0.));
#61828=CARTESIAN_POINT('',(-15.5,-3.03190208378603E-16,2.47573593128807));
#61829=CARTESIAN_POINT('Origin',(-15.5,0.,0.));
#61830=CARTESIAN_POINT('',(-15.587867965644,-3.29168890065668E-16,2.68786796564404));
#61831=CARTESIAN_POINT('Origin',(-15.8,-3.03190208378603E-16,2.47573593128807));
#61832=CARTESIAN_POINT('',(-15.587867965644,-2.68786796564404,-3.29168890065668E-16));
#61833=CARTESIAN_POINT('Origin',(-15.587867965644,0.,-4.11461112582085E-16));
#61834=CARTESIAN_POINT('Origin',(-15.587867965644,0.,-4.11461112582085E-16));
#61835=CARTESIAN_POINT('Origin',(-15.7,0.,0.));
#61836=CARTESIAN_POINT('',(-15.812132034356,-2.91213203435596,-3.5663331745685E-16));
#61837=CARTESIAN_POINT('',(-15.7,-2.8,-3.42901103761259E-16));
#61838=CARTESIAN_POINT('',(-15.812132034356,-3.5663331745685E-16,2.91213203435596));
#61839=CARTESIAN_POINT('Origin',(-15.812132034356,0.,-4.45791646821063E-16));
#61840=CARTESIAN_POINT('Origin',(-15.812132034356,0.,-4.45791646821063E-16));
#61841=CARTESIAN_POINT('Origin',(-15.5,0.,0.));
#61842=CARTESIAN_POINT('Origin',(-16.0242640687119,0.,0.));
#61843=CARTESIAN_POINT('',(-16.0242640687119,-3.67394039744206E-16,3.));
#61844=CARTESIAN_POINT('Origin',(-16.0242640687119,-3.30654635769785E-16,
2.7));
#61845=CARTESIAN_POINT('',(-16.0242640687119,-3.,-3.67394039744206E-16));
#61846=CARTESIAN_POINT('Origin',(-16.0242640687119,0.,0.));
#61847=CARTESIAN_POINT('Origin',(-16.0242640687119,0.,0.));
#61848=CARTESIAN_POINT('Origin',(-47.25,0.,0.));
#61849=CARTESIAN_POINT('',(-78.4757359312881,-3.,-3.67394039744206E-16));
#61850=CARTESIAN_POINT('',(-47.25,-3.,-3.67394039744206E-16));
#61851=CARTESIAN_POINT('',(-78.4757359312881,-3.67394039744206E-16,3.));
#61852=CARTESIAN_POINT('Origin',(-78.4757359312881,0.,0.));
#61853=CARTESIAN_POINT('Origin',(-78.4757359312881,0.,0.));
#61854=CARTESIAN_POINT('Origin',(-78.4757359312881,0.,0.));
#61855=CARTESIAN_POINT('',(-78.687867965644,-3.5663331745685E-16,2.91213203435596));
#61856=CARTESIAN_POINT('Origin',(-78.4757359312881,-3.30654635769785E-16,
2.7));
#61857=CARTESIAN_POINT('',(-78.687867965644,-2.91213203435597,-3.5663331745685E-16));
#61858=CARTESIAN_POINT('Origin',(-78.687867965644,0.,-4.45791646821063E-16));
#61859=CARTESIAN_POINT('Origin',(-78.687867965644,0.,-4.45791646821063E-16));
#61860=CARTESIAN_POINT('Origin',(-78.8,0.,0.));
#61861=CARTESIAN_POINT('',(-78.912132034356,-2.68786796564404,-3.29168890065668E-16));
#61862=CARTESIAN_POINT('',(-78.8,-2.8,-3.42901103761259E-16));
#61863=CARTESIAN_POINT('',(-78.912132034356,-3.29168890065668E-16,2.68786796564404));
#61864=CARTESIAN_POINT('Origin',(-78.912132034356,0.,-4.11461112582085E-16));
#61865=CARTESIAN_POINT('Origin',(-78.912132034356,0.,-4.11461112582085E-16));
#61866=CARTESIAN_POINT('Origin',(-78.7,0.,0.));
#61867=CARTESIAN_POINT('',(-79.,-3.03190208378603E-16,2.47573593128807));
#61868=CARTESIAN_POINT('Origin',(-78.7,-3.03190208378603E-16,2.47573593128807));
#61869=CARTESIAN_POINT('Origin',(-79.,0.,0.));
#61870=CARTESIAN_POINT('Origin',(-79.,2.6,0.));
#61871=CARTESIAN_POINT('',(0.,0.,0.));
#61872=CARTESIAN_POINT('Origin',(4.7,7.5,2.2));
#61873=CARTESIAN_POINT('',(5.,10.,2.2));
#61874=CARTESIAN_POINT('',(4.7,10.,2.5));
#61875=CARTESIAN_POINT('Origin',(4.7,10.,2.2));
#61876=CARTESIAN_POINT('',(4.7,0.,2.5));
#61877=CARTESIAN_POINT('',(4.7,7.5,2.5));
#61878=CARTESIAN_POINT('',(5.,0.,2.2));
#61879=CARTESIAN_POINT('Origin',(4.7,0.,2.2));
#61880=CARTESIAN_POINT('',(5.,7.5,2.2));
#61881=CARTESIAN_POINT('Origin',(4.7,0.,0.));
#61882=CARTESIAN_POINT('',(4.7,0.,-2.5));
#61883=CARTESIAN_POINT('',(5.,0.,-2.2));
#61884=CARTESIAN_POINT('Origin',(4.7,0.,-2.2));
#61885=CARTESIAN_POINT('Origin',(5.,0.,0.));
#61886=CARTESIAN_POINT('Origin',(4.7,0.,0.));
#61887=CARTESIAN_POINT('Origin',(4.7,2.5,-2.2));
#61888=CARTESIAN_POINT('',(4.7,10.,-2.5));
#61889=CARTESIAN_POINT('',(5.,10.,-2.2));
#61890=CARTESIAN_POINT('Origin',(4.7,10.,-2.2));
#61891=CARTESIAN_POINT('',(5.,2.5,-2.2));
#61892=CARTESIAN_POINT('',(4.7,2.5,-2.5));
#61893=CARTESIAN_POINT('Origin',(4.7,10.,0.));
#61894=CARTESIAN_POINT('Origin',(5.,10.,0.));
#61895=CARTESIAN_POINT('Origin',(4.7,10.,0.));
#61896=CARTESIAN_POINT('Origin',(0.,0.,0.));
#61897=CARTESIAN_POINT('',(0.3,0.,2.5));
#61898=CARTESIAN_POINT('',(0.,0.,2.5));
#61899=CARTESIAN_POINT('',(0.3,0.,-2.5));
#61900=CARTESIAN_POINT('Origin',(0.3,0.,0.));
#61901=CARTESIAN_POINT('',(0.,0.,-2.5));
#61902=CARTESIAN_POINT('Origin',(0.,10.,2.5));
#61903=CARTESIAN_POINT('',(0.3,10.,2.5));
#61904=CARTESIAN_POINT('',(0.,10.,2.5));
#61905=CARTESIAN_POINT('',(0.3,7.5,2.5));
#61906=CARTESIAN_POINT('Origin',(5.,5.,0.));
#61907=CARTESIAN_POINT('',(5.,-1.92881870865708E-16,-1.575));
#61908=CARTESIAN_POINT('Origin',(5.,0.,0.));
#61909=CARTESIAN_POINT('Origin',(0.3,7.5,2.2));
#61910=CARTESIAN_POINT('',(0.,0.,2.2));
#61911=CARTESIAN_POINT('Origin',(0.3,0.,2.2));
#61912=CARTESIAN_POINT('',(0.,10.,2.2));
#61913=CARTESIAN_POINT('Origin',(0.3,10.,2.2));
#61914=CARTESIAN_POINT('',(0.,7.5,2.2));
#61915=CARTESIAN_POINT('Origin',(0.3,10.,0.));
#61916=CARTESIAN_POINT('',(0.3,10.,-2.5));
#61917=CARTESIAN_POINT('',(0.,10.,-2.2));
#61918=CARTESIAN_POINT('Origin',(0.3,10.,-2.2));
#61919=CARTESIAN_POINT('Origin',(0.,10.,0.));
#61920=CARTESIAN_POINT('Origin',(0.3,10.,0.));
#61921=CARTESIAN_POINT('Origin',(0.3,2.5,-2.2));
#61922=CARTESIAN_POINT('',(0.,0.,-2.2));
#61923=CARTESIAN_POINT('Origin',(0.3,0.,-2.2));
#61924=CARTESIAN_POINT('',(0.,2.5,-2.2));
#61925=CARTESIAN_POINT('',(0.3,2.5,-2.5));
#61926=CARTESIAN_POINT('Origin',(0.3,0.,0.));
#61927=CARTESIAN_POINT('Origin',(0.,0.,0.));
#61928=CARTESIAN_POINT('Origin',(0.,10.,0.));
#61929=CARTESIAN_POINT('',(0.,10.,-2.5));
#61930=CARTESIAN_POINT('Origin',(0.,5.,0.));
#61931=CARTESIAN_POINT('',(0.,1.92881870865708E-16,1.575));
#61932=CARTESIAN_POINT('Origin',(0.,0.,0.));
#61933=CARTESIAN_POINT('Origin',(0.3,0.,0.));
#61934=CARTESIAN_POINT('',(0.3,-1.56142466891288E-16,1.275));
#61935=CARTESIAN_POINT('Origin',(0.3,-1.92881870865708E-16,1.575));
#61936=CARTESIAN_POINT('Origin',(0.3,0.,0.));
#61937=CARTESIAN_POINT('Origin',(0.,0.,0.));
#61938=CARTESIAN_POINT('',(4.7,1.56142466891288E-16,1.275));
#61939=CARTESIAN_POINT('',(0.,-1.56142466891288E-16,1.275));
#61940=CARTESIAN_POINT('',(4.7,-1.56142466891288E-16,-1.275));
#61941=CARTESIAN_POINT('Origin',(4.7,0.,0.));
#61942=CARTESIAN_POINT('Origin',(4.7,0.,0.));
#61943=CARTESIAN_POINT('Origin',(4.7,0.,0.));
#61944=CARTESIAN_POINT('Origin',(4.7,-1.92881870865708E-16,-1.575));
#61945=CARTESIAN_POINT('Origin',(0.,0.,-2.5));
#61946=CARTESIAN_POINT('',(0.,0.,0.));
#61947=CARTESIAN_POINT('Origin',(9.8,0.,0.));
#61948=CARTESIAN_POINT('',(10.,-1.06196139652526E-16,0.867157287525381));
#61949=CARTESIAN_POINT('Origin',(10.,0.,0.));
#61950=CARTESIAN_POINT('',(9.94142135623731,-1.23515260777236E-16,1.00857864376269));
#61951=CARTESIAN_POINT('Origin',(9.8,-1.06196139652526E-16,0.867157287525381));
#61952=CARTESIAN_POINT('',(9.94142135623731,-1.00857864376269,-1.23515260777236E-16));
#61953=CARTESIAN_POINT('Origin',(9.94142135623731,0.,-1.54394075971545E-16));
#61954=CARTESIAN_POINT('Origin',(9.94142135623731,0.,-1.54394075971545E-16));
#61955=CARTESIAN_POINT('Origin',(9.85,0.,0.));
#61956=CARTESIAN_POINT('',(9.75857864376269,-1.19142135623731,-1.45907035035182E-16));
#61957=CARTESIAN_POINT('',(9.85,-1.1,-1.34711147906209E-16));
#61958=CARTESIAN_POINT('',(9.75857864376269,-1.45907035035182E-16,1.19142135623731));
#61959=CARTESIAN_POINT('Origin',(9.75857864376269,0.,-1.82383793793977E-16));
#61960=CARTESIAN_POINT('Origin',(9.75857864376269,0.,-1.82383793793977E-16));
#61961=CARTESIAN_POINT('Origin',(10.,0.,0.));
#61962=CARTESIAN_POINT('Origin',(9.61715728752538,0.,0.));
#61963=CARTESIAN_POINT('',(9.61715728752538,-1.53080849893419E-16,1.25));
#61964=CARTESIAN_POINT('Origin',(9.61715728752538,-1.28587913910472E-16,
1.05));
#61965=CARTESIAN_POINT('',(9.61715728752538,-1.25,-1.53080849893419E-16));
#61966=CARTESIAN_POINT('Origin',(9.61715728752538,0.,0.));
#61967=CARTESIAN_POINT('Origin',(9.61715728752538,0.,0.));
#61968=CARTESIAN_POINT('Origin',(5.,0.,0.));
#61969=CARTESIAN_POINT('',(0.382842712474619,-1.25,-1.53080849893419E-16));
#61970=CARTESIAN_POINT('',(5.,-1.25,-1.53080849893419E-16));
#61971=CARTESIAN_POINT('',(0.382842712474619,-1.53080849893419E-16,1.25));
#61972=CARTESIAN_POINT('Origin',(0.382842712474619,0.,0.));
#61973=CARTESIAN_POINT('Origin',(0.382842712474619,0.,0.));
#61974=CARTESIAN_POINT('Origin',(0.382842712474619,0.,0.));
#61975=CARTESIAN_POINT('',(0.241421356237309,-1.45907035035182E-16,1.19142135623731));
#61976=CARTESIAN_POINT('Origin',(0.382842712474619,-1.28587913910472E-16,
1.05));
#61977=CARTESIAN_POINT('',(0.24142135623731,-1.19142135623731,-1.45907035035182E-16));
#61978=CARTESIAN_POINT('Origin',(0.241421356237309,0.,-1.82383793793977E-16));
#61979=CARTESIAN_POINT('Origin',(0.241421356237309,0.,-1.82383793793977E-16));
#61980=CARTESIAN_POINT('Origin',(0.15,0.,0.));
#61981=CARTESIAN_POINT('',(0.0585786437626904,-1.00857864376269,-1.23515260777236E-16));
#61982=CARTESIAN_POINT('',(0.15,-1.1,-1.34711147906209E-16));
#61983=CARTESIAN_POINT('',(0.0585786437626905,-1.23515260777236E-16,1.00857864376269));
#61984=CARTESIAN_POINT('Origin',(0.0585786437626905,0.,-1.54394075971545E-16));
#61985=CARTESIAN_POINT('Origin',(0.0585786437626905,0.,-1.54394075971545E-16));
#61986=CARTESIAN_POINT('Origin',(0.2,0.,0.));
#61987=CARTESIAN_POINT('',(0.,-1.06196139652526E-16,0.867157287525381));
#61988=CARTESIAN_POINT('Origin',(0.2,-1.06196139652526E-16,0.867157287525381));
#61989=CARTESIAN_POINT('Origin',(0.,0.,0.));
#61990=CARTESIAN_POINT('Origin',(0.,0.95,0.));
#61991=CARTESIAN_POINT('',(0.,0.,0.));
#61992=CARTESIAN_POINT('Origin',(-74.5,0.,0.));
#61993=CARTESIAN_POINT('',(-74.5,40.0309056454797,-14.5700581056735));
#61994=CARTESIAN_POINT('Origin',(-74.5,40.5947212179512,-14.7752701916689));
#61995=CARTESIAN_POINT('',(-74.5,42.6,0.));
#61996=CARTESIAN_POINT('Origin',(-74.5,0.,0.));
#61997=CARTESIAN_POINT('Origin',(-74.5,43.2,0.));
#61998=CARTESIAN_POINT('Origin',(-74.5,40.5947212179512,-14.7752701916689));
#61999=CARTESIAN_POINT('Origin',(-74.5,43.2,0.));
#62000=CARTESIAN_POINT('',(0.,0.,0.));
#62001=CARTESIAN_POINT('Origin',(-6.69999999999999,-19.75,2.6));
#62002=CARTESIAN_POINT('',(-7.09999999999999,-21.2403502950465,2.6));
#62003=CARTESIAN_POINT('',(-7.,-20.9392803321658,2.86457513110645));
#62004=CARTESIAN_POINT('Ctrl Pts',(-7.09999999999999,-21.2403502950465,
2.59999999999964));
#62005=CARTESIAN_POINT('Ctrl Pts',(-7.1,-21.2390201143488,2.61086673229779));
#62006=CARTESIAN_POINT('Ctrl Pts',(-7.09955586847657,-21.2371830675583,
2.62168006860561));
#62007=CARTESIAN_POINT('Ctrl Pts',(-7.09868849358987,-21.2348575067649,
2.63236487415456));
#62008=CARTESIAN_POINT('Ctrl Pts',(-7.09693748140351,-21.2301627832357,
2.65393481468648));
#62009=CARTESIAN_POINT('Ctrl Pts',(-7.09345958992832,-21.2235106692755,
2.67487809903275));
#62010=CARTESIAN_POINT('Ctrl Pts',(-7.08092182655856,-21.2013035537358,
2.72631763724185));
#62011=CARTESIAN_POINT('Ctrl Pts',(-7.06990173845251,-21.1830658893345,
2.75455791698437));
#62012=CARTESIAN_POINT('Ctrl Pts',(-7.04472545150511,-21.1345591360924,
2.80504815321184));
#62013=CARTESIAN_POINT('Ctrl Pts',(-7.03094322851031,-21.1040599206881,
2.8253852234994));
#62014=CARTESIAN_POINT('Ctrl Pts',(-7.0101394940111,-21.0367728935879,2.85316918621411));
#62015=CARTESIAN_POINT('Ctrl Pts',(-7.00306375646934,-21.0013304617958,
2.8610826404679));
#62016=CARTESIAN_POINT('Ctrl Pts',(-7.00027014871753,-20.9564045695961,
2.86426972203768));
#62017=CARTESIAN_POINT('Ctrl Pts',(-6.99999999947518,-20.9478389844979,
2.86457513170154));
#62018=CARTESIAN_POINT('Ctrl Pts',(-7.,-20.9392803321658,2.86457513110645));
#62019=CARTESIAN_POINT('',(-7.09999999999999,-21.9,2.6));
#62020=CARTESIAN_POINT('',(-7.09999999999999,-19.75,2.6));
#62021=CARTESIAN_POINT('',(-6.69999999999999,-21.9,3.));
#62022=CARTESIAN_POINT('Origin',(-6.69999999999999,-21.9,2.6));
#62023=CARTESIAN_POINT('',(-6.69999999999999,-19.3,3.));
#62024=CARTESIAN_POINT('',(-6.69999999999999,-19.75,3.));
#62025=CARTESIAN_POINT('',(-7.,-19.,2.86457513110648));
#62026=CARTESIAN_POINT('Origin',(-6.69999999999999,-19.3,2.6));
#62027=CARTESIAN_POINT('',(-7.,-19.75,2.86457513110645));
#62028=CARTESIAN_POINT('Origin',(-6.69999999999999,-21.9,1.5));
#62029=CARTESIAN_POINT('',(-6.69999999999999,-22.3,-2.6));
#62030=CARTESIAN_POINT('',(-6.69999999999999,-22.3,2.6));
#62031=CARTESIAN_POINT('',(-6.69999999999999,-22.3,1.5));
#62032=CARTESIAN_POINT('Origin',(-6.69999999999999,-21.9,2.6));
#62033=CARTESIAN_POINT('',(-7.09999999999999,-21.9,-3.));
#62034=CARTESIAN_POINT('',(-7.09999999999999,-21.9,1.5));
#62035=CARTESIAN_POINT('Origin',(-6.69999999999999,-21.9,-2.6));
#62036=CARTESIAN_POINT('Origin',(-3.89999999999999,-21.9,-2.6));
#62037=CARTESIAN_POINT('',(-3.89999999999999,-22.3,-2.6));
#62038=CARTESIAN_POINT('',(-3.49999999999999,-21.9,-2.6));
#62039=CARTESIAN_POINT('Origin',(-3.89999999999999,-21.9,-2.6));
#62040=CARTESIAN_POINT('',(-3.89999999999999,-21.9,-3.));
#62041=CARTESIAN_POINT('Origin',(-3.89999999999999,-21.9,-2.6));
#62042=CARTESIAN_POINT('Origin',(-3.89999999999999,-21.9,-2.6));
#62043=CARTESIAN_POINT('Origin',(-7.09999999999999,-21.9,-2.6));
#62044=CARTESIAN_POINT('',(-7.09999999999999,-21.9,-3.));
#62045=CARTESIAN_POINT('',(-7.09999999999999,-22.3,-2.6));
#62046=CARTESIAN_POINT('Origin',(-3.89999999999999,-21.45,-2.6));
#62047=CARTESIAN_POINT('',(-3.89999999999999,-19.3,-3.));
#62048=CARTESIAN_POINT('',(-3.49999999999999,-19.3,-2.6));
#62049=CARTESIAN_POINT('Origin',(-3.89999999999999,-19.3,-2.6));
#62050=CARTESIAN_POINT('',(-3.49999999999999,-21.45,-2.6));
#62051=CARTESIAN_POINT('',(-3.89999999999999,-21.45,-3.));
#62052=CARTESIAN_POINT('Origin',(-3.89999999999999,-19.3,-2.6));
#62053=CARTESIAN_POINT('',(-3.89999999999999,-18.9,-2.6));
#62054=CARTESIAN_POINT('Origin',(-3.89999999999999,-19.3,-2.6));
#62055=CARTESIAN_POINT('Origin',(-3.89999999999999,-19.3,-2.6));
#62056=CARTESIAN_POINT('Origin',(-3.89999999999999,-21.9,2.6));
#62057=CARTESIAN_POINT('',(-3.89999999999999,-22.3,2.6));
#62058=CARTESIAN_POINT('',(-3.49999999999999,-21.9,2.6));
#62059=CARTESIAN_POINT('Origin',(-3.89999999999999,-21.9,2.6));
#62060=CARTESIAN_POINT('',(-3.89999999999999,-21.9,3.));
#62061=CARTESIAN_POINT('Origin',(-3.89999999999999,-21.9,2.6));
#62062=CARTESIAN_POINT('Origin',(-3.89999999999999,-21.9,2.6));
#62063=CARTESIAN_POINT('Origin',(-3.89999999999999,-21.9,1.5));
#62064=CARTESIAN_POINT('',(-3.89999999999999,-22.3,1.5));
#62065=CARTESIAN_POINT('',(-3.49999999999999,-21.9,1.5));
#62066=CARTESIAN_POINT('Origin',(-6.69999999999999,-21.9,2.6));
#62067=CARTESIAN_POINT('Origin',(-6.69999999999999,-21.9,2.6));
#62068=CARTESIAN_POINT('Origin',(-7.09999999999999,-19.3,2.6));
#62069=CARTESIAN_POINT('',(-3.89999999999999,-19.3,3.));
#62070=CARTESIAN_POINT('',(-7.09999999999999,-19.3,3.));
#62071=CARTESIAN_POINT('',(-3.89999999999999,-18.9,2.6));
#62072=CARTESIAN_POINT('Origin',(-3.89999999999999,-19.3,2.6));
#62073=CARTESIAN_POINT('',(-7.,-18.9,2.6));
#62074=CARTESIAN_POINT('',(-7.09999999999999,-18.9,2.6));
#62075=CARTESIAN_POINT('Origin',(-7.,-19.3,2.6));
#62076=CARTESIAN_POINT('Origin',(-7.09999999999999,-18.9,3.));
#62077=CARTESIAN_POINT('',(-7.09999999999999,-21.9,3.));
#62078=CARTESIAN_POINT('',(-3.89999999999999,-19.75,3.));
#62079=CARTESIAN_POINT('Origin',(-7.09999999999999,-22.3,3.));
#62080=CARTESIAN_POINT('',(-7.09999999999999,-22.3,2.6));
#62081=CARTESIAN_POINT('Origin',(-7.09999999999999,-21.9,2.6));
#62082=CARTESIAN_POINT('Origin',(-7.09999999999999,-19.3,-2.6));
#62083=CARTESIAN_POINT('',(-7.,-19.3,-3.));
#62084=CARTESIAN_POINT('',(-7.09999999999999,-19.3,-3.));
#62085=CARTESIAN_POINT('',(-7.,-18.9,-2.6));
#62086=CARTESIAN_POINT('Origin',(-7.,-19.3,-2.6));
#62087=CARTESIAN_POINT('',(-7.09999999999999,-18.9,-2.6));
#62088=CARTESIAN_POINT('Origin',(-3.89999999999999,-19.3,2.6));
#62089=CARTESIAN_POINT('',(-3.49999999999999,-19.3,2.6));
#62090=CARTESIAN_POINT('Origin',(-3.89999999999999,-19.3,2.6));
#62091=CARTESIAN_POINT('Origin',(-3.89999999999999,-19.3,2.6));
#62092=CARTESIAN_POINT('Origin',(-3.89999999999999,-19.75,2.6));
#62093=CARTESIAN_POINT('',(-3.49999999999999,-19.75,2.6));
#62094=CARTESIAN_POINT('Origin',(-3.89999999999999,-19.3,-1.5));
#62095=CARTESIAN_POINT('',(-3.89999999999999,-18.9,-1.5));
#62096=CARTESIAN_POINT('',(-3.49999999999999,-19.3,-1.5));
#62097=CARTESIAN_POINT('Origin',(-3.49999999999999,-20.6,2.22044604925031E-15));
#62098=CARTESIAN_POINT('Origin',(-7.09999999999999,-20.6,2.22044604925031E-15));
#62099=CARTESIAN_POINT('',(-7.10000000571368,-21.1875548662612,-3.));
#62100=CARTESIAN_POINT('Origin',(-7.09999999999999,0.,0.));
#62101=CARTESIAN_POINT('',(-7.09999999999999,-21.45,-3.));
#62102=CARTESIAN_POINT('Origin',(-6.69999999999999,2.6,19.75));
#62103=CARTESIAN_POINT('',(-7.09999999999999,2.6,21.2403502950465));
#62104=CARTESIAN_POINT('',(-7.,2.86457513110645,20.9392803321658));
#62105=CARTESIAN_POINT('Ctrl Pts',(-7.09999999999999,2.59999999999964,21.2403502950465));
#62106=CARTESIAN_POINT('Ctrl Pts',(-7.1,2.61086673229779,21.2390201143488));
#62107=CARTESIAN_POINT('Ctrl Pts',(-7.09955586847657,2.62168006860561,21.2371830675583));
#62108=CARTESIAN_POINT('Ctrl Pts',(-7.09868849358987,2.63236487415455,21.2348575067649));
#62109=CARTESIAN_POINT('Ctrl Pts',(-7.09693748140351,2.65393481468647,21.2301627832357));
#62110=CARTESIAN_POINT('Ctrl Pts',(-7.09345958992833,2.67487809903273,21.2235106692755));
#62111=CARTESIAN_POINT('Ctrl Pts',(-7.08092182655855,2.72631763724185,21.2013035537358));
#62112=CARTESIAN_POINT('Ctrl Pts',(-7.06990173845251,2.75455791698437,21.1830658893345));
#62113=CARTESIAN_POINT('Ctrl Pts',(-7.0447254515051,2.80504815321185,21.1345591360924));
#62114=CARTESIAN_POINT('Ctrl Pts',(-7.0309432285103,2.8253852234994,21.1040599206881));
#62115=CARTESIAN_POINT('Ctrl Pts',(-7.0101394940111,2.85316918621411,21.0367728935879));
#62116=CARTESIAN_POINT('Ctrl Pts',(-7.00306375646934,2.8610826404679,21.0013304617958));
#62117=CARTESIAN_POINT('Ctrl Pts',(-7.00027014871753,2.86426972203768,20.9564045695961));
#62118=CARTESIAN_POINT('Ctrl Pts',(-6.99999999947518,2.86457513170154,20.9478389844979));
#62119=CARTESIAN_POINT('Ctrl Pts',(-7.,2.86457513110645,20.9392803321658));
#62120=CARTESIAN_POINT('',(-7.09999999999999,2.6,21.9));
#62121=CARTESIAN_POINT('',(-7.09999999999999,2.6,19.75));
#62122=CARTESIAN_POINT('',(-6.69999999999999,3.,21.9));
#62123=CARTESIAN_POINT('Origin',(-6.69999999999999,2.6,21.9));
#62124=CARTESIAN_POINT('',(-6.69999999999999,3.,19.3));
#62125=CARTESIAN_POINT('',(-6.69999999999999,3.,19.75));
#62126=CARTESIAN_POINT('',(-7.,2.86457513110643,19.));
#62127=CARTESIAN_POINT('Origin',(-6.69999999999999,2.6,19.3));
#62128=CARTESIAN_POINT('',(-7.,2.86457513110645,19.75));
#62129=CARTESIAN_POINT('Origin',(-3.89999999999999,1.5,21.9));
#62130=CARTESIAN_POINT('',(-3.89999999999999,-2.6,22.3));
#62131=CARTESIAN_POINT('',(-3.49999999999999,-2.6,21.9));
#62132=CARTESIAN_POINT('Origin',(-3.89999999999999,-2.6,21.9));
#62133=CARTESIAN_POINT('',(-3.49999999999999,2.6,21.9));
#62134=CARTESIAN_POINT('',(-3.49999999999999,1.5,21.9));
#62135=CARTESIAN_POINT('',(-3.89999999999999,2.6,22.3));
#62136=CARTESIAN_POINT('Origin',(-3.89999999999999,2.6,21.9));
#62137=CARTESIAN_POINT('',(-3.89999999999999,1.5,22.3));
#62138=CARTESIAN_POINT('Origin',(-3.89999999999999,2.6,21.9));
#62139=CARTESIAN_POINT('',(-3.89999999999999,3.,21.9));
#62140=CARTESIAN_POINT('Origin',(-3.89999999999999,2.6,21.9));
#62141=CARTESIAN_POINT('Origin',(-3.89999999999999,2.6,21.9));
#62142=CARTESIAN_POINT('Origin',(-6.69999999999999,1.5,21.9));
#62143=CARTESIAN_POINT('',(-6.69999999999999,-2.6,22.3));
#62144=CARTESIAN_POINT('',(-6.69999999999999,2.6,22.3));
#62145=CARTESIAN_POINT('',(-6.69999999999999,1.5,22.3));
#62146=CARTESIAN_POINT('Origin',(-6.69999999999999,2.6,21.9));
#62147=CARTESIAN_POINT('',(-7.09999999999999,-3.,21.9));
#62148=CARTESIAN_POINT('',(-7.09999999999999,1.5,21.9));
#62149=CARTESIAN_POINT('Origin',(-6.69999999999999,-2.6,21.9));
#62150=CARTESIAN_POINT('Origin',(-7.09999999999999,-2.6,21.9));
#62151=CARTESIAN_POINT('',(-3.89999999999999,-3.,21.9));
#62152=CARTESIAN_POINT('',(-7.09999999999999,-3.,21.9));
#62153=CARTESIAN_POINT('Origin',(-3.89999999999999,-2.6,21.9));
#62154=CARTESIAN_POINT('',(-7.09999999999999,-2.6,22.3));
#62155=CARTESIAN_POINT('Origin',(-3.89999999999999,-2.6,21.9));
#62156=CARTESIAN_POINT('Origin',(-3.89999999999999,-2.6,21.9));
#62157=CARTESIAN_POINT('Origin',(-6.69999999999999,2.6,21.9));
#62158=CARTESIAN_POINT('Origin',(-6.69999999999999,2.6,21.9));
#62159=CARTESIAN_POINT('Origin',(-7.09999999999999,2.6,19.3));
#62160=CARTESIAN_POINT('',(-3.89999999999999,3.,19.3));
#62161=CARTESIAN_POINT('',(-7.09999999999999,3.,19.3));
#62162=CARTESIAN_POINT('',(-3.89999999999999,2.6,18.9));
#62163=CARTESIAN_POINT('Origin',(-3.89999999999999,2.6,19.3));
#62164=CARTESIAN_POINT('',(-7.,2.6,18.9));
#62165=CARTESIAN_POINT('',(-7.09999999999999,2.6,18.9));
#62166=CARTESIAN_POINT('Origin',(-7.,2.6,19.3));
#62167=CARTESIAN_POINT('Origin',(-7.09999999999999,3.,18.9));
#62168=CARTESIAN_POINT('',(-7.09999999999999,3.,21.9));
#62169=CARTESIAN_POINT('',(-3.89999999999999,3.,19.75));
#62170=CARTESIAN_POINT('Origin',(-7.09999999999999,2.6,21.9));
#62171=CARTESIAN_POINT('',(-7.09999999999999,2.6,22.3));
#62172=CARTESIAN_POINT('Origin',(-3.89999999999999,-2.6,19.3));
#62173=CARTESIAN_POINT('',(-3.89999999999999,-3.,19.3));
#62174=CARTESIAN_POINT('',(-3.49999999999999,-2.6,19.3));
#62175=CARTESIAN_POINT('Origin',(-3.89999999999999,-2.6,19.3));
#62176=CARTESIAN_POINT('',(-3.89999999999999,-2.6,18.9));
#62177=CARTESIAN_POINT('Origin',(-3.89999999999999,-2.6,19.3));
#62178=CARTESIAN_POINT('Origin',(-3.89999999999999,-2.6,19.3));
#62179=CARTESIAN_POINT('Origin',(-7.09999999999999,-2.6,19.3));
#62180=CARTESIAN_POINT('',(-7.,-3.,19.3));
#62181=CARTESIAN_POINT('',(-7.,-2.6,18.9));
#62182=CARTESIAN_POINT('Origin',(-7.,-2.6,19.3));
#62183=CARTESIAN_POINT('',(-7.09999999999999,-2.6,18.9));
#62184=CARTESIAN_POINT('',(-7.09999999999999,-3.,19.3));
#62185=CARTESIAN_POINT('Origin',(-3.89999999999999,2.6,19.3));
#62186=CARTESIAN_POINT('',(-3.49999999999999,2.6,19.3));
#62187=CARTESIAN_POINT('Origin',(-3.89999999999999,2.6,19.3));
#62188=CARTESIAN_POINT('Origin',(-3.89999999999999,2.6,19.3));
#62189=CARTESIAN_POINT('Origin',(-3.89999999999999,2.6,19.75));
#62190=CARTESIAN_POINT('',(-3.49999999999999,2.6,19.75));
#62191=CARTESIAN_POINT('Origin',(-3.89999999999999,-1.5,19.3));
#62192=CARTESIAN_POINT('',(-3.49999999999999,-1.5,19.3));
#62193=CARTESIAN_POINT('',(-3.89999999999999,-1.5,18.9));
#62194=CARTESIAN_POINT('Origin',(-3.89999999999999,-2.6,21.45));
#62195=CARTESIAN_POINT('',(-3.89999999999999,-3.,21.45));
#62196=CARTESIAN_POINT('',(-3.49999999999999,-2.6,21.45));
#62197=CARTESIAN_POINT('Origin',(-3.49999999999999,1.11022302462516E-15,
20.6));
#62198=CARTESIAN_POINT('Origin',(-7.09999999999999,1.11022302462516E-15,
20.6));
#62199=CARTESIAN_POINT('',(-7.09999999999999,-2.62060817839527E-15,21.3988897061572));
#62200=CARTESIAN_POINT('Origin',(-7.09999999999999,0.,0.));
#62201=CARTESIAN_POINT('',(-7.10000000571368,-3.,21.1875548662612));
#62202=CARTESIAN_POINT('Origin',(-7.09999999999999,0.,0.));
#62203=CARTESIAN_POINT('',(-7.09999999999999,-3.,21.45));
#62204=CARTESIAN_POINT('Origin',(-3.89999999999999,21.9,-1.5));
#62205=CARTESIAN_POINT('',(-3.49999999999999,21.9,-2.6));
#62206=CARTESIAN_POINT('',(-3.89999999999999,22.3,-2.6));
#62207=CARTESIAN_POINT('Origin',(-3.89999999999999,21.9,-2.6));
#62208=CARTESIAN_POINT('',(-3.89999999999999,22.3,2.6));
#62209=CARTESIAN_POINT('',(-3.89999999999999,22.3,-1.5));
#62210=CARTESIAN_POINT('',(-3.49999999999999,21.9,2.6));
#62211=CARTESIAN_POINT('Origin',(-3.89999999999999,21.9,2.6));
#62212=CARTESIAN_POINT('',(-3.49999999999999,21.9,-1.5));
#62213=CARTESIAN_POINT('Origin',(-3.89999999999999,21.9,2.6));
#62214=CARTESIAN_POINT('',(-3.89999999999999,21.9,3.));
#62215=CARTESIAN_POINT('Origin',(-3.89999999999999,21.9,2.6));
#62216=CARTESIAN_POINT('Origin',(-3.89999999999999,21.9,2.6));
#62217=CARTESIAN_POINT('Origin',(-3.89999999999999,21.9,-2.6));
#62218=CARTESIAN_POINT('',(-3.89999999999999,21.9,-3.));
#62219=CARTESIAN_POINT('Origin',(-3.89999999999999,21.9,-2.6));
#62220=CARTESIAN_POINT('Origin',(-3.89999999999999,21.9,-2.6));
#62221=CARTESIAN_POINT('Origin',(-7.09999999999999,21.9,-2.6));
#62222=CARTESIAN_POINT('',(-6.69999999999999,21.9,-3.));
#62223=CARTESIAN_POINT('',(-7.09999999999999,21.9,-3.));
#62224=CARTESIAN_POINT('',(-6.69999999999999,22.3,-2.6));
#62225=CARTESIAN_POINT('Origin',(-6.69999999999999,21.9,-2.6));
#62226=CARTESIAN_POINT('',(-7.09999999999999,22.3,-2.6));
#62227=CARTESIAN_POINT('Origin',(-3.89999999999999,19.75,-2.6));
#62228=CARTESIAN_POINT('',(-3.49999999999999,19.3,-2.6));
#62229=CARTESIAN_POINT('',(-3.49999999999999,19.75,-2.6));
#62230=CARTESIAN_POINT('',(-3.89999999999999,19.3,-3.));
#62231=CARTESIAN_POINT('Origin',(-3.89999999999999,19.3,-2.6));
#62232=CARTESIAN_POINT('',(-3.89999999999999,19.75,-3.));
#62233=CARTESIAN_POINT('Origin',(-3.49999999999999,20.6,0.));
#62234=CARTESIAN_POINT('',(-3.49999999999999,19.3,2.6));
#62235=CARTESIAN_POINT('',(-3.49999999999999,21.45,2.6));
#62236=CARTESIAN_POINT('',(-3.49999999999999,19.3,1.5));
#62237=CARTESIAN_POINT('Origin',(-6.69999999999999,19.75,-2.6));
#62238=CARTESIAN_POINT('',(-7.09999999999999,21.2403502950465,-2.6));
#62239=CARTESIAN_POINT('',(-7.,20.9392803321658,-2.86457513110645));
#62240=CARTESIAN_POINT('Ctrl Pts',(-7.09999999999999,21.2403502950465,-2.59999999999964));
#62241=CARTESIAN_POINT('Ctrl Pts',(-7.1,21.2390201143488,-2.61086673229778));
#62242=CARTESIAN_POINT('Ctrl Pts',(-7.09955586847657,21.2371830675583,-2.6216800686056));
#62243=CARTESIAN_POINT('Ctrl Pts',(-7.09868849358987,21.2348575067649,-2.63236487415455));
#62244=CARTESIAN_POINT('Ctrl Pts',(-7.09693748140351,21.2301627832357,-2.6539348146865));
#62245=CARTESIAN_POINT('Ctrl Pts',(-7.09345958992831,21.2235106692755,-2.67487809903278));
#62246=CARTESIAN_POINT('Ctrl Pts',(-7.08092182655856,21.2013035537358,-2.72631763724183));
#62247=CARTESIAN_POINT('Ctrl Pts',(-7.06990173845252,21.1830658893345,-2.75455791698435));
#62248=CARTESIAN_POINT('Ctrl Pts',(-7.04472545150511,21.1345591360924,-2.80504815321183));
#62249=CARTESIAN_POINT('Ctrl Pts',(-7.03094322851031,21.1040599206881,-2.82538522349939));
#62250=CARTESIAN_POINT('Ctrl Pts',(-7.01013949401111,21.0367728935879,-2.8531691862141));
#62251=CARTESIAN_POINT('Ctrl Pts',(-7.00306375646934,21.0013304617958,-2.8610826404679));
#62252=CARTESIAN_POINT('Ctrl Pts',(-7.00027014871753,20.9564045695961,-2.86426972203768));
#62253=CARTESIAN_POINT('Ctrl Pts',(-6.99999999947518,20.9478389844979,-2.86457513170154));
#62254=CARTESIAN_POINT('Ctrl Pts',(-7.,20.9392803321658,-2.86457513110645));
#62255=CARTESIAN_POINT('',(-7.09999999999999,21.9,-2.6));
#62256=CARTESIAN_POINT('',(-7.09999999999999,19.75,-2.6));
#62257=CARTESIAN_POINT('Origin',(-6.69999999999999,21.9,-2.6));
#62258=CARTESIAN_POINT('',(-6.69999999999999,19.3,-3.));
#62259=CARTESIAN_POINT('',(-6.69999999999999,19.75,-3.));
#62260=CARTESIAN_POINT('',(-7.,19.,-2.86457513110643));
#62261=CARTESIAN_POINT('Origin',(-6.69999999999999,19.3,-2.6));
#62262=CARTESIAN_POINT('',(-7.,19.75,-2.86457513110645));
#62263=CARTESIAN_POINT('Origin',(-6.69999999999999,21.9,-1.5));
#62264=CARTESIAN_POINT('Origin',(-6.69999999999999,21.9,-2.6));
#62265=CARTESIAN_POINT('',(-7.09999999999999,21.9,2.6));
#62266=CARTESIAN_POINT('',(-7.09999999999999,21.9,-1.5));
#62267=CARTESIAN_POINT('',(-6.69999999999999,22.3,2.6));
#62268=CARTESIAN_POINT('Origin',(-6.69999999999999,21.9,2.6));
#62269=CARTESIAN_POINT('',(-6.69999999999999,22.3,-1.5));
#62270=CARTESIAN_POINT('Origin',(-6.69999999999999,21.45,2.6));
#62271=CARTESIAN_POINT('',(-7.,19.,2.86457513110643));
#62272=CARTESIAN_POINT('',(-6.69999999999999,19.3,3.));
#62273=CARTESIAN_POINT('Origin',(-6.69999999999999,19.3,2.6));
#62274=CARTESIAN_POINT('',(-6.69999999999999,21.9,3.));
#62275=CARTESIAN_POINT('',(-6.69999999999999,21.45,3.));
#62276=CARTESIAN_POINT('Origin',(-6.69999999999999,21.9,2.6));
#62277=CARTESIAN_POINT('',(-7.09999999999999,21.2403502950465,2.6));
#62278=CARTESIAN_POINT('',(-7.09999999999999,21.45,2.6));
#62279=CARTESIAN_POINT('',(-7.,20.939280330552,2.86457513110645));
#62280=CARTESIAN_POINT('Ctrl Pts',(-7.,20.9392803305521,2.86457513110645));
#62281=CARTESIAN_POINT('Ctrl Pts',(-6.9999999978217,20.9726487442632,2.86457513357641));
#62282=CARTESIAN_POINT('Ctrl Pts',(-7.00418879911678,21.0059157565623,2.86000991879761));
#62283=CARTESIAN_POINT('Ctrl Pts',(-7.01958904143543,21.0718993033474,2.84089197849509));
#62284=CARTESIAN_POINT('Ctrl Pts',(-7.03129369231811,21.1035538664428,2.82549715408756));
#62285=CARTESIAN_POINT('Ctrl Pts',(-7.05699818661693,21.160006242706,2.7822473587533));
#62286=CARTESIAN_POINT('Ctrl Pts',(-7.07049988125604,21.1834359928131,2.75458608787846));
#62287=CARTESIAN_POINT('Ctrl Pts',(-7.08973887000163,21.2168017558866,2.69454207075082));
#62288=CARTESIAN_POINT('Ctrl Pts',(-7.09610571805172,21.2279327022523,2.66418093757161));
#62289=CARTESIAN_POINT('Ctrl Pts',(-7.09868849358987,21.2348575067649,2.63236487415455));
#62290=CARTESIAN_POINT('Ctrl Pts',(-7.09954198702743,21.2371458493331,2.62185106800518));
#62291=CARTESIAN_POINT('Ctrl Pts',(-7.09998646943438,21.2389629679018,2.61120519714679));
#62292=CARTESIAN_POINT('Ctrl Pts',(-7.09999989834893,21.2403098710973,2.60032927350281));
#62293=CARTESIAN_POINT('Ctrl Pts',(-7.09999999999999,21.2403301414833,2.60016464182416));
#62294=CARTESIAN_POINT('Ctrl Pts',(-7.09999999999999,21.2403502950465,2.6));
#62295=CARTESIAN_POINT('',(-7.,21.45,2.86457513110645));
#62296=CARTESIAN_POINT('Origin',(-6.69999999999999,21.9,2.6));
#62297=CARTESIAN_POINT('Origin',(-6.69999999999999,21.9,2.6));
#62298=CARTESIAN_POINT('Origin',(-6.69999999999999,21.9,-2.6));
#62299=CARTESIAN_POINT('Origin',(-7.09999999999999,19.3,-2.6));
#62300=CARTESIAN_POINT('',(-7.09999999999999,19.3,-3.));
#62301=CARTESIAN_POINT('',(-3.89999999999999,18.9,-2.6));
#62302=CARTESIAN_POINT('Origin',(-3.89999999999999,19.3,-2.6));
#62303=CARTESIAN_POINT('',(-7.,18.9,-2.6));
#62304=CARTESIAN_POINT('',(-7.09999999999999,18.9,-2.6));
#62305=CARTESIAN_POINT('Origin',(-7.,19.3,-2.6));
#62306=CARTESIAN_POINT('Origin',(-7.09999999999999,18.9,-3.));
#62307=CARTESIAN_POINT('Origin',(-7.09999999999999,22.3,-3.));
#62308=CARTESIAN_POINT('',(-7.09999999999999,22.3,2.6));
#62309=CARTESIAN_POINT('Origin',(-7.09999999999999,21.9,2.6));
#62310=CARTESIAN_POINT('',(-7.09999999999999,21.9,3.));
#62311=CARTESIAN_POINT('Origin',(-7.09999999999999,22.3,3.));
#62312=CARTESIAN_POINT('',(-3.89999999999999,19.3,3.));
#62313=CARTESIAN_POINT('',(-7.09999999999999,19.3,3.));
#62314=CARTESIAN_POINT('',(-3.89999999999999,21.45,3.));
#62315=CARTESIAN_POINT('Origin',(-7.09999999999999,19.3,2.6));
#62316=CARTESIAN_POINT('',(-7.,18.9,2.6));
#62317=CARTESIAN_POINT('Origin',(-7.,19.3,2.6));
#62318=CARTESIAN_POINT('',(-3.89999999999999,18.9,2.6));
#62319=CARTESIAN_POINT('',(-7.09999999999999,18.9,2.6));
#62320=CARTESIAN_POINT('Origin',(-3.89999999999999,19.3,2.6));
#62321=CARTESIAN_POINT('Origin',(-7.4,0.,0.));
#62322=CARTESIAN_POINT('',(-7.,-3.,20.9203071812343));
#62323=CARTESIAN_POINT('Ctrl Pts',(-7.10000000898043,-3.,21.187554863459));
#62324=CARTESIAN_POINT('Ctrl Pts',(-7.0714456188059,-3.,21.1548542805031));
#62325=CARTESIAN_POINT('Ctrl Pts',(-7.04641393471848,-3.,21.113705953019));
#62326=CARTESIAN_POINT('Ctrl Pts',(-7.01162679116877,-3.,21.0292320043449));
#62327=CARTESIAN_POINT('Ctrl Pts',(-7.,-3.,20.9703351236358));
#62328=CARTESIAN_POINT('Ctrl Pts',(-7.,-3.,20.9203071812343));
#62329=CARTESIAN_POINT('',(-7.11715728752538,-2.62284531190034E-15,21.4171572875254));
#62330=CARTESIAN_POINT('Origin',(-7.4,-2.58820706965092E-15,21.1343145750508));
#62331=CARTESIAN_POINT('',(-7.11715728752538,-21.4171572875254,-2.62284531190034E-15));
#62332=CARTESIAN_POINT('Origin',(-7.11715728752538,-1.11022302462516E-15,
-1.11022302462516E-15));
#62333=CARTESIAN_POINT('Origin',(-7.11715728752538,-1.11022302462516E-15,
-1.11022302462516E-15));
#62334=CARTESIAN_POINT('Origin',(-7.,0.,0.));
#62335=CARTESIAN_POINT('Origin',(-7.09999999999999,0.,0.));
#62336=CARTESIAN_POINT('',(-7.,2.86457513110645,-20.9392803571529));
#62337=CARTESIAN_POINT('Origin',(-7.,0.,0.));
#62338=CARTESIAN_POINT('',(-7.09999999999999,2.6,-21.2403502950465));
#62339=CARTESIAN_POINT('Ctrl Pts',(-7.09999999999999,2.6,-21.2403502950465));
#62340=CARTESIAN_POINT('Ctrl Pts',(-7.09999999999999,2.6003921713453,-21.2403022899296));
#62341=CARTESIAN_POINT('Ctrl Pts',(-7.09999942325386,2.6007842840571,-21.2402536221204));
#62342=CARTESIAN_POINT('Ctrl Pts',(-7.09999630362454,2.60184507611363,-21.2401201486839));
#62343=CARTESIAN_POINT('Ctrl Pts',(-7.09999266043989,2.60251362028008,-21.240034081592));
#62344=CARTESIAN_POINT('Ctrl Pts',(-7.09997602470054,2.60460481765257,-21.2397587769154));
#62345=CARTESIAN_POINT('Ctrl Pts',(-7.09995712122886,2.60602658190596,-21.2395627811672));
#62346=CARTESIAN_POINT('Ctrl Pts',(-7.09977488248242,2.61581335410445,-21.2381530086686));
#62347=CARTESIAN_POINT('Ctrl Pts',(-7.09935699857395,2.62412985850796,-21.2366498678362));
#62348=CARTESIAN_POINT('Ctrl Pts',(-7.09868849358987,2.63236487415455,-21.2348575067649));
#62349=CARTESIAN_POINT('Ctrl Pts',(-7.09715565553086,2.6512472246232,-21.2307477404491));
#62350=CARTESIAN_POINT('Ctrl Pts',(-7.09430136895356,2.66965802332072,-21.225133614234));
#62351=CARTESIAN_POINT('Ctrl Pts',(-7.08497519397776,2.71137287081551,-21.2083557037175));
#62352=CARTESIAN_POINT('Ctrl Pts',(-7.0776055735118,2.73375616436245,-21.1960045404144));
#62353=CARTESIAN_POINT('Ctrl Pts',(-7.05934927081274,2.77755052489804,-21.1632306404314));
#62354=CARTESIAN_POINT('Ctrl Pts',(-7.04831649738891,2.7976105486174,-21.1421536207631));
#62355=CARTESIAN_POINT('Ctrl Pts',(-7.02658383602801,2.83193954938331,-21.0909146928277));
#62356=CARTESIAN_POINT('Ctrl Pts',(-7.01639288683744,2.84497738989315,-21.0607499422713));
#62357=CARTESIAN_POINT('Ctrl Pts',(-7.00341459029669,2.86082920681864,-20.9995815899696));
#62358=CARTESIAN_POINT('Ctrl Pts',(-6.99999999999998,2.86457513110647,-20.9694560416778));
#62359=CARTESIAN_POINT('Ctrl Pts',(-7.,2.86457513110645,-20.9392803571526));
#62360=CARTESIAN_POINT('',(-7.09999999999999,-2.6,-21.2403502950465));
#62361=CARTESIAN_POINT('Origin',(-7.09999999999999,0.,0.));
#62362=CARTESIAN_POINT('',(-7.,-2.86457513110646,-20.9392803571529));
#62363=CARTESIAN_POINT('Ctrl Pts',(-7.,-2.86457513110646,-20.9392803571526));
#62364=CARTESIAN_POINT('Ctrl Pts',(-6.99999999999998,-2.86457513110648,
-20.9618455210744));
#62365=CARTESIAN_POINT('Ctrl Pts',(-7.00189590232315,-2.86246650530523,
-20.9844202381741));
#62366=CARTESIAN_POINT('Ctrl Pts',(-7.01140185478759,-2.85122632172449,
-21.0436263038058));
#62367=CARTESIAN_POINT('Ctrl Pts',(-7.02201855971974,-2.83837640858004,
-21.0785265213582));
#62368=CARTESIAN_POINT('Ctrl Pts',(-7.04364595086458,-2.80538967801371,
-21.1319953593187));
#62369=CARTESIAN_POINT('Ctrl Pts',(-7.05354342289825,-2.78840016518533,
-21.1519891336581));
#62370=CARTESIAN_POINT('Ctrl Pts',(-7.0689762416833,-2.7551424923852,-21.1807205825222));
#62371=CARTESIAN_POINT('Ctrl Pts',(-7.07477587083774,-2.74074065264234,
-21.1908445906006));
#62372=CARTESIAN_POINT('Ctrl Pts',(-7.08922373671821,-2.69693339673472,
-21.2159198464697));
#62373=CARTESIAN_POINT('Ctrl Pts',(-7.09600316823805,-2.66544420312709,
-21.227657750983));
#62374=CARTESIAN_POINT('Ctrl Pts',(-7.09868849358987,-2.63236487415455,
-21.2348575067649));
#62375=CARTESIAN_POINT('Ctrl Pts',(-7.09936536158736,-2.62402683826439,
-21.2366722903163));
#62376=CARTESIAN_POINT('Ctrl Pts',(-7.09978524624839,-2.61560576952592,
-21.238190470791));
#62377=CARTESIAN_POINT('Ctrl Pts',(-7.09996050880447,-2.60578130232895,
-21.2395967409211));
#62378=CARTESIAN_POINT('Ctrl Pts',(-7.09997780022238,-2.60442682623069,
-21.2397826271377));
#62379=CARTESIAN_POINT('Ctrl Pts',(-7.09999323912115,-2.60241617783349,
-21.2400466815348));
#62380=CARTESIAN_POINT('Ctrl Pts',(-7.09999666166736,-2.60176080456852,
-21.2401308801099));
#62381=CARTESIAN_POINT('Ctrl Pts',(-7.09999949086643,-2.60073687963955,
-21.2402595033544));
#62382=CARTESIAN_POINT('Ctrl Pts',(-7.09999999999999,-2.60036846778023,
-21.2403051914481));
#62383=CARTESIAN_POINT('Ctrl Pts',(-7.09999999999999,-2.59999999999997,
-21.2403502950465));
#62384=CARTESIAN_POINT('',(-7.,-20.9203071812343,-3.));
#62385=CARTESIAN_POINT('Origin',(-7.,0.,0.));
#62386=CARTESIAN_POINT('Ctrl Pts',(-7.10000000898044,-21.187554863459,-3.));
#62387=CARTESIAN_POINT('Ctrl Pts',(-7.0714456188059,-21.1548542805032,-3.));
#62388=CARTESIAN_POINT('Ctrl Pts',(-7.04641393471848,-21.113705953019,-3.));
#62389=CARTESIAN_POINT('Ctrl Pts',(-7.01162679116877,-21.0292320043449,
-3.));
#62390=CARTESIAN_POINT('Ctrl Pts',(-7.,-20.9703351236358,-3.));
#62391=CARTESIAN_POINT('Ctrl Pts',(-7.,-20.9203071812343,-3.));
#62392=CARTESIAN_POINT('Origin',(-7.,0.,0.));
#62393=CARTESIAN_POINT('Origin',(-7.,7.05,0.));
#62394=CARTESIAN_POINT('',(-7.,-2.86457513110643,-19.));
#62395=CARTESIAN_POINT('',(-7.,-2.86457513110646,-19.75));
#62396=CARTESIAN_POINT('',(-7.,-2.6,-18.9));
#62397=CARTESIAN_POINT('Origin',(-7.,-2.6,-19.3));
#62398=CARTESIAN_POINT('',(-7.,2.6,-18.9));
#62399=CARTESIAN_POINT('',(-7.,5.025,-18.9));
#62400=CARTESIAN_POINT('',(-7.,2.86457513110645,-19.));
#62401=CARTESIAN_POINT('Origin',(-7.,2.6,-19.3));
#62402=CARTESIAN_POINT('',(-7.,2.86457513110645,-21.45));
#62403=CARTESIAN_POINT('',(-7.,18.9,1.5));
#62404=CARTESIAN_POINT('',(-7.,2.025,18.9));
#62405=CARTESIAN_POINT('',(-7.,-3.,11.15));
#62406=CARTESIAN_POINT('',(-7.,-18.9,-1.5));
#62407=CARTESIAN_POINT('',(-7.,-7.625,-3.));
#62408=CARTESIAN_POINT('',(-7.,-10.7968626966597,6.52035061571116E-16));
#62409=CARTESIAN_POINT('Origin',(-7.,0.,0.));
#62410=CARTESIAN_POINT('Origin',(-7.25,0.,0.));
#62411=CARTESIAN_POINT('',(-7.38284271247462,-21.6828427124746,-2.65538239242476E-15));
#62412=CARTESIAN_POINT('',(-7.25,-21.55,-2.63911385216255E-15));
#62413=CARTESIAN_POINT('',(-7.38284271247462,-2.65538239242476E-15,21.6828427124746));
#62414=CARTESIAN_POINT('Origin',(-7.38284271247462,0.,-3.31922799053094E-15));
#62415=CARTESIAN_POINT('Origin',(-7.38284271247462,0.,-3.31922799053094E-15));
#62416=CARTESIAN_POINT('Origin',(-10.4,0.,0.));
#62417=CARTESIAN_POINT('',(-10.,-2.76770176607302E-15,22.6));
#62418=CARTESIAN_POINT('Origin',(-10.,0.,0.));
#62419=CARTESIAN_POINT('',(-10.4,-2.81668763803891E-15,23.));
#62420=CARTESIAN_POINT('Origin',(-10.4,-2.76770176607302E-15,22.6));
#62421=CARTESIAN_POINT('',(-10.4,-23.,-2.81668763803891E-15));
#62422=CARTESIAN_POINT('Origin',(-10.4,0.,0.));
#62423=CARTESIAN_POINT('Origin',(-10.4,0.,0.));
#62424=CARTESIAN_POINT('Origin',(-11.45,0.,0.));
#62425=CARTESIAN_POINT('',(-12.7343145750508,-23.,-2.81668763803891E-15));
#62426=CARTESIAN_POINT('',(-11.45,-23.,-2.81668763803891E-15));
#62427=CARTESIAN_POINT('',(-12.7343145750508,-2.81668763803891E-15,23.));
#62428=CARTESIAN_POINT('Origin',(-12.7343145750508,0.,0.));
#62429=CARTESIAN_POINT('Origin',(-12.7343145750508,0.,0.));
#62430=CARTESIAN_POINT('Origin',(-10.,21.8,0.));
#62431=CARTESIAN_POINT('',(-10.,-21.8,-2.66973002214123E-15));
#62432=CARTESIAN_POINT('Origin',(-10.,0.,0.));
#62433=CARTESIAN_POINT('Origin',(-3.89999999999999,19.3,2.6));
#62434=CARTESIAN_POINT('Origin',(-3.89999999999999,19.3,2.6));
#62435=CARTESIAN_POINT('Origin',(-3.89999999999999,19.3,2.6));
#62436=CARTESIAN_POINT('Origin',(-3.89999999999999,19.3,1.5));
#62437=CARTESIAN_POINT('Origin',(-3.89999999999999,19.3,-2.6));
#62438=CARTESIAN_POINT('',(-3.89999999999999,18.9,1.5));
#62439=CARTESIAN_POINT('Origin',(-3.89999999999999,21.45,2.6));
#62440=CARTESIAN_POINT('Origin',(-3.89999999999999,19.3,-2.6));
#62441=CARTESIAN_POINT('Origin',(-7.09999999999999,20.6,0.));
#62442=CARTESIAN_POINT('Origin',(-7.09999999999999,18.9,3.));
#62443=CARTESIAN_POINT('Origin',(-6.69999999999999,2.6,-21.45));
#62444=CARTESIAN_POINT('',(-6.69999999999999,3.,-19.3));
#62445=CARTESIAN_POINT('Origin',(-6.69999999999999,2.6,-19.3));
#62446=CARTESIAN_POINT('',(-6.69999999999999,3.,-21.9));
#62447=CARTESIAN_POINT('',(-6.69999999999999,3.,-21.45));
#62448=CARTESIAN_POINT('',(-7.09999999999999,2.6,-21.9));
#62449=CARTESIAN_POINT('Origin',(-6.69999999999999,2.6,-21.9));
#62450=CARTESIAN_POINT('',(-7.09999999999999,2.6,-21.45));
#62451=CARTESIAN_POINT('Origin',(-7.09999999999999,2.6,-21.9));
#62452=CARTESIAN_POINT('',(-6.69999999999999,2.6,-22.3));
#62453=CARTESIAN_POINT('Origin',(-6.69999999999999,2.6,-21.9));
#62454=CARTESIAN_POINT('',(-3.89999999999999,3.,-21.9));
#62455=CARTESIAN_POINT('',(-7.09999999999999,3.,-21.9));
#62456=CARTESIAN_POINT('',(-3.89999999999999,2.6,-22.3));
#62457=CARTESIAN_POINT('Origin',(-3.89999999999999,2.6,-21.9));
#62458=CARTESIAN_POINT('',(-7.09999999999999,2.6,-22.3));
#62459=CARTESIAN_POINT('Origin',(-3.89999999999999,2.6,-21.45));
#62460=CARTESIAN_POINT('',(-3.49999999999999,2.6,-21.9));
#62461=CARTESIAN_POINT('Origin',(-3.89999999999999,2.6,-21.9));
#62462=CARTESIAN_POINT('',(-3.89999999999999,3.,-19.3));
#62463=CARTESIAN_POINT('',(-3.89999999999999,3.,-21.45));
#62464=CARTESIAN_POINT('',(-3.49999999999999,2.6,-19.3));
#62465=CARTESIAN_POINT('Origin',(-3.89999999999999,2.6,-19.3));
#62466=CARTESIAN_POINT('',(-3.49999999999999,2.6,-21.45));
#62467=CARTESIAN_POINT('Origin',(-3.89999999999999,2.6,-19.3));
#62468=CARTESIAN_POINT('',(-3.89999999999999,2.6,-18.9));
#62469=CARTESIAN_POINT('Origin',(-3.89999999999999,2.6,-19.3));
#62470=CARTESIAN_POINT('Origin',(-3.89999999999999,2.6,-19.3));
#62471=CARTESIAN_POINT('Origin',(-3.89999999999999,2.6,-21.9));
#62472=CARTESIAN_POINT('Origin',(-3.89999999999999,2.6,-21.9));
#62473=CARTESIAN_POINT('Origin',(-6.69999999999999,2.6,-21.9));
#62474=CARTESIAN_POINT('Origin',(-6.69999999999999,2.6,-21.9));
#62475=CARTESIAN_POINT('Origin',(-7.09999999999999,-3.88578058618805E-15,
-20.6));
#62476=CARTESIAN_POINT('',(-7.09999999999999,-2.6,-21.9));
#62477=CARTESIAN_POINT('',(-7.09999999999999,-1.5,-21.9));
#62478=CARTESIAN_POINT('',(-7.09999999999999,-2.6,-19.75));
#62479=CARTESIAN_POINT('Origin',(-6.69999999999999,-1.5,-21.9));
#62480=CARTESIAN_POINT('',(-6.69999999999999,-2.6,-22.3));
#62481=CARTESIAN_POINT('',(-6.69999999999999,-1.5,-22.3));
#62482=CARTESIAN_POINT('Origin',(-6.69999999999999,-2.6,-21.9));
#62483=CARTESIAN_POINT('Origin',(-7.09999999999999,-3.,-22.3));
#62484=CARTESIAN_POINT('',(-3.89999999999999,-2.6,-22.3));
#62485=CARTESIAN_POINT('',(-3.89999999999999,-1.5,-22.3));
#62486=CARTESIAN_POINT('',(-7.09999999999999,-2.6,-22.3));
#62487=CARTESIAN_POINT('Origin',(-3.89999999999999,-1.5,-21.9));
#62488=CARTESIAN_POINT('',(-3.49999999999999,-2.6,-21.9));
#62489=CARTESIAN_POINT('',(-3.49999999999999,-1.5,-21.9));
#62490=CARTESIAN_POINT('Origin',(-3.89999999999999,-2.6,-21.9));
#62491=CARTESIAN_POINT('Origin',(-3.49999999999999,-3.88578058618805E-15,
-20.6));
#62492=CARTESIAN_POINT('',(-3.49999999999999,-2.6,-19.3));
#62493=CARTESIAN_POINT('',(-3.49999999999999,1.5,-19.3));
#62494=CARTESIAN_POINT('',(-3.49999999999999,-2.6,-19.75));
#62495=CARTESIAN_POINT('Origin',(-12.7343145750508,0.,0.));
#62496=CARTESIAN_POINT('',(-13.0171572875254,-2.80234000832244E-15,22.8828427124746));
#62497=CARTESIAN_POINT('Origin',(-12.7343145750508,-2.76770176607302E-15,
22.6));
#62498=CARTESIAN_POINT('',(-13.0171572875254,-22.8828427124746,-2.80234000832244E-15));
#62499=CARTESIAN_POINT('Origin',(-13.0171572875254,0.,-3.50292501040305E-15));
#62500=CARTESIAN_POINT('Origin',(-13.0171572875254,0.,-3.50292501040305E-15));
#62501=CARTESIAN_POINT('Origin',(-13.2,0.,0.));
#62502=CARTESIAN_POINT('',(-13.3828427124746,-22.5171572875254,-2.75755645980654E-15));
#62503=CARTESIAN_POINT('',(-13.2,-22.7,-2.77994823406449E-15));
#62504=CARTESIAN_POINT('',(-13.3828427124746,-2.75755645980654E-15,22.5171572875254));
#62505=CARTESIAN_POINT('Origin',(-13.3828427124746,0.,-3.44694557475818E-15));
#62506=CARTESIAN_POINT('Origin',(-13.3828427124746,0.,-3.44694557475818E-15));
#62507=CARTESIAN_POINT('Origin',(-7.66568542494924,0.,0.));
#62508=CARTESIAN_POINT('',(-7.66568542494924,-2.66973002214123E-15,21.8));
#62509=CARTESIAN_POINT('Origin',(-7.66568542494924,-2.62074415017534E-15,
21.4));
#62510=CARTESIAN_POINT('',(-7.66568542494924,-21.8,-2.66973002214123E-15));
#62511=CARTESIAN_POINT('Origin',(-7.66568542494924,0.,0.));
#62512=CARTESIAN_POINT('Origin',(-7.66568542494924,0.,0.));
#62513=CARTESIAN_POINT('Origin',(-8.75,0.,0.));
#62514=CARTESIAN_POINT('',(-8.75,-21.8,-2.66973002214123E-15));
#62515=CARTESIAN_POINT('Origin',(-7.4,0.,0.));
#62516=CARTESIAN_POINT('',(-7.45,-10.4,3.17533340522386E-15));
#62517=CARTESIAN_POINT('Origin',(-7.45,0.,0.));
#62518=CARTESIAN_POINT('Origin',(-7.4,-10.7968626966597,3.29650373003067E-15));
#62519=CARTESIAN_POINT('Origin',(-13.1,0.,0.));
#62520=CARTESIAN_POINT('',(-13.5,-2.72291821755713E-15,22.2343145750508));
#62521=CARTESIAN_POINT('Origin',(-13.1,-2.72291821755713E-15,22.2343145750508));
#62522=CARTESIAN_POINT('Origin',(-13.5,0.,0.));
#62523=CARTESIAN_POINT('Origin',(-13.5,22.4,0.));
#62524=CARTESIAN_POINT('',(-13.5,-9.12361865364778E-16,7.45));
#62525=CARTESIAN_POINT('Origin',(-13.5,0.,0.));
#62526=CARTESIAN_POINT('Origin',(-6.69999999999999,-2.6,-19.75));
#62527=CARTESIAN_POINT('',(-6.69999999999999,-3.,-21.9));
#62528=CARTESIAN_POINT('Origin',(-6.69999999999999,-2.6,-21.9));
#62529=CARTESIAN_POINT('',(-6.69999999999999,-3.,-19.3));
#62530=CARTESIAN_POINT('',(-6.69999999999999,-3.,-19.75));
#62531=CARTESIAN_POINT('Origin',(-6.69999999999999,-2.6,-19.3));
#62532=CARTESIAN_POINT('Origin',(-6.69999999999999,-2.6,-21.9));
#62533=CARTESIAN_POINT('Origin',(-6.69999999999999,-2.6,-21.9));
#62534=CARTESIAN_POINT('Origin',(-7.09999999999999,-2.6,-19.3));
#62535=CARTESIAN_POINT('',(-3.89999999999999,-3.,-19.3));
#62536=CARTESIAN_POINT('',(-7.09999999999999,-3.,-19.3));
#62537=CARTESIAN_POINT('',(-3.89999999999999,-2.6,-18.9));
#62538=CARTESIAN_POINT('Origin',(-3.89999999999999,-2.6,-19.3));
#62539=CARTESIAN_POINT('',(-7.09999999999999,-2.6,-18.9));
#62540=CARTESIAN_POINT('Origin',(-7.09999999999999,-3.,-18.9));
#62541=CARTESIAN_POINT('',(-3.89999999999999,-3.,-21.9));
#62542=CARTESIAN_POINT('',(-7.09999999999999,-3.,-21.9));
#62543=CARTESIAN_POINT('',(-3.89999999999999,-3.,-19.75));
#62544=CARTESIAN_POINT('Origin',(-7.09999999999999,-2.6,-21.9));
#62545=CARTESIAN_POINT('Origin',(-3.89999999999999,-2.6,-21.9));
#62546=CARTESIAN_POINT('Origin',(-7.09999999999999,3.,-22.3));
#62547=CARTESIAN_POINT('',(-7.09999999999999,3.,-19.3));
#62548=CARTESIAN_POINT('Origin',(-3.89999999999999,-2.6,-21.9));
#62549=CARTESIAN_POINT('Origin',(-3.89999999999999,-2.6,-21.9));
#62550=CARTESIAN_POINT('Origin',(-7.09999999999999,2.6,-19.3));
#62551=CARTESIAN_POINT('',(-7.09999999999999,2.6,-18.9));
#62552=CARTESIAN_POINT('Origin',(-3.89999999999999,-2.6,-19.3));
#62553=CARTESIAN_POINT('Origin',(-3.89999999999999,-2.6,-19.3));
#62554=CARTESIAN_POINT('Origin',(-3.89999999999999,-2.6,-19.3));
#62555=CARTESIAN_POINT('Origin',(-3.89999999999999,-2.6,-19.75));
#62556=CARTESIAN_POINT('Origin',(-3.89999999999999,1.5,-19.3));
#62557=CARTESIAN_POINT('',(-3.89999999999999,1.5,-18.9));
#62558=CARTESIAN_POINT('Origin',(-13.1,0.,0.));
#62559=CARTESIAN_POINT('',(-13.1,-8.63375993398884E-16,7.05));
#62560=CARTESIAN_POINT('Origin',(-13.1,-9.12361865364778E-16,7.45));
#62561=CARTESIAN_POINT('',(-13.1,-7.05,-8.63375993398884E-16));
#62562=CARTESIAN_POINT('Origin',(-13.1,0.,0.));
#62563=CARTESIAN_POINT('Origin',(-13.1,0.,0.));
#62564=CARTESIAN_POINT('Origin',(-10.25,0.,0.));
#62565=CARTESIAN_POINT('',(-11.95,-7.05,8.63375993398884E-16));
#62566=CARTESIAN_POINT('',(-11.95,-8.63375993398884E-16,7.05));
#62567=CARTESIAN_POINT('Origin',(-11.95,0.,0.));
#62568=CARTESIAN_POINT('',(-10.25,-7.05,-8.63375993398884E-16));
#62569=CARTESIAN_POINT('Origin',(-11.95,0.,0.));
#62570=CARTESIAN_POINT('Origin',(-11.95,0.,0.));
#62571=CARTESIAN_POINT('',(-11.55,-9.12361865364778E-16,7.45));
#62572=CARTESIAN_POINT('Origin',(-11.95,-9.12361865364778E-16,7.45));
#62573=CARTESIAN_POINT('Origin',(-11.55,0.,0.));
#62574=CARTESIAN_POINT('Origin',(-11.55,10.4,0.));
#62575=CARTESIAN_POINT('',(-11.55,-10.4,-1.27363267111325E-15));
#62576=CARTESIAN_POINT('Origin',(-11.55,0.,0.));
#62577=CARTESIAN_POINT('Origin',(-9.5,0.,0.));
#62578=CARTESIAN_POINT('',(-9.5,-10.4,-1.27363267111325E-15));
#62579=CARTESIAN_POINT('Origin',(-7.09999999999999,3.,-18.9));
#62580=CARTESIAN_POINT('Origin',(-7.09999999999999,-3.,18.9));
#62581=CARTESIAN_POINT('Origin',(-7.09999999999999,-3.,22.3));
#62582=CARTESIAN_POINT('Origin',(-7.09999999999999,3.,22.3));
#62583=CARTESIAN_POINT('Origin',(-7.09999999999999,-18.9,-3.));
#62584=CARTESIAN_POINT('Origin',(-7.09999999999999,-22.3,-3.));
#62585=CARTESIAN_POINT('',(0.,0.,0.));
#62586=CARTESIAN_POINT('Origin',(-7.8,9.9,1.7));
#62587=CARTESIAN_POINT('',(-7.5,9.6,1.7));
#62588=CARTESIAN_POINT('',(-7.8,9.6,2.));
#62589=CARTESIAN_POINT('',(-7.5,9.6,1.7));
#62590=CARTESIAN_POINT('',(-7.8,9.9,1.7));
#62591=CARTESIAN_POINT('',(-7.8,9.9,1.7));
#62592=CARTESIAN_POINT('',(-7.8,9.6,2.));
#62593=CARTESIAN_POINT('Origin',(-7.5,-9.6,1.7));
#62594=CARTESIAN_POINT('',(-7.8,-9.9,1.7));
#62595=CARTESIAN_POINT('',(-7.8,-9.6,2.));
#62596=CARTESIAN_POINT('',(-7.8,-9.9,1.7));
#62597=CARTESIAN_POINT('',(-7.5,-9.6,1.7));
#62598=CARTESIAN_POINT('',(-7.5,-9.6,1.7));
#62599=CARTESIAN_POINT('',(-7.8,-9.6,2.));
#62600=CARTESIAN_POINT('Origin',(-11.5,9.6,1.7));
#62601=CARTESIAN_POINT('',(-11.2,9.9,1.7));
#62602=CARTESIAN_POINT('',(-11.2,9.6,2.));
#62603=CARTESIAN_POINT('',(-11.2,9.9,1.7));
#62604=CARTESIAN_POINT('',(-11.5,9.6,1.7));
#62605=CARTESIAN_POINT('',(-11.5,9.6,1.7));
#62606=CARTESIAN_POINT('',(-11.2,9.6,2.));
#62607=CARTESIAN_POINT('Origin',(-7.5,9.6,-1.7));
#62608=CARTESIAN_POINT('',(-7.8,9.9,-1.7));
#62609=CARTESIAN_POINT('',(-7.8,9.6,-2.));
#62610=CARTESIAN_POINT('',(-7.8,9.9,-1.7));
#62611=CARTESIAN_POINT('',(-7.5,9.6,-1.7));
#62612=CARTESIAN_POINT('',(-7.5,9.6,-1.7));
#62613=CARTESIAN_POINT('',(-7.8,9.6,-2.));
#62614=CARTESIAN_POINT('Origin',(-7.65,9.75,0.));
#62615=CARTESIAN_POINT('',(-7.5,9.6,0.));
#62616=CARTESIAN_POINT('',(-7.8,9.9,0.));
#62617=CARTESIAN_POINT('Origin',(-11.2,-9.9,1.7));
#62618=CARTESIAN_POINT('',(-11.5,-9.6,1.7));
#62619=CARTESIAN_POINT('',(-11.2,-9.6,2.));
#62620=CARTESIAN_POINT('',(-11.5,-9.6,1.7));
#62621=CARTESIAN_POINT('',(-11.2,-9.9,1.7));
#62622=CARTESIAN_POINT('',(-11.2,-9.9,1.7));
#62623=CARTESIAN_POINT('',(-11.2,-9.6,2.));
#62624=CARTESIAN_POINT('Origin',(-7.8,-9.9,-1.7));
#62625=CARTESIAN_POINT('',(-7.5,-9.6,-1.7));
#62626=CARTESIAN_POINT('',(-7.8,-9.6,-2.));
#62627=CARTESIAN_POINT('',(-7.5,-9.6,-1.7));
#62628=CARTESIAN_POINT('',(-7.8,-9.9,-1.7));
#62629=CARTESIAN_POINT('',(-7.8,-9.9,-1.7));
#62630=CARTESIAN_POINT('',(-7.8,-9.6,-2.));
#62631=CARTESIAN_POINT('Origin',(-7.65,-9.75,0.));
#62632=CARTESIAN_POINT('',(-7.8,-9.9,0.));
#62633=CARTESIAN_POINT('',(-7.5,-9.6,0.));
#62634=CARTESIAN_POINT('Origin',(-11.2,9.9,-1.7));
#62635=CARTESIAN_POINT('',(-11.5,9.6,-1.7));
#62636=CARTESIAN_POINT('',(-11.2,9.6,-2.));
#62637=CARTESIAN_POINT('',(-11.5,9.6,-1.7));
#62638=CARTESIAN_POINT('',(-11.2,9.9,-1.7));
#62639=CARTESIAN_POINT('',(-11.2,9.9,-1.7));
#62640=CARTESIAN_POINT('',(-11.2,9.6,-2.));
#62641=CARTESIAN_POINT('Origin',(-11.35,9.75,0.));
#62642=CARTESIAN_POINT('',(-11.5,9.6,0.));
#62643=CARTESIAN_POINT('',(-11.2,9.9,0.));
#62644=CARTESIAN_POINT('Origin',(-8.5,9.75,-1.85));
#62645=CARTESIAN_POINT('',(-8.5,9.6,-2.));
#62646=CARTESIAN_POINT('',(-8.5,9.9,-1.7));
#62647=CARTESIAN_POINT('Origin',(-11.5,-9.6,-1.7));
#62648=CARTESIAN_POINT('',(-11.2,-9.9,-1.7));
#62649=CARTESIAN_POINT('',(-11.2,-9.6,-2.));
#62650=CARTESIAN_POINT('',(-11.2,-9.9,-1.7));
#62651=CARTESIAN_POINT('',(-11.5,-9.6,-1.7));
#62652=CARTESIAN_POINT('',(-11.5,-9.6,-1.7));
#62653=CARTESIAN_POINT('',(-11.2,-9.6,-2.));
#62654=CARTESIAN_POINT('Origin',(-11.35,-9.75,0.));
#62655=CARTESIAN_POINT('',(-11.5,-9.6,0.));
#62656=CARTESIAN_POINT('',(-11.2,-9.9,0.));
#62657=CARTESIAN_POINT('Origin',(-11.35,4.95,-1.85));
#62658=CARTESIAN_POINT('',(-11.2,4.95,-2.));
#62659=CARTESIAN_POINT('',(-11.5,4.95,-1.7));
#62660=CARTESIAN_POINT('Origin',(-10.5,-9.75,-1.85));
#62661=CARTESIAN_POINT('',(-10.5,-9.6,-2.));
#62662=CARTESIAN_POINT('',(-10.5,-9.9,-1.7));
#62663=CARTESIAN_POINT('Origin',(-7.65,-4.95,-1.85));
#62664=CARTESIAN_POINT('',(-7.8,-4.95,-2.));
#62665=CARTESIAN_POINT('',(-7.5,-4.95,-1.7));
#62666=CARTESIAN_POINT('Origin',(-10.5,-9.75,1.85));
#62667=CARTESIAN_POINT('',(-10.5,-9.6,2.));
#62668=CARTESIAN_POINT('',(-10.5,-9.9,1.7));
#62669=CARTESIAN_POINT('Origin',(-11.35,4.95,1.85));
#62670=CARTESIAN_POINT('',(-11.2,4.95,2.));
#62671=CARTESIAN_POINT('',(-11.5,4.95,1.7));
#62672=CARTESIAN_POINT('Origin',(-8.5,9.75,1.85));
#62673=CARTESIAN_POINT('',(-8.5,9.6,2.));
#62674=CARTESIAN_POINT('',(-8.5,9.9,1.7));
#62675=CARTESIAN_POINT('Origin',(-7.65,-4.95,1.85));
#62676=CARTESIAN_POINT('',(-7.8,-4.95,2.));
#62677=CARTESIAN_POINT('',(-7.5,-4.95,1.7));
#62678=CARTESIAN_POINT('Origin',(-7.5,-9.9,0.));
#62679=CARTESIAN_POINT('Origin',(-7.5,9.9,0.));
#62680=CARTESIAN_POINT('Origin',(-9.5,0.,-2.));
#62681=CARTESIAN_POINT('Origin',(-11.5,-9.9,0.));
#62682=CARTESIAN_POINT('Origin',(-11.5,9.9,0.));
#62683=CARTESIAN_POINT('Origin',(-9.5,0.,2.));
#62684=CARTESIAN_POINT('',(0.,0.,0.));
#62685=CARTESIAN_POINT('Ctrl Pts',(-5.40297363237939,11.445432490473,-0.042087482955348));
#62686=CARTESIAN_POINT('Ctrl Pts',(-5.33369696111111,11.4406895414653,1.27598004405306));
#62687=CARTESIAN_POINT('Ctrl Pts',(-5.19521862607164,11.0085774465653,3.79612986924071));
#62688=CARTESIAN_POINT('Ctrl Pts',(-4.91840015088629,8.49992872694836,8.36573269447326));
#62689=CARTESIAN_POINT('Ctrl Pts',(-4.57320339639667,2.77438806679843,11.967805106163));
#62690=CARTESIAN_POINT('Ctrl Pts',(-4.15990469688328,-5.28321395100969,
11.056569093912));
#62691=CARTESIAN_POINT('Ctrl Pts',(-3.747686811287,-10.9955419925911,5.33820880446098));
#62692=CARTESIAN_POINT('Ctrl Pts',(-3.33647538038886,-11.8953437286105,
-2.67607624391012));
#62693=CARTESIAN_POINT('Ctrl Pts',(-2.92629230091383,-7.61357058494829,
-9.48509907357355));
#62694=CARTESIAN_POINT('Ctrl Pts',(-2.51711411539744,-0.0352081461009456,
-12.133141923791));
#62695=CARTESIAN_POINT('Ctrl Pts',(-2.12405346851776,7.23325257089384,-9.58201967934875));
#62696=CARTESIAN_POINT('Ctrl Pts',(-1.74697035839629,11.3507348234515,-3.53593739186965));
#62697=CARTESIAN_POINT('Ctrl Pts',(-1.44594495704173,11.3410956049915,2.29151330201399));
#62698=CARTESIAN_POINT('Ctrl Pts',(-1.23555813837642,9.62414272926665,5.84190263222694));
#62699=CARTESIAN_POINT('Ctrl Pts',(-1.11543119956109,8.23345778533256,7.58643680207061));
#62700=CARTESIAN_POINT('Ctrl Pts',(-0.965350761047819,6.18988758696103,
9.48427609552777));
#62701=CARTESIAN_POINT('Ctrl Pts',(-0.755455752947343,2.59800826091561,
11.2146857757666));
#62702=CARTESIAN_POINT('Ctrl Pts',(-0.486005297879084,-2.52226170629262,
11.2131697972667));
#62703=CARTESIAN_POINT('Ctrl Pts',(-0.216964169512981,-7.12771226807027,
8.99614845847778));
#62704=CARTESIAN_POINT('Ctrl Pts',(0.051673199605982,-10.3093017586739,
5.0037967419436));
#62705=CARTESIAN_POINT('Ctrl Pts',(0.319912004204202,-11.4424452984132,
0.0352862821531482));
#62706=CARTESIAN_POINT('Ctrl Pts',(0.587759827560524,-10.3093945561263,
-4.92692882386994));
#62707=CARTESIAN_POINT('Ctrl Pts',(0.810644510337,-7.66768866486485,-8.23632315062337));
#62708=CARTESIAN_POINT('Ctrl Pts',(0.9887628738834,-4.85431418623128,-10.0009017448057));
#62709=CARTESIAN_POINT('Ctrl Pts',(1.16675569936477,-1.72248496421437,-11.0992889627176));
#62710=CARTESIAN_POINT('Ctrl Pts',(1.38901397173341,2.49959534000996,-11.0999021750131));
#62711=CARTESIAN_POINT('Ctrl Pts',(1.65535913685916,7.06073570919373,-8.90264472811187));
#62712=CARTESIAN_POINT('Ctrl Pts',(1.92134523430893,10.2082911979719,-4.95142581114747));
#62713=CARTESIAN_POINT('Ctrl Pts',(2.21649491340346,11.464268710378,0.517623581655109));
#62714=CARTESIAN_POINT('Ctrl Pts',(2.54067136572795,9.61231028484355,6.51924754582076));
#62715=CARTESIAN_POINT('Ctrl Pts',(2.89372530199723,4.26040343756882,10.7809878391944));
#62716=CARTESIAN_POINT('Ctrl Pts',(3.24620579430313,-2.5499807271206,11.2895594263092));
#62717=CARTESIAN_POINT('Ctrl Pts',(3.59813519099429,-8.45086172951072,7.88046583695986));
#62718=CARTESIAN_POINT('Ctrl Pts',(3.94952923360969,-11.4105207073045,1.7432987177926));
#62719=CARTESIAN_POINT('Ctrl Pts',(4.24193167813174,-10.5600221745821,-3.85384587814088));
#62720=CARTESIAN_POINT('Ctrl Pts',(4.53402805814432,-7.47314001623606,-8.38031426693708));
#62721=CARTESIAN_POINT('Ctrl Pts',(4.79664370266186,-3.07363708606063,-10.9230350253262));
#62722=CARTESIAN_POINT('Ctrl Pts',(5.08810557752102,2.47013445948664,-10.9134823314909));
#62723=CARTESIAN_POINT('Ctrl Pts',(5.35017440554513,6.95492422204958,-8.75633618182547));
#62724=CARTESIAN_POINT('Ctrl Pts',(5.61200361956877,10.0542035018942,-4.86537952153394));
#62725=CARTESIAN_POINT('Ctrl Pts',(5.91720482332597,11.3540414258911,0.789064544875747));
#62726=CARTESIAN_POINT('Ctrl Pts',(6.26564105547289,9.10553979339257,7.23636750926088));
#62727=CARTESIAN_POINT('Ctrl Pts',(6.65717646488775,2.59867870246558,11.321535036503));
#62728=CARTESIAN_POINT('Ctrl Pts',(7.04828730943666,-5.02094595929096,10.4607994583915));
#62729=CARTESIAN_POINT('Ctrl Pts',(7.43900933211819,-10.4395500322981,5.04208746732736));
#62730=CARTESIAN_POINT('Ctrl Pts',(7.82938055234697,-11.2946782793107,-2.56617594127693));
#62731=CARTESIAN_POINT('Ctrl Pts',(8.21943575999143,-7.22551638204153,-9.04156914965989));
#62732=CARTESIAN_POINT('Ctrl Pts',(8.60921106212656,-0.0075686889805855,
-11.5674090717167));
#62733=CARTESIAN_POINT('Ctrl Pts',(8.93382080129404,5.99528673196386,-9.45936192902959));
#62734=CARTESIAN_POINT('Ctrl Pts',(9.19340748731854,9.23614030177817,-5.81293639312917));
#62735=CARTESIAN_POINT('Ctrl Pts',(9.45293101808351,11.1142702697208,-1.3107448337562));
#62736=CARTESIAN_POINT('Ctrl Pts',(9.77723136794952,10.4154952826205,5.00401083523754));
#62737=CARTESIAN_POINT('Ctrl Pts',(10.1662605952158,5.00921490063267,10.4044353775234));
#62738=CARTESIAN_POINT('Ctrl Pts',(10.5119839322498,-1.72077939907436,11.154116840079));
#62739=CARTESIAN_POINT('Ctrl Pts',(10.8144567422258,-6.89887898300864,8.65022675987097));
#62740=CARTESIAN_POINT('Ctrl Pts',(11.0737061869649,-9.97097573622103,4.80256799145211));
#62741=CARTESIAN_POINT('Ctrl Pts',(11.332954454476,-11.0656005972151,-0.0012636146746602));
#62742=CARTESIAN_POINT('Ctrl Pts',(11.592212676988,-9.96981484505854,-4.80333442118138));
#62743=CARTESIAN_POINT('Ctrl Pts',(11.8514921790329,-6.89841951530921,-8.65513848120015));
#62744=CARTESIAN_POINT('Ctrl Pts',(12.1108041978391,-2.45923784927583,-10.7938299796143));
#62745=CARTESIAN_POINT('Ctrl Pts',(12.3701601255276,2.46836208123245,-10.7925664321256));
#62746=CARTESIAN_POINT('Ctrl Pts',(12.6295710107042,6.9094980637413,-8.65413386138286));
#62747=CARTESIAN_POINT('Ctrl Pts',(12.8890481983849,9.98316171476258,-4.8004177652554));
#62748=CARTESIAN_POINT('Ctrl Pts',(13.1486032818335,11.0817124894507,0.00909499825818533));
#62749=CARTESIAN_POINT('Ctrl Pts',(13.4082458776239,9.98216422539828,4.81540788001813));
#62750=CARTESIAN_POINT('Ctrl Pts',(13.7112804745406,6.39794424339377,9.32638055254148));
#62751=CARTESIAN_POINT('Ctrl Pts',(14.0577858522366,-0.00835395432331517,
11.5770141955486));
#62752=CARTESIAN_POINT('Ctrl Pts',(14.4478987172592,-7.23337005489467,9.04881838019601));
#62753=CARTESIAN_POINT('Ctrl Pts',(14.8383177312182,-11.3068424364633,2.56726391915326));
#62754=CARTESIAN_POINT('Ctrl Pts',(15.2291319944184,-10.4497082271469,-5.04888270590908));
#62755=CARTESIAN_POINT('Ctrl Pts',(15.6202557238013,-5.02806227013448,-10.4744930049956));
#62756=CARTESIAN_POINT('Ctrl Pts',(16.0119892870161,2.60831854215743,-11.3347514386656));
#62757=CARTESIAN_POINT('Ctrl Pts',(16.338482088023,8.02442066121112,-7.9277656209221));
#62758=CARTESIAN_POINT('Ctrl Pts',(16.6004710641513,10.3977390912262,-3.60280630418266));
#62759=CARTESIAN_POINT('Ctrl Pts',(16.7309850253063,10.8049718643827,-1.22750855798432));
#62760=CARTESIAN_POINT('Ctrl Pts',(16.796746560446,10.8094741535653,0.0236795036592751));
#62761=CARTESIAN_POINT('Ctrl Pts',(-5.38662443082758,11.6842329202395,-0.042087482955348));
#62762=CARTESIAN_POINT('Ctrl Pts',(-5.31602073284708,11.6793991178476,1.30122823777898));
#62763=CARTESIAN_POINT('Ctrl Pts',(-5.17453105309391,11.2378404310333,3.87611783187972));
#62764=CARTESIAN_POINT('Ctrl Pts',(-4.89207386432173,8.67783202920574,8.53871783783621));
#62765=CARTESIAN_POINT('Ctrl Pts',(-4.53961983973176,2.83264538933516,12.2168195484002));
#62766=CARTESIAN_POINT('Ctrl Pts',(-4.11779670190641,-5.39139693844397,
11.2859525558124));
#62767=CARTESIAN_POINT('Ctrl Pts',(-3.69704974086023,-11.2215827743621,
5.44988936613388));
#62768=CARTESIAN_POINT('Ctrl Pts',(-3.27740459014898,-12.1395545614036,
-2.72889999849327));
#62769=CARTESIAN_POINT('Ctrl Pts',(-2.8588531609028,-7.77040836600443,-9.67639362221006));
#62770=CARTESIAN_POINT('Ctrl Pts',(-2.44139968754143,-0.0388721142853535,
-12.3776586948657));
#62771=CARTESIAN_POINT('Ctrl Pts',(-2.04046215341628,7.3748814694369,-9.77518585108066));
#62772=CARTESIAN_POINT('Ctrl Pts',(-1.65589905289416,11.5736066792837,-3.60919969149015));
#62773=CARTESIAN_POINT('Ctrl Pts',(-1.34897071506894,11.563561957149,2.33231726086283));
#62774=CARTESIAN_POINT('Ctrl Pts',(-1.13450959748022,9.81333086311448,5.9513827672463));
#62775=CARTESIAN_POINT('Ctrl Pts',(-1.01206942024888,8.39587803284931,7.72948090408433));
#62776=CARTESIAN_POINT('Ctrl Pts',(-0.859108571001228,6.31309527913905,
9.66370587564346));
#62777=CARTESIAN_POINT('Ctrl Pts',(-0.645184736392552,2.65240388760526,
11.4271146010615));
#62778=CARTESIAN_POINT('Ctrl Pts',(-0.370635299740237,-2.5645957521349,
11.4254307821442));
#62779=CARTESIAN_POINT('Ctrl Pts',(-0.0965765947892482,-7.25574474773981,
9.16696825093226));
#62780=CARTESIAN_POINT('Ctrl Pts',(0.177029974179721,-10.495940553954,5.10090160620736));
#62781=CARTESIAN_POINT('Ctrl Pts',(0.450155222364603,-11.6494709439128,
0.0420395084777696));
#62782=CARTESIAN_POINT('Ctrl Pts',(0.722812894385383,-10.4960064731164,
-5.00904716447792));
#62783=CARTESIAN_POINT('Ctrl Pts',(0.949649833562332,-7.80748481493112,
-8.37685596577217));
#62784=CARTESIAN_POINT('Ctrl Pts',(1.13086935173756,-4.94518515744457,-10.1720883688267));
#62785=CARTESIAN_POINT('Ctrl Pts',(1.31193547259697,-1.75933863472017,-11.2893824118723));
#62786=CARTESIAN_POINT('Ctrl Pts',(1.53800808648294,2.53496041621199,-11.2898509308499));
#62787=CARTESIAN_POINT('Ctrl Pts',(1.80882928470653,7.17245519023224,-9.0555522803647));
#62788=CARTESIAN_POINT('Ctrl Pts',(2.07920370118388,10.3716655806418,-5.03925894158933));
#62789=CARTESIAN_POINT('Ctrl Pts',(2.37912972697024,11.6476623900761,0.518107830099377));
#62790=CARTESIAN_POINT('Ctrl Pts',(2.7084215266127,9.76615815837076,6.61394631540922));
#62791=CARTESIAN_POINT('Ctrl Pts',(3.06686380982559,4.33246375617594,10.9402548757315));
#62792=CARTESIAN_POINT('Ctrl Pts',(3.42458416068682,-2.57871836910459,11.4557472388598));
#62793=CARTESIAN_POINT('Ctrl Pts',(3.78156882350692,-8.56367510055875,7.99749077041819));
#62794=CARTESIAN_POINT('Ctrl Pts',(4.13779970244094,-11.5633896761636,1.77577652817538));
#62795=CARTESIAN_POINT('Ctrl Pts',(4.43407615107156,-10.7011768584388,-3.8951157658593));
#62796=CARTESIAN_POINT('Ctrl Pts',(4.72991998621853,-7.57473185360497,-8.4794174000976));
#62797=CARTESIAN_POINT('Ctrl Pts',(4.99579563816587,-3.12059647036658,-11.0531492863553));
#62798=CARTESIAN_POINT('Ctrl Pts',(5.29071945165254,2.48877066815634,-11.0432915057983));
#62799=CARTESIAN_POINT('Ctrl Pts',(5.55579786749363,7.02472382683712,-8.86124346251412));
#62800=CARTESIAN_POINT('Ctrl Pts',(5.82051763671242,10.1578631240965,-4.92747349510609));
#62801=CARTESIAN_POINT('Ctrl Pts',(6.12893287481644,11.4710667735206,0.786351846504364));
#62802=CARTESIAN_POINT('Ctrl Pts',(6.48086970009608,9.19948880042808,7.29767185085932));
#62803=CARTESIAN_POINT('Ctrl Pts',(6.876036093994,2.63214136512159,11.4196583755266));
#62804=CARTESIAN_POINT('Ctrl Pts',(7.2704951360562,-5.05206738614446,10.5507066000566));
#62805=CARTESIAN_POINT('Ctrl Pts',(7.664269849656,-10.5119684082973,5.08929931648977));
#62806=CARTESIAN_POINT('Ctrl Pts',(8.05739638782829,-11.3721058534257,-2.5723084615911));
#62807=CARTESIAN_POINT('Ctrl Pts',(8.44991208702215,-7.27666845581022,-9.08750535291988));
#62808=CARTESIAN_POINT('Ctrl Pts',(8.84183589581078,-0.0190233677037744,
-11.6261961433184));
#62809=CARTESIAN_POINT('Ctrl Pts',(9.16800897973602,6.01193267834016,-9.50734087777631));
#62810=CARTESIAN_POINT('Ctrl Pts',(9.42865337465075,9.26567864906491,-5.84611390760456));
#62811=CARTESIAN_POINT('Ctrl Pts',(9.68913010904725,11.1505695545849,-1.32743556288045));
#62812=CARTESIAN_POINT('Ctrl Pts',(10.01444990245,10.4487042298974,5.00670632569537));
#62813=CARTESIAN_POINT('Ctrl Pts',(10.404410400302,5.0292579730303,10.418996824966));
#62814=CARTESIAN_POINT('Ctrl Pts',(10.7506877702216,-1.71103270316429,11.1687624961623));
#62815=CARTESIAN_POINT('Ctrl Pts',(11.0534087660824,-6.89297973807507,8.66266553885666));
#62816=CARTESIAN_POINT('Ctrl Pts',(11.3127577882607,-9.96570753196438,4.81359043978792));
#62817=CARTESIAN_POINT('Ctrl Pts',(11.5719265540532,-11.0597406950972,0.0113000199644781));
#62818=CARTESIAN_POINT('Ctrl Pts',(11.8309999800597,-9.96443740908525,-4.78691623055493));
#62819=CARTESIAN_POINT('Ctrl Pts',(12.089942848211,-6.89699200645375,-8.63338332691425));
#62820=CARTESIAN_POINT('Ctrl Pts',(12.3487984396484,-2.46582258118391,-10.7678176469866));
#62821=CARTESIAN_POINT('Ctrl Pts',(12.6075197618077,2.44956273217333,-10.766340494442));
#62822=CARTESIAN_POINT('Ctrl Pts',(12.8661852362955,6.87753001040116,-8.63389160824295));
#62823=CARTESIAN_POINT('Ctrl Pts',(13.1247741476138,9.94027936125449,-4.79343295279293));
#62824=CARTESIAN_POINT('Ctrl Pts',(13.3833009319311,11.0341713583544,-0.00317416406982458));
#62825=CARTESIAN_POINT('Ctrl Pts',(13.6417781017764,9.93937775359348,4.78122924367456));
#62826=CARTESIAN_POINT('Ctrl Pts',(13.9432825257392,6.3731535080168,9.26905415030222));
#62827=CARTESIAN_POINT('Ctrl Pts',(14.2878439989708,0.00300314958158428,
11.5061588243725));
#62828=CARTESIAN_POINT('Ctrl Pts',(14.6754462417248,-7.17478563786537,8.99342192147372));
#62829=CARTESIAN_POINT('Ctrl Pts',(15.0630597522916,-11.2179471506956,2.55835488475392));
#62830=CARTESIAN_POINT('Ctrl Pts',(15.4507706640767,-10.3667041184257,-4.99673895003962));
#62831=CARTESIAN_POINT('Ctrl Pts',(15.8384977092108,-4.99174936807355,-10.3743665471522));
#62832=CARTESIAN_POINT('Ctrl Pts',(16.2265565504856,2.57263136784385,-11.2253812680671));
#62833=CARTESIAN_POINT('Ctrl Pts',(16.5497447116511,7.93342720259043,-7.8526330852735));
#62834=CARTESIAN_POINT('Ctrl Pts',(16.8089720533906,10.2814647901916,-3.57330742364719));
#62835=CARTESIAN_POINT('Ctrl Pts',(16.9379965316827,10.6841596272025,-1.22522263021414));
#62836=CARTESIAN_POINT('Ctrl Pts',(17.0030907568274,10.6886162297605,0.0132690991824951));
#62837=CARTESIAN_POINT('Ctrl Pts',(-5.58213752804996,12.1756744501656,-0.0300430479348889));
#62838=CARTESIAN_POINT('Ctrl Pts',(-5.50877812904515,12.1706519818174,1.36570302154143));
#62839=CARTESIAN_POINT('Ctrl Pts',(-5.36106226989209,11.7096936310828,4.05389952128246));
#62840=CARTESIAN_POINT('Ctrl Pts',(-5.06685484898808,9.0428635992223,8.91045562475751));
#62841=CARTESIAN_POINT('Ctrl Pts',(-4.69909942041695,2.94563865221725,12.7498701343512));
#62842=CARTESIAN_POINT('Ctrl Pts',(-4.25898293676952,-5.63608587336797,
11.7779719464893));
#62843=CARTESIAN_POINT('Ctrl Pts',(-3.81963203329655,-11.7245092162211,
5.68555235440507));
#62844=CARTESIAN_POINT('Ctrl Pts',(-3.38127989331131,-12.6839981428031,
-2.85852486490255));
#62845=CARTESIAN_POINT('Ctrl Pts',(-2.94385951041784,-8.11849627124418,
-10.1194220241074));
#62846=CARTESIAN_POINT('Ctrl Pts',(-2.50743743147879,-0.0355288229951717,
-12.9441324262393));
#62847=CARTESIAN_POINT('Ctrl Pts',(-2.08814562231316,7.71791821403956,-10.2228628918827));
#62848=CARTESIAN_POINT('Ctrl Pts',(-1.68588713127857,12.1102975092266,-3.77315273387394));
#62849=CARTESIAN_POINT('Ctrl Pts',(-1.36477227087896,12.0999643764455,2.44316120718691));
#62850=CARTESIAN_POINT('Ctrl Pts',(-1.14036484630118,10.2685685552556,6.23014691826401));
#62851=CARTESIAN_POINT('Ctrl Pts',(-1.0122386454203,8.78527999884706,8.09084634428638));
#62852=CARTESIAN_POINT('Ctrl Pts',(-0.85216987072336,6.60570228047088,10.1149895329489));
#62853=CARTESIAN_POINT('Ctrl Pts',(-0.628321429176446,2.77503882988668,
11.9603687960931));
#62854=CARTESIAN_POINT('Ctrl Pts',(-0.341007099925978,-2.68468283670305,
11.9586500930173));
#62855=CARTESIAN_POINT('Ctrl Pts',(-0.0541880283575395,-7.59440137466866,
9.59501436524506));
#62856=CARTESIAN_POINT('Ctrl Pts',(0.232133536516826,-10.9853111743879,
5.33976875825063));
#62857=CARTESIAN_POINT('Ctrl Pts',(0.517951166519818,-12.1925427115221,
0.0456306551254132));
#62858=CARTESIAN_POINT('Ctrl Pts',(0.803260682123494,-10.9854331034987,
-5.24005102588547));
#62859=CARTESIAN_POINT('Ctrl Pts',(1.04059235059325,-8.17236014711802,-8.76383928564432));
#62860=CARTESIAN_POINT('Ctrl Pts',(1.2301999694469,-5.17749816539757,-10.6422030007412));
#62861=CARTESIAN_POINT('Ctrl Pts',(1.41963543254174,-1.84431402112184,-11.8111697640491));
#62862=CARTESIAN_POINT('Ctrl Pts',(1.65610507694268,2.6477367975528,-11.811608800416));
#62863=CARTESIAN_POINT('Ctrl Pts',(1.93934686505911,7.49812591212634,-9.47468373122583));
#62864=CARTESIAN_POINT('Ctrl Pts',(2.22206455148271,10.8434401317323,-5.27473146272307));
#62865=CARTESIAN_POINT('Ctrl Pts',(2.53560960785567,12.1773347135935,0.535301325191032));
#62866=CARTESIAN_POINT('Ctrl Pts',(2.87975460475582,10.2105264526929,6.90643581380321));
#62867=CARTESIAN_POINT('Ctrl Pts',(3.25424270967884,4.53310104469524,11.4261564695298));
#62868=CARTESIAN_POINT('Ctrl Pts',(3.62777977875684,-2.68423523986195,11.9641280503083));
#62869=CARTESIAN_POINT('Ctrl Pts',(4.00036632514192,-8.93103640357327,8.35396714094425));
#62870=CARTESIAN_POINT('Ctrl Pts',(4.37200507590755,-12.0601729625909,1.86268306094367));
#62871=CARTESIAN_POINT('Ctrl Pts',(4.68091022499164,-11.1607102375445,-4.05023454867948));
#62872=CARTESIAN_POINT('Ctrl Pts',(4.98922157892821,-7.90218781464488,-8.82784028522772));
#62873=CARTESIAN_POINT('Ctrl Pts',(5.26616701679252,-3.26213222142188,-11.5085441738385));
#62874=CARTESIAN_POINT('Ctrl Pts',(5.57319492830223,2.57770964828084,-11.4977849322459));
#62875=CARTESIAN_POINT('Ctrl Pts',(5.84898620445269,7.29714668223437,-9.22715804319427));
#62876=CARTESIAN_POINT('Ctrl Pts',(6.12424703583544,10.5549795888417,-5.13618793357213));
#62877=CARTESIAN_POINT('Ctrl Pts',(6.44477147423336,11.9193648706261,0.802433581377994));
#62878=CARTESIAN_POINT('Ctrl Pts',(6.810201779699,9.55929334082063,7.56370607387037));
#62879=CARTESIAN_POINT('Ctrl Pts',(7.22014147482059,2.74520255759924,11.8389419876145));
#62880=CARTESIAN_POINT('Ctrl Pts',(7.62891578995641,-5.21837344535205,10.9369214780428));
#62881=CARTESIAN_POINT('Ctrl Pts',(8.0365379096552,-10.8696746733105,5.28195384018169));
#62882=CARTESIAN_POINT('Ctrl Pts',(8.44302223705143,-11.7575201639929,-2.64075235344257));
#62883=CARTESIAN_POINT('Ctrl Pts',(8.84838123656028,-7.52639107092263,-9.36895084697553));
#62884=CARTESIAN_POINT('Ctrl Pts',(9.25263526251976,-0.0392759205799279,
-11.9860267493518));
#62885=CARTESIAN_POINT('Ctrl Pts',(9.58859730899462,6.17283522387099,-9.80208377905409));
#62886=CARTESIAN_POINT('Ctrl Pts',(9.85684366241965,9.52142304101027,-6.03375708408332));
#62887=CARTESIAN_POINT('Ctrl Pts',(10.1247368478916,11.4597337643269,-1.38603993283289));
#62888=CARTESIAN_POINT('Ctrl Pts',(10.4589411719737,10.7372829702099,5.121580228287));
#62889=CARTESIAN_POINT('Ctrl Pts',(10.8589525646346,5.17601081871361,10.672306219655));
#62890=CARTESIAN_POINT('Ctrl Pts',(11.2136246222839,-1.72855590679122,11.4388774467827));
#62891=CARTESIAN_POINT('Ctrl Pts',(11.5233392509183,-7.03015404855583,8.87404791214989));
#62892=CARTESIAN_POINT('Ctrl Pts',(11.7883721374067,-10.1702418575688,4.93991879033325));
#62893=CARTESIAN_POINT('Ctrl Pts',(12.0529994415247,-11.2866773983137,0.0361816243266041));
#62894=CARTESIAN_POINT('Ctrl Pts',(12.3172031678835,-10.1691224548695,-4.85742315527652));
#62895=CARTESIAN_POINT('Ctrl Pts',(12.5810085730965,-7.04333516732229,-8.77595778561382));
#62896=CARTESIAN_POINT('Ctrl Pts',(12.8444122722771,-2.53358181596827,-10.9476579632121));
#62897=CARTESIAN_POINT('Ctrl Pts',(13.1074454062801,2.46392456498872,-10.9454322140739));
#62898=CARTESIAN_POINT('Ctrl Pts',(13.3700914250086,6.96015352944818,-8.77946190588175));
#62899=CARTESIAN_POINT('Ctrl Pts',(13.6323722416537,10.0663826285115,-4.88343493856922));
#62900=CARTESIAN_POINT('Ctrl Pts',(13.894296945586,11.1740422712744,-0.0296971803831297));
#62901=CARTESIAN_POINT('Ctrl Pts',(14.1558727999502,10.0654107461421,4.81229139485823));
#62902=CARTESIAN_POINT('Ctrl Pts',(14.4606573163972,6.45944618588964,9.34875999480817));
#62903=CARTESIAN_POINT('Ctrl Pts',(14.8084186207746,0.0286940154300198,
11.6049438878024));
#62904=CARTESIAN_POINT('Ctrl Pts',(15.1989659292178,-7.20343837095942,9.0707366164502));
#62905=CARTESIAN_POINT('Ctrl Pts',(15.5888271044371,-11.2684315837746,2.59648807102487));
#62906=CARTESIAN_POINT('Ctrl Pts',(15.9781003660338,-10.4114044148879,-4.98937302790091));
#62907=CARTESIAN_POINT('Ctrl Pts',(16.3666890068541,-5.02240875860095,-10.3778490907909));
#62908=CARTESIAN_POINT('Ctrl Pts',(16.75491996291,2.54609586936617,-11.2269852191641));
#62909=CARTESIAN_POINT('Ctrl Pts',(17.0776472449118,7.8986520888767,-7.8571397173543));
#62910=CARTESIAN_POINT('Ctrl Pts',(17.3361860886226,10.2399861777324,-3.5889008967425));
#62911=CARTESIAN_POINT('Ctrl Pts',(17.4647378405461,10.6409669797038,-1.24921590933198));
#62912=CARTESIAN_POINT('Ctrl Pts',(17.5296467076155,10.6454108919306,-0.0142508283097832));
#62913=CARTESIAN_POINT('Ctrl Pts',(-6.34175946120379,12.4040821855152,0.0107040337528743));
#62914=CARTESIAN_POINT('Ctrl Pts',(-6.26706179117867,12.398968093954,1.43191223271551));
#62915=CARTESIAN_POINT('Ctrl Pts',(-6.11635370620616,11.9288069117454,4.17463339171532));
#62916=CARTESIAN_POINT('Ctrl Pts',(-5.81628679876286,9.2092221886427,9.12810114140272));
#62917=CARTESIAN_POINT('Ctrl Pts',(-5.44029591289839,2.97759289791273,13.0564360914058));
#62918=CARTESIAN_POINT('Ctrl Pts',(-4.98949435753561,-5.81353510375367,
12.0632665775625));
#62919=CARTESIAN_POINT('Ctrl Pts',(-4.53841730021845,-12.0667921857124,
5.81108553319272));
#62920=CARTESIAN_POINT('Ctrl Pts',(-4.08742934584185,-13.057041864785,-2.97951654626261));
#62921=CARTESIAN_POINT('Ctrl Pts',(-3.63642773955957,-8.35245308061332,
-10.4675245804829));
#62922=CARTESIAN_POINT('Ctrl Pts',(-3.18552048891545,-0.00195865738740459,
-13.3890796953648));
#62923=CARTESIAN_POINT('Ctrl Pts',(-2.751417959208,8.0264806856427,-10.5743146210541));
#62924=CARTESIAN_POINT('Ctrl Pts',(-2.33416003624442,12.5846595571708,-3.88522073955045));
#62925=CARTESIAN_POINT('Ctrl Pts',(-2.00048088021236,12.5755296487166,2.57451200864791));
#62926=CARTESIAN_POINT('Ctrl Pts',(-1.76698407230375,10.670190652471,6.51510179427282));
#62927=CARTESIAN_POINT('Ctrl Pts',(-1.63358171760574,9.12583521912976,8.45245139042781));
#62928=CARTESIAN_POINT('Ctrl Pts',(-1.46685019792153,6.85557171288117,10.560894186678));
#62929=CARTESIAN_POINT('Ctrl Pts',(-1.2335005384759,2.86250938720469,12.4851894756634));
#62930=CARTESIAN_POINT('Ctrl Pts',(-0.933608830224655,-2.83629378794764,
12.484184502557));
#62931=CARTESIAN_POINT('Ctrl Pts',(-0.633859801053286,-7.96772149200299,
10.0146740366583));
#62932=CARTESIAN_POINT('Ctrl Pts',(-0.334278396183705,-11.5163113708967,
5.56273552772346));
#62933=CARTESIAN_POINT('Ctrl Pts',(-0.0348645255961784,-12.7817158623768,
0.0168674356443003));
#62934=CARTESIAN_POINT('Ctrl Pts',(0.264362813841201,-11.5163950507525,
-5.5269006446327));
#62935=CARTESIAN_POINT('Ctrl Pts',(0.513553405915242,-8.5631641849765,-9.22718654740676));
#62936=CARTESIAN_POINT('Ctrl Pts',(0.712806926101561,-5.41596454340597,
-11.2012236785028));
#62937=CARTESIAN_POINT('Ctrl Pts',(0.911989524646343,-1.91131413349739,
-12.4304453184779));
#62938=CARTESIAN_POINT('Ctrl Pts',(1.16082303907062,2.81564799024151,-12.4314570114187));
#62939=CARTESIAN_POINT('Ctrl Pts',(1.459193817749,7.92546878244216,-9.9702951678761));
#62940=CARTESIAN_POINT('Ctrl Pts',(1.7573216234739,11.4536360269907,-5.54174799395099));
#62941=CARTESIAN_POINT('Ctrl Pts',(2.08829138644019,12.8623669859745,0.590980361928457));
#62942=CARTESIAN_POINT('Ctrl Pts',(2.45197695065466,10.785129106603,7.32433413314867));
#62943=CARTESIAN_POINT('Ctrl Pts',(2.84823026768593,4.77857709686782,12.1078614071571));
#62944=CARTESIAN_POINT('Ctrl Pts',(3.24395222388046,-2.86735584763152,12.6791154950883));
#62945=CARTESIAN_POINT('Ctrl Pts',(3.63912043631913,-9.49342202523412,8.85119319113865));
#62946=CARTESIAN_POINT('Ctrl Pts',(4.0337213999701,-12.8170179970068,1.95940039112546));
#62947=CARTESIAN_POINT('Ctrl Pts',(4.36205345736307,-11.8618890483679,-4.32554789162836));
#62948=CARTESIAN_POINT('Ctrl Pts',(4.68999551311996,-8.3960872137632,-9.40751712592762));
#62949=CARTESIAN_POINT('Ctrl Pts',(4.98478752120831,-3.45741751832818,-12.2615793993256));
#62950=CARTESIAN_POINT('Ctrl Pts',(5.31185556491466,2.76363202170254,-12.2506035050116));
#62951=CARTESIAN_POINT('Ctrl Pts',(5.60583527334105,7.79447342695731,-9.83054973508101));
#62952=CARTESIAN_POINT('Ctrl Pts',(5.89942807060424,11.2695311402808,-5.46736710999676));
#62953=CARTESIAN_POINT('Ctrl Pts',(6.24149197480825,12.7260002736351,0.870188005253589));
#62954=CARTESIAN_POINT('Ctrl Pts',(6.63174332507484,10.2065394057231,8.09093665967303));
#62955=CARTESIAN_POINT('Ctrl Pts',(7.06983734038559,2.92500698185025,12.6606037658675));
#62956=CARTESIAN_POINT('Ctrl Pts',(7.50696568218765,-5.59098643250971,11.6968630723186));
#62957=CARTESIAN_POINT('Ctrl Pts',(7.94310322458065,-11.6380802493207,5.64685644540905));
#62958=CARTESIAN_POINT('Ctrl Pts',(8.37822412215387,-12.5890445132526,-2.83387178302892));
#62959=CARTESIAN_POINT('Ctrl Pts',(8.81230632819328,-8.05854610358395,-10.0389570413963));
#62960=CARTESIAN_POINT('Ctrl Pts',(9.24532947911908,-0.038785248132775,
-12.842590638725));
#62961=CARTESIAN_POINT('Ctrl Pts',(9.60528130639712,6.61682954666117,-10.502876810536));
#62962=CARTESIAN_POINT('Ctrl Pts',(9.89269473817186,10.2046562682575,-6.46531635211994));
#62963=CARTESIAN_POINT('Ctrl Pts',(10.1797394837133,12.2815441775112,-1.48538330475788));
#62964=CARTESIAN_POINT('Ctrl Pts',(10.5378474556428,11.5073725540162,5.48755966310341));
#62965=CARTESIAN_POINT('Ctrl Pts',(10.9664455129648,5.54866596836936,11.4347559671639));
#62966=CARTESIAN_POINT('Ctrl Pts',(11.3464036646752,-1.84798660091247,12.2556102432363));
#62967=CARTESIAN_POINT('Ctrl Pts',(11.6781166939346,-7.52600746857995,9.50851847857713));
#62968=CARTESIAN_POINT('Ctrl Pts',(11.9619245164408,-10.8882955584731,5.29569253526718));
#62969=CARTESIAN_POINT('Ctrl Pts',(12.2452108460461,-12.0832976277723,0.0461979593358211));
#62970=CARTESIAN_POINT('Ctrl Pts',(12.5279739899067,-10.8870335306923,-5.19097370078296));
#62971=CARTESIAN_POINT('Ctrl Pts',(12.8102105391723,-7.54275874293532,-9.38308321473704));
#62972=CARTESIAN_POINT('Ctrl Pts',(13.0919194206535,-2.71962628545003,-11.7053766605458));
#62973=CARTESIAN_POINT('Ctrl Pts',(13.3730967409146,2.62254510442751,-11.7027590086165));
#62974=CARTESIAN_POINT('Ctrl Pts',(13.6537434878202,7.42666913824623,-9.38811573361164));
#62975=CARTESIAN_POINT('Ctrl Pts',(13.9338570502649,10.7437663434859,-5.22710379048192));
#62976=CARTESIAN_POINT('Ctrl Pts',(14.2134367039418,11.9257320683964,-0.0462399805677666));
#62977=CARTESIAN_POINT('Ctrl Pts',(14.4924819112214,10.7427611087893,5.11889347639459));
#62978=CARTESIAN_POINT('Ctrl Pts',(14.8174102629407,6.89814482154727,9.95484178310012));
#62979=CARTESIAN_POINT('Ctrl Pts',(15.1878675784235,0.0475887665098514,
12.3570599665712));
#62980=CARTESIAN_POINT('Ctrl Pts',(15.60343011016,-7.64719333189951,9.658942786652));
#62981=CARTESIAN_POINT('Ctrl Pts',(16.0177919854228,-11.9658388446688,2.77756371508464));
#62982=CARTESIAN_POINT('Ctrl Pts',(16.4309653348316,-11.0545902282553,-5.27451592744702));
#62983=CARTESIAN_POINT('Ctrl Pts',(16.8429380715054,-5.34037028988571,-10.9839370189219));
#62984=CARTESIAN_POINT('Ctrl Pts',(17.2537589451344,2.66970311374553,-11.8825373324373));
#62985=CARTESIAN_POINT('Ctrl Pts',(17.5950843011881,8.3276981377702,-8.31584017070621));
#62986=CARTESIAN_POINT('Ctrl Pts',(17.8676474164505,10.7963199255675,-3.81611675463074));
#62987=CARTESIAN_POINT('Ctrl Pts',(18.0035957502116,11.2204164513183,-1.34196072369696));
#62988=CARTESIAN_POINT('Ctrl Pts',(18.0717719751097,11.2250840595062,-0.0448304407862714));
#62989=CARTESIAN_POINT('Ctrl Pts',(-6.99577676753807,11.952974211143,0.0434554360374288));
#62990=CARTESIAN_POINT('Ctrl Pts',(-6.92354819783309,11.9480291637448,1.41768619088611));
#62991=CARTESIAN_POINT('Ctrl Pts',(-6.7784296219674,11.4953034355832,4.0586609902612));
#62992=CARTESIAN_POINT('Ctrl Pts',(-6.48867577802364,8.87010370902588,8.84204422931722));
#62993=CARTESIAN_POINT('Ctrl Pts',(-6.12530330932051,2.84823660147519,12.6398835273164));
#62994=CARTESIAN_POINT('Ctrl Pts',(-5.68857922216732,-5.6680044099001,11.6816959347463));
#62995=CARTESIAN_POINT('Ctrl Pts',(-5.25073555922688,-11.7399831228001,
5.61456522614908));
#62996=CARTESIAN_POINT('Ctrl Pts',(-4.81200855085364,-12.7064619153397,
-2.93611368688326));
#62997=CARTESIAN_POINT('Ctrl Pts',(-4.37232938788964,-8.12271966538111,
-10.2377880044934));
#62998=CARTESIAN_POINT('Ctrl Pts',(-3.93176827936533,0.0348328210943832,
-13.0952412158728));
#62999=CARTESIAN_POINT('Ctrl Pts',(-3.50668474008689,7.89732345693862,-10.3419323625203));
#63000=CARTESIAN_POINT('Ctrl Pts',(-3.09722403722738,12.3722191925458,-3.7793768466969));
#63001=CARTESIAN_POINT('Ctrl Pts',(-2.76912452694493,12.3650890133529,2.57226891368155));
#63002=CARTESIAN_POINT('Ctrl Pts',(-2.53919306504922,10.4891472653307,6.45285596073122));
#63003=CARTESIAN_POINT('Ctrl Pts',(-2.40772900615144,8.96727281566909,8.36205471574902));
#63004=CARTESIAN_POINT('Ctrl Pts',(-2.2433365747859,6.72892811627392,10.4409303885383));
#63005=CARTESIAN_POINT('Ctrl Pts',(-2.01300451361892,2.78796532718832,12.340912648531));
#63006=CARTESIAN_POINT('Ctrl Pts',(-1.71654890422905,-2.84542392262709,
12.3409008152921));
#63007=CARTESIAN_POINT('Ctrl Pts',(-1.41978813824793,-7.92600416136757,
9.89691654580502));
#63008=CARTESIAN_POINT('Ctrl Pts',(-1.12271904140829,-11.4455308662374,
5.48309264597084));
#63009=CARTESIAN_POINT('Ctrl Pts',(-0.825363517227147,-12.7031226545021,
-0.0243048795543868));
#63010=CARTESIAN_POINT('Ctrl Pts',(-0.527731514558294,-11.4455893823448,
-5.53859048082785));
#63011=CARTESIAN_POINT('Ctrl Pts',(-0.279478005503598,-8.50418660255496,
-9.22536834241496));
#63012=CARTESIAN_POINT('Ctrl Pts',(-0.0807549704906864,-5.36547510445352,
-11.1942782947732));
#63013=CARTESIAN_POINT('Ctrl Pts',(0.118051755945107,-1.8675651818906,-12.4213082475664));
#63014=CARTESIAN_POINT('Ctrl Pts',(0.366722102791505,2.85612569879392,-12.4231343878714));
#63015=CARTESIAN_POINT('Ctrl Pts',(0.665352877801153,7.97071605146552,-9.96078604555384));
#63016=CARTESIAN_POINT('Ctrl Pts',(0.964206395126258,11.5081607160169,-5.52218356455426));
#63017=CARTESIAN_POINT('Ctrl Pts',(1.29649977104871,12.9235881289301,0.634564968811868));
#63018=CARTESIAN_POINT('Ctrl Pts',(1.66230004176491,10.8364263379226,7.40750400995353));
#63019=CARTESIAN_POINT('Ctrl Pts',(2.06167174932048,4.78420119573235,12.230536232645));
#63020=CARTESIAN_POINT('Ctrl Pts',(2.4613476543818,-2.93770395852455,12.8098037984882));
#63021=CARTESIAN_POINT('Ctrl Pts',(2.86128398965418,-9.64464038610263,8.93787022257689));
#63022=CARTESIAN_POINT('Ctrl Pts',(3.26144748282469,-13.0171740913694,1.95011291304442));
#63023=CARTESIAN_POINT('Ctrl Pts',(3.59508775314631,-12.0484781972671,-4.43660651624035));
#63024=CARTESIAN_POINT('Ctrl Pts',(3.92883523912539,-8.52186871803321,-9.60879315096172));
#63025=CARTESIAN_POINT('Ctrl Pts',(4.22929904502273,-3.48912056106834,-12.5190732399397));
#63026=CARTESIAN_POINT('Ctrl Pts',(4.56323741679503,2.86256934376227,-12.5090759805677));
#63027=CARTESIAN_POINT('Ctrl Pts',(4.86384381459426,8.00709959101652,-10.0353408515575));
#63028=CARTESIAN_POINT('Ctrl Pts',(5.16449854937864,11.5664022511167,-5.56793348942886));
#63029=CARTESIAN_POINT('Ctrl Pts',(5.51529547561481,13.0611497278196,0.930947571039876));
#63030=CARTESIAN_POINT('Ctrl Pts',(5.91625229346491,10.4753825672146,8.35038622910933));
#63031=CARTESIAN_POINT('Ctrl Pts',(6.36731990925114,2.98011034179285,13.0580379108325));
#63032=CARTESIAN_POINT('Ctrl Pts',(6.81834949067038,-5.80685122812227,12.0668130502114));
#63033=CARTESIAN_POINT('Ctrl Pts',(7.26929377330161,-12.0612898991556,5.81375475793947));
#63034=CARTESIAN_POINT('Ctrl Pts',(7.72010735706853,-13.0495675260762,-2.97232521957111));
#63035=CARTESIAN_POINT('Ctrl Pts',(8.17075036739142,-8.34884614818407,-10.4536677858431));
#63036=CARTESIAN_POINT('Ctrl Pts',(8.62117589579843,-0.00791391267151051,
-13.3727411912355));
#63037=CARTESIAN_POINT('Ctrl Pts',(8.99632517267344,6.92934274946376,-10.936465798048));
#63038=CARTESIAN_POINT('Ctrl Pts',(9.29628043819794,10.6740986744864,-6.72296849065872));
#63039=CARTESIAN_POINT('Ctrl Pts',(9.59612919106517,12.8440088694065,-1.52123511579387));
#63040=CARTESIAN_POINT('Ctrl Pts',(9.97073190268916,12.0363481832331,5.77286443669366));
#63041=CARTESIAN_POINT('Ctrl Pts',(10.4198783301282,5.79407206251631,12.0070815806333));
#63042=CARTESIAN_POINT('Ctrl Pts',(10.8187411384565,-1.97027233311315,12.8708724365812));
#63043=CARTESIAN_POINT('Ctrl Pts',(11.1674340824346,-7.93932119118973,9.98396585791531));
#63044=CARTESIAN_POINT('Ctrl Pts',(11.4661029846676,-11.4780906888311,5.55105116774377));
#63045=CARTESIAN_POINT('Ctrl Pts',(11.7645290272056,-12.7376376654062,0.0211894625936921));
#63046=CARTESIAN_POINT('Ctrl Pts',(12.0627229130648,-11.4767297176299,-5.50183090606377));
#63047=CARTESIAN_POINT('Ctrl Pts',(12.3606592012589,-7.94698392227365,-9.92748510239363));
#63048=CARTESIAN_POINT('Ctrl Pts',(12.6583360267427,-2.8508280855602,-12.3819217266038));
#63049=CARTESIAN_POINT('Ctrl Pts',(12.9557247677888,2.79931904143353,-12.379773222104));
#63050=CARTESIAN_POINT('Ctrl Pts',(13.2528343635669,7.88544101719467,-9.92990805014466));
#63051=CARTESIAN_POINT('Ctrl Pts',(13.549644270199,11.4006534463597,-5.52129050887731));
#63052=CARTESIAN_POINT('Ctrl Pts',(13.8461441282306,12.6546960389499,-0.0270590683343575));
#63053=CARTESIAN_POINT('Ctrl Pts',(14.142325486993,11.3995925558707,5.45532204259041));
#63054=CARTESIAN_POINT('Ctrl Pts',(14.4874806409761,7.31619812550857,10.5926204476333));
#63055=CARTESIAN_POINT('Ctrl Pts',(14.8813899261482,0.0326555994906588,
13.1482752638617));
#63056=CARTESIAN_POINT('Ctrl Pts',(15.3237262854681,-8.15850127667032,10.2777019802623));
#63057=CARTESIAN_POINT('Ctrl Pts',(15.7652478499986,-12.7611663516314,2.94651360079951));
#63058=CARTESIAN_POINT('Ctrl Pts',(16.2058751260915,-11.7908725563387,-5.6416476886062));
#63059=CARTESIAN_POINT('Ctrl Pts',(16.6456846506483,-5.69172965589703,-11.7358279093178));
#63060=CARTESIAN_POINT('Ctrl Pts',(17.084418208847,2.86369100930359,-12.6988551400737));
#63061=CARTESIAN_POINT('Ctrl Pts',(17.4495345059912,8.91441846626095,-8.88278736054426));
#63062=CARTESIAN_POINT('Ctrl Pts',(17.7406676458964,11.5522099350677,-4.07665772399991));
#63063=CARTESIAN_POINT('Ctrl Pts',(17.8865302419488,12.0072646015869,-1.42218653131724));
#63064=CARTESIAN_POINT('Ctrl Pts',(17.9590854976129,12.0122320151672,-0.0417402034811674));
#63065=CARTESIAN_POINT('Ctrl Pts',(-7.04836243219494,11.1602873706909,0.0433668871147811));
#63066=CARTESIAN_POINT('Ctrl Pts',(-6.98054923009834,11.1556446164462,1.33359024729692));
#63067=CARTESIAN_POINT('Ctrl Pts',(-6.84542083169465,10.734108144334,3.79280974414481));
#63068=CARTESIAN_POINT('Ctrl Pts',(-6.57440587453761,8.27955737620748,8.26700195680993));
#63069=CARTESIAN_POINT('Ctrl Pts',(-6.23509541011525,2.6547559310062,11.8124549780299));
#63070=CARTESIAN_POINT('Ctrl Pts',(-5.82667850202676,-5.30836037069009,
10.9193453075009));
#63071=CARTESIAN_POINT('Ctrl Pts',(-5.41714811934068,-10.9886329727755,
5.24339954566476));
#63072=CARTESIAN_POINT('Ctrl Pts',(-5.00642724205123,-11.8945997983615,
-2.76045718501004));
#63073=CARTESIAN_POINT('Ctrl Pts',(-4.5945364954459,-7.60126338096456,-9.60168441536687));
#63074=CARTESIAN_POINT('Ctrl Pts',(-4.18145490797301,0.0469804373507585,
-12.2819941081016));
#63075=CARTESIAN_POINT('Ctrl Pts',(-3.78252541805809,7.42629200691454,-9.69929592859116));
#63076=CARTESIAN_POINT('Ctrl Pts',(-3.39789099794522,11.6308417690081,-3.53519632822153));
#63077=CARTESIAN_POINT('Ctrl Pts',(-3.08939324254413,11.6250000259672,2.43710008693653));
#63078=CARTESIAN_POINT('Ctrl Pts',(-2.87302899057922,9.85989537087712,6.08882885264012));
#63079=CARTESIAN_POINT('Ctrl Pts',(-2.74927343717844,8.42726546917283,7.88610073971078));
#63080=CARTESIAN_POINT('Ctrl Pts',(-2.5944799794377,6.3196412110271,9.84362143917224));
#63081=CARTESIAN_POINT('Ctrl Pts',(-2.37749287855617,2.60710207818047,11.6339173336133));
#63082=CARTESIAN_POINT('Ctrl Pts',(-2.09797454340211,-2.70450448853709,
11.6344255830779));
#63083=CARTESIAN_POINT('Ctrl Pts',(-1.81792170554395,-7.49931778606355,
9.32850799058278));
#63084=CARTESIAN_POINT('Ctrl Pts',(-1.53733736459604,-10.8240376978191,
5.15986381030307));
#63085=CARTESIAN_POINT('Ctrl Pts',(-1.2562206918343,-12.0135545707024,-0.0467397984840756));
#63086=CARTESIAN_POINT('Ctrl Pts',(-0.974573862808477,-10.8241045261154,
-5.26507248654322));
#63087=CARTESIAN_POINT('Ctrl Pts',(-0.739428880773772,-8.03834277864345,
-8.7575825674062));
#63088=CARTESIAN_POINT('Ctrl Pts',(-0.551047584316217,-5.0629822009722,
-10.6241459120783));
#63089=CARTESIAN_POINT('Ctrl Pts',(-0.36249111019426,-1.74543644090898,
-11.7880199128214));
#63090=CARTESIAN_POINT('Ctrl Pts',(-0.126471246010493,2.73805411019759,
-11.7902852668568));
#63091=CARTESIAN_POINT('Ctrl Pts',(0.15727512594571,7.59811342657792,-9.45125426124965));
#63092=CARTESIAN_POINT('Ctrl Pts',(0.441539765519954,10.9634581264468,-5.22961150140885));
#63093=CARTESIAN_POINT('Ctrl Pts',(0.757961052591613,12.3120920790573,0.632947183835009));
#63094=CARTESIAN_POINT('Ctrl Pts',(1.106753006709,10.3234214073197,7.09159088554642));
#63095=CARTESIAN_POINT('Ctrl Pts',(1.48815637392869,4.54447620677922,11.6990671932346));
#63096=CARTESIAN_POINT('Ctrl Pts',(1.87044320169088,-2.84159511207509,12.2549877464399));
#63097=CARTESIAN_POINT('Ctrl Pts',(2.25360605983208,-9.26834602877216,8.54689771165241));
#63098=CARTESIAN_POINT('Ctrl Pts',(2.63764130942004,-12.506791768106,1.84154262526316));
#63099=CARTESIAN_POINT('Ctrl Pts',(2.95837917353033,-11.5770968607523,-4.29863956570323));
#63100=CARTESIAN_POINT('Ctrl Pts',(3.27964083689423,-8.18273565833188,-9.27768576125995));
#63101=CARTESIAN_POINT('Ctrl Pts',(3.56924420355609,-3.33250795673198,-12.0840904780873));
#63102=CARTESIAN_POINT('Ctrl Pts',(3.89162245652149,2.79949587180547,-12.075394977273));
#63103=CARTESIAN_POINT('Ctrl Pts',(4.18221107033807,7.77306303674672,-9.68479374718664));
#63104=CARTESIAN_POINT('Ctrl Pts',(4.47324550024543,11.2192354884859,-5.36069128118948));
#63105=CARTESIAN_POINT('Ctrl Pts',(4.81329994937238,12.6692418509689,0.938993978829623));
#63106=CARTESIAN_POINT('Ctrl Pts',(5.20264288309048,10.1607760172556,8.1446283728886));
#63107=CARTESIAN_POINT('Ctrl Pts',(5.64159910107618,2.86826488077924,12.7287442963195));
#63108=CARTESIAN_POINT('Ctrl Pts',(6.08146878975716,-5.70197123211863,11.7651487592271));
#63109=CARTESIAN_POINT('Ctrl Pts',(6.52222468717438,-11.8175960823832,5.65548456063045));
#63110=CARTESIAN_POINT('Ctrl Pts',(6.9638341956865,-12.7890005253937,-2.9511346052465));
#63111=CARTESIAN_POINT('Ctrl Pts',(7.406265245255,-8.17660276171336,-10.2982067424904));
#63112=CARTESIAN_POINT('Ctrl Pts',(7.84949033536914,0.0301268930120722,
-13.1738913494456));
#63113=CARTESIAN_POINT('Ctrl Pts',(8.21946795867107,6.8730544511525,-10.773707415888));
#63114=CARTESIAN_POINT('Ctrl Pts',(8.51582239217239,10.5734673348988,-6.61096540438714));
#63115=CARTESIAN_POINT('Ctrl Pts',(8.81241356784579,12.7202653194831,-1.46599044540228));
#63116=CARTESIAN_POINT('Ctrl Pts',(9.18357435136159,11.92282528886,5.76150100397621));
#63117=CARTESIAN_POINT('Ctrl Pts',(9.62961377853879,5.72592863888784,11.9553621584614));
#63118=CARTESIAN_POINT('Ctrl Pts',(10.0266360172958,-2.00273443034567,12.8182691334911));
#63119=CARTESIAN_POINT('Ctrl Pts',(10.3744160574443,-7.95691351092337,9.93987207302513));
#63120=CARTESIAN_POINT('Ctrl Pts',(10.6727487589153,-11.4926568425675,5.51240413664081));
#63121=CARTESIAN_POINT('Ctrl Pts',(10.9713288571319,-12.7538129729755,-0.0201879333039461));
#63122=CARTESIAN_POINT('Ctrl Pts',(11.2701178023546,-11.4913614123974,-5.55469829188671));
#63123=CARTESIAN_POINT('Ctrl Pts',(11.5691210946344,-7.94962366264769,-9.99691887323886));
#63124=CARTESIAN_POINT('Ctrl Pts',(11.8683146332215,-2.82771967206129,-12.4649155906732));
#63125=CARTESIAN_POINT('Ctrl Pts',(12.1677087571372,2.86064740523475,-12.4636884231645));
#63126=CARTESIAN_POINT('Ctrl Pts',(12.4672656194031,7.98928703920157,-9.99446720376893));
#63127=CARTESIAN_POINT('Ctrl Pts',(12.7669854736347,11.539839877033,-5.54307362452573));
#63128=CARTESIAN_POINT('Ctrl Pts',(13.0668545363388,12.8091293590171,0.0135521506018108));
#63129=CARTESIAN_POINT('Ctrl Pts',(13.3668611248283,11.5386673942862,5.56715714768572));
#63130=CARTESIAN_POINT('Ctrl Pts',(13.7170156480823,7.39700058178498,10.7796506199623));
#63131=CARTESIAN_POINT('Ctrl Pts',(14.1173696451114,-0.00500635456861792,
13.3799462588683));
#63132=CARTESIAN_POINT('Ctrl Pts',(14.5679743207715,-8.35073144806058,10.4588250356471));
#63133=CARTESIAN_POINT('Ctrl Pts',(15.0187604015418,-13.0529116373161,2.97536203022895));
#63134=CARTESIAN_POINT('Ctrl Pts',(15.4696255793761,-12.0633772300983,-5.81330552308052));
#63135=CARTESIAN_POINT('Ctrl Pts',(15.9206676140184,-5.81066798050118,-12.0651133483454));
#63136=CARTESIAN_POINT('Ctrl Pts',(16.3715292508672,2.98158699450849,-13.0587842802026));
#63137=CARTESIAN_POINT('Ctrl Pts',(16.74763550258,9.21538084923311,-9.12936080720287));
#63138=CARTESIAN_POINT('Ctrl Pts',(17.0478498402495,11.9363656394525,-4.17344447879534));
#63139=CARTESIAN_POINT('Ctrl Pts',(17.1986488358564,12.4067864910178,-1.42910559164386));
#63140=CARTESIAN_POINT('Ctrl Pts',(17.2733863906656,12.4119033132428,-0.00713853848606688));
#63141=CARTESIAN_POINT('Ctrl Pts',(-6.46451084474973,10.6219998496075,0.0107430921454236));
#63142=CARTESIAN_POINT('Ctrl Pts',(-6.39973786109817,10.6175652404827,1.24312283579603));
#63143=CARTESIAN_POINT('Ctrl Pts',(-6.27148773155715,10.2175233413502,3.57725363696463));
#63144=CARTESIAN_POINT('Ctrl Pts',(-6.01354281718277,7.88152801963195,7.83570282159969));
#63145=CARTESIAN_POINT('Ctrl Pts',(-5.6916402210612,2.54243119535446,11.1966519138041));
#63146=CARTESIAN_POINT('Ctrl Pts',(-5.30446195420775,-5.00545208161645,
10.3497136548024));
#63147=CARTESIAN_POINT('Ctrl Pts',(-4.91701686110735,-10.378305483713,4.97667753500867));
#63148=CARTESIAN_POINT('Ctrl Pts',(-4.52896396181057,-11.2325118891829,
-2.5850252195442));
#63149=CARTESIAN_POINT('Ctrl Pts',(-4.14040222720135,-7.18047154399281,
-9.03829370587454));
#63150=CARTESIAN_POINT('Ctrl Pts',(-3.75123335740469,0.0256095269495808,
-11.5617311438726));
#63151=CARTESIAN_POINT('Ctrl Pts',(-3.37588434017118,6.96841646516042,-9.13023292284201));
#63152=CARTESIAN_POINT('Ctrl Pts',(-3.01438757125082,10.9191588748908,-3.336215850523));
#63153=CARTESIAN_POINT('Ctrl Pts',(-2.72473343890907,10.9128857663664,2.27133764692916));
#63154=CARTESIAN_POINT('Ctrl Pts',(-2.52171757764907,9.25656237679485,5.69770180441265));
#63155=CARTESIAN_POINT('Ctrl Pts',(-2.40563491295491,7.9127356846986,7.38354185859245));
#63156=CARTESIAN_POINT('Ctrl Pts',(-2.2604702649357,5.93618622336592,9.21928819606915));
#63157=CARTESIAN_POINT('Ctrl Pts',(-2.05707464492104,2.456009344374,10.8972276117971));
#63158=CARTESIAN_POINT('Ctrl Pts',(-1.79521358272284,-2.5200959412735,10.8973620123061));
#63159=CARTESIAN_POINT('Ctrl Pts',(-1.53299186318285,-7.00951239375684,
8.73797920866642));
#63160=CARTESIAN_POINT('Ctrl Pts',(-1.27041014228868,-10.1206970399566,
4.83657004935519));
#63161=CARTESIAN_POINT('Ctrl Pts',(-1.00745089130815,-11.2331352219311,
-0.0338319676480412));
#63162=CARTESIAN_POINT('Ctrl Pts',(-0.744106125260249,-10.1207240761438,
-4.91302292482435));
#63163=CARTESIAN_POINT('Ctrl Pts',(-0.524326291037735,-7.51683671547534,
-8.1772128104801));
#63164=CARTESIAN_POINT('Ctrl Pts',(-0.348297896955578,-4.73656341431799,
-9.9213468149702));
#63165=CARTESIAN_POINT('Ctrl Pts',(-0.172134410376588,-1.63704484364765,
-11.0086906838672));
#63166=CARTESIAN_POINT('Ctrl Pts',(0.0483231360515193,2.55082881753386,
-11.0106551516741));
#63167=CARTESIAN_POINT('Ctrl Pts',(0.313293760511986,7.08920053100004,-8.82626877853864));
#63168=CARTESIAN_POINT('Ctrl Pts',(0.578689934519355,10.2310632724682,-4.88476898925453));
#63169=CARTESIAN_POINT('Ctrl Pts',(0.874057039176359,11.4898322642623,0.587734432288766));
#63170=CARTESIAN_POINT('Ctrl Pts',(1.19959272293443,9.63362448009566,6.61561806556494));
#63171=CARTESIAN_POINT('Ctrl Pts',(1.55552459185528,4.24058903205902,10.9153192716146));
#63172=CARTESIAN_POINT('Ctrl Pts',(1.91227491147004,-2.6520217183213,11.4340475330235));
#63173=CARTESIAN_POINT('Ctrl Pts',(2.26986112049208,-8.64968231974067,7.97358806105671));
#63174=CARTESIAN_POINT('Ctrl Pts',(2.62829340991396,-11.6723112697667,1.71535743622179));
#63175=CARTESIAN_POINT('Ctrl Pts',(2.92770617853484,-10.804591364036,-4.01651813335133));
#63176=CARTESIAN_POINT('Ctrl Pts',(3.22766556999648,-7.63540278102332,-8.66538451201058));
#63177=CARTESIAN_POINT('Ctrl Pts',(3.4981240761088,-3.10596760239311,-11.2864014018338));
#63178=CARTESIAN_POINT('Ctrl Pts',(3.79928270555332,2.62235242391335,-11.2784987560585));
#63179=CARTESIAN_POINT('Ctrl Pts',(4.07083363394759,7.27005370883939,-9.04470812959211));
#63180=CARTESIAN_POINT('Ctrl Pts',(4.34289415231203,10.4916521068476,-5.0027262212335));
#63181=CARTESIAN_POINT('Ctrl Pts',(4.66089571348296,11.8478670218135,0.888232375739401));
#63182=CARTESIAN_POINT('Ctrl Pts',(5.02519340925734,9.50159493778667,7.6303760718029));
#63183=CARTESIAN_POINT('Ctrl Pts',(5.43620055799739,2.67414369723583,11.9233586539389));
#63184=CARTESIAN_POINT('Ctrl Pts',(5.8483918643095,-5.35671023029638,11.0215334211548));
#63185=CARTESIAN_POINT('Ctrl Pts',(6.26177439049753,-11.0932021843605,5.292365326979));
#63186=CARTESIAN_POINT('Ctrl Pts',(6.67635400543509,-12.0064745014867,-2.78707182970431));
#63187=CARTESIAN_POINT('Ctrl Pts',(7.09213698834625,-7.67323447007579,-9.69208842969653));
#63188=CARTESIAN_POINT('Ctrl Pts',(7.50912165860666,0.0468454391472405,
-12.3989463730217));
#63189=CARTESIAN_POINT('Ctrl Pts',(7.85762186683386,6.49272731621592,-10.1394282360524));
#63190=CARTESIAN_POINT('Ctrl Pts',(8.1370130781375,9.98148681853618,-6.21518078295535));
#63191=CARTESIAN_POINT('Ctrl Pts',(8.41680490762239,12.006925113785,-1.36188908633659));
#63192=CARTESIAN_POINT('Ctrl Pts',(8.76730393267241,11.2553288749941,5.46305292595075));
#63193=CARTESIAN_POINT('Ctrl Pts',(9.18910851961994,5.39694230000765,11.3216601465911));
#63194=CARTESIAN_POINT('Ctrl Pts',(9.56511020248836,-1.92199990529629,12.1404778976687));
#63195=CARTESIAN_POINT('Ctrl Pts',(9.8948686207416,-7.56786642714936,9.41200252003379));
#63196=CARTESIAN_POINT('Ctrl Pts',(10.1780547485049,-10.9243129504653,5.20988772093761));
#63197=CARTESIAN_POINT('Ctrl Pts',(10.4617475384838,-12.1232577320106,-0.0466174706278744));
#63198=CARTESIAN_POINT('Ctrl Pts',(10.7459743347294,-10.9229595673016,-5.3112508257592));
#63199=CARTESIAN_POINT('Ctrl Pts',(11.0307120599722,-7.55087576180269,-9.54183041614082));
#63200=CARTESIAN_POINT('Ctrl Pts',(11.3159714208886,-2.66808064202225,-11.8953207101883));
#63201=CARTESIAN_POINT('Ctrl Pts',(11.6017219729367,2.76095286619628,-11.8949196289229));
#63202=CARTESIAN_POINT('Ctrl Pts',(11.8879901126779,7.66215797385631,-9.53596929854585));
#63203=CARTESIAN_POINT('Ctrl Pts',(12.1747562619772,11.0596787348937,-5.27762781084655));
#63204=CARTESIAN_POINT('Ctrl Pts',(12.4620164112936,12.276330565939,0.0449487542660262));
#63205=CARTESIAN_POINT('Ctrl Pts',(12.7497675937242,11.0585470320048,5.37163302664251));
#63206=CARTESIAN_POINT('Ctrl Pts',(13.0860359161205,7.08211853912157,10.3777700655797));
#63207=CARTESIAN_POINT('Ctrl Pts',(13.4711607269014,-0.0370068386633191,
12.8813060800447));
#63208=CARTESIAN_POINT('Ctrl Pts',(13.9054671788381,-8.08136907240343,10.0687773727722));
#63209=CARTESIAN_POINT('Ctrl Pts',(14.3408246393693,-12.624968966042,2.84325776332699));
#63210=CARTESIAN_POINT('Ctrl Pts',(14.7771670529737,-11.6702358127997,-5.66182189773967));
#63211=CARTESIAN_POINT('Ctrl Pts',(15.2145608917499,-5.60909929244629,-11.7270189034878));
#63212=CARTESIAN_POINT('Ctrl Pts',(15.6527884242738,2.93550487495931,-12.6948971579645));
#63213=CARTESIAN_POINT('Ctrl Pts',(16.0190063123979,9.00736970826819,-8.87180598157205));
#63214=CARTESIAN_POINT('Ctrl Pts',(16.312038702112,11.6635526352396,-4.03468871097921));
#63215=CARTESIAN_POINT('Ctrl Pts',(16.4591456512362,12.1226664499012,-1.35766244804026));
#63216=CARTESIAN_POINT('Ctrl Pts',(16.5322293926541,12.1276700456614,0.032838922831008));
#63217=CARTESIAN_POINT('Ctrl Pts',(-5.67986690813377,10.7476981461842,-0.0300449087323375));
#63218=CARTESIAN_POINT('Ctrl Pts',(-5.61446261326135,10.7432203150502,1.2143462495032));
#63219=CARTESIAN_POINT('Ctrl Pts',(-5.48474172974139,10.338418680291,3.57512573258163));
#63220=CARTESIAN_POINT('Ctrl Pts',(-5.22429202276908,7.97900472045824,7.87465592993745));
#63221=CARTESIAN_POINT('Ctrl Pts',(-4.89987273796351,2.59696395563541,11.2594571007491));
#63222=CARTESIAN_POINT('Ctrl Pts',(-4.51074074352916,-4.98843741605642,
10.4047506337951));
#63223=CARTESIAN_POINT('Ctrl Pts',(-4.12237963223429,-10.3713388494899,
5.01690086047654));
#63224=CARTESIAN_POINT('Ctrl Pts',(-3.73446117498051,-11.2218192436182,
-2.54233631811985));
#63225=CARTESIAN_POINT('Ctrl Pts',(-3.34707792581103,-7.17929284493749,
-8.97399278959156));
#63226=CARTESIAN_POINT('Ctrl Pts',(-2.96013196535152,-0.0134791104480878,
-11.4796641361566));
#63227=CARTESIAN_POINT('Ctrl Pts',(-2.58792476469585,6.86992918584355,-9.06556804792655));
#63228=CARTESIAN_POINT('Ctrl Pts',(-2.23035369122419,10.7755084984827,-3.33320230703603));
#63229=CARTESIAN_POINT('Ctrl Pts',(-1.94452142571969,10.7674793826984,2.20014896093121));
#63230=CARTESIAN_POINT('Ctrl Pts',(-1.74454263547472,9.13565802983238,5.57501603792962));
#63231=CARTESIAN_POINT('Ctrl Pts',(-1.63029710540912,7.81308261009993,7.23414756185225));
#63232=CARTESIAN_POINT('Ctrl Pts',(-1.48751289001078,5.86890020544803,9.03974351324414));
#63233=CARTESIAN_POINT('Ctrl Pts',(-1.28767164976426,2.44929606941102,10.6876936039675));
#63234=CARTESIAN_POINT('Ctrl Pts',(-1.03083752138013,-2.43121825419115,
10.6868992575839));
#63235=CARTESIAN_POINT('Ctrl Pts',(-0.774094836015582,-6.82640924735232,
8.57182122854547));
#63236=CARTESIAN_POINT('Ctrl Pts',(-0.517428636590572,-9.86675985217741,
4.75781809857857));
#63237=CARTESIAN_POINT('Ctrl Pts',(-0.260829431273375,-10.9514117086836,
0.00504714446565881));
#63238=CARTESIAN_POINT('Ctrl Pts',(-0.00427994114409397,-9.86686153589834,
-4.74799752907425));
#63239=CARTESIAN_POINT('Ctrl Pts',(0.209477030133823,-7.33380134185567,
-7.92225761692041));
#63240=CARTESIAN_POINT('Ctrl Pts',(0.380470781566099,-4.63300634635791,
-9.61637377023796));
#63241=CARTESIAN_POINT('Ctrl Pts',(0.551457441280128,-1.62450730338498,
-10.6716406274424));
#63242=CARTESIAN_POINT('Ctrl Pts',(0.765180641413356,2.43544556613168,-10.6728558702936));
#63243=CARTESIAN_POINT('Ctrl Pts',(1.02165026761106,6.82783061592847,-8.55778083035606));
#63244=CARTESIAN_POINT('Ctrl Pts',(1.27813102224132,9.86352480724084,-4.74819843566146));
#63245=CARTESIAN_POINT('Ctrl Pts',(1.56313651150202,11.0772375739532,0.532638737281799));
#63246=CARTESIAN_POINT('Ctrl Pts',(1.8766998993098,9.28760209391739,6.33834310175836));
#63247=CARTESIAN_POINT('Ctrl Pts',(2.21886909367739,4.10188743890763,10.4702862968775));
#63248=CARTESIAN_POINT('Ctrl Pts',(2.56116042531579,-2.51158893027609,10.966193922874));
#63249=CARTESIAN_POINT('Ctrl Pts',(2.90361377532428,-8.25466119657915,7.65060657153079));
#63250=CARTESIAN_POINT('Ctrl Pts',(3.24625901396941,-11.1425949229273,1.66715126822539));
#63251=CARTESIAN_POINT('Ctrl Pts',(3.53197933085045,-10.3132181039043,-3.80246223862247));
#63252=CARTESIAN_POINT('Ctrl Pts',(3.81785656818665,-7.29245349613011,-8.23289553288844));
#63253=CARTESIAN_POINT('Ctrl Pts',(4.07529235944329,-2.98044886201398,-10.726822682243));
#63254=CARTESIAN_POINT('Ctrl Pts',(4.36154951821464,2.46446136838667,-10.7184995863623));
#63255=CARTESIAN_POINT('Ctrl Pts',(4.61935550740964,6.87674774915925,-8.59720962983951));
#63256=CARTESIAN_POINT('Ctrl Pts',(4.87734897679494,9.93138387504632,-4.76372459953767));
#63257=CARTESIAN_POINT('Ctrl Pts',(5.17858169940585,11.2154055251366,0.81693402950548));
#63258=CARTESIAN_POINT('Ctrl Pts',(5.52319110276872,8.99418327156995,7.19444176827225));
#63259=CARTESIAN_POINT('Ctrl Pts',(5.91140672757681,2.54413577000337,11.247876132119));
#63260=CARTESIAN_POINT('Ctrl Pts',(6.30017748440511,-5.03048374964069,10.3954931992179));
#63261=CARTESIAN_POINT('Ctrl Pts',(6.68954510735853,-10.432763020561,4.99777633096148));
#63262=CARTESIAN_POINT('Ctrl Pts',(7.07954892180132,-11.2903897670847,-2.60315821386011));
#63263=CARTESIAN_POINT('Ctrl Pts',(7.47022118865678,-7.21747965815942,-9.09075239737114));
#63264=CARTESIAN_POINT('Ctrl Pts',(7.86160367679631,0.0293157389431672,
-11.6302094613265));
#63265=CARTESIAN_POINT('Ctrl Pts',(8.18836008818057,6.07305731078864,-9.51067643046102));
#63266=CARTESIAN_POINT('Ctrl Pts',(8.45017202789412,9.34226240457075,-5.83317563617857));
#63267=CARTESIAN_POINT('Ctrl Pts',(8.71224807096988,11.2393094987126,-1.2869623709495));
#63268=CARTESIAN_POINT('Ctrl Pts',(9.0403378978682,10.5350241421098,5.10193081371875));
#63269=CARTESIAN_POINT('Ctrl Pts',(9.43487539495064,5.05431032876375,10.5813936281332));
#63270=CARTESIAN_POINT('Ctrl Pts',(9.78634691457013,-1.7876785094993,11.3463953829615));
#63271=CARTESIAN_POINT('Ctrl Pts',(10.0944857195819,-7.06345577776651,8.79648617998475));
#63272=CARTESIAN_POINT('Ctrl Pts',(10.358998280792,-10.19877817368,4.87114494261225));
#63273=CARTESIAN_POINT('Ctrl Pts',(10.6239497905261,-11.3183484730333,-0.0382477388943832));
#63274=CARTESIAN_POINT('Ctrl Pts',(10.8893064308135,-10.1976583163031,-4.95368746912103));
#63275=CARTESIAN_POINT('Ctrl Pts',(11.1551028378205,-7.04964451414481,-8.90293670258816));
#63276=CARTESIAN_POINT('Ctrl Pts',(11.4213273795416,-2.49231916840097,-11.099568267378));
#63277=CARTESIAN_POINT('Ctrl Pts',(11.6880226277189,2.57482727977078,-11.0990792013691));
#63278=CARTESIAN_POINT('Ctrl Pts',(11.9551548606348,7.14869677466965,-8.89770335751692));
#63279=CARTESIAN_POINT('Ctrl Pts',(12.2227507809561,10.3192851058014,-4.923781451297));
#63280=CARTESIAN_POINT('Ctrl Pts',(12.4908155555466,11.454693239686,0.0433976178169967));
#63281=CARTESIAN_POINT('Ctrl Pts',(12.7593530592786,10.3181824292637,5.0147287420611));
#63282=CARTESIAN_POINT('Ctrl Pts',(13.0732143174343,6.60660401385552,9.68752965695795));
#63283=CARTESIAN_POINT('Ctrl Pts',(13.4326981334329,-0.0391034732694524,
12.0247678504407));
#63284=CARTESIAN_POINT('Ctrl Pts',(13.8382440069182,-7.55120859904456,9.39895212335986));
#63285=CARTESIAN_POINT('Ctrl Pts',(14.2449041216069,-11.7963627755015,2.64906040860919));
#63286=CARTESIAN_POINT('Ctrl Pts',(14.6527221776558,-10.9045091416774,-5.29961988595021));
#63287=CARTESIAN_POINT('Ctrl Pts',(15.0616548396602,-5.2376856166355,-10.9731166019128));
#63288=CARTESIAN_POINT('Ctrl Pts',(15.471829200061,2.75900263637003,-11.8777086663017));
#63289=CARTESIAN_POINT('Ctrl Pts',(15.8144664683391,8.44283296966011,-8.3026767417502));
#63290=CARTESIAN_POINT('Ctrl Pts',(16.0894080251075,10.9344522487339,-3.76400044022369));
#63291=CARTESIAN_POINT('Ctrl Pts',(16.22689108617,11.363370689184,-1.26185267405424));
#63292=CARTESIAN_POINT('Ctrl Pts',(16.2957361032235,11.368084085471,0.048002140892809));
#63293=CARTESIAN_POINT('Ctrl Pts',(-5.41932283393119,11.2066320607065,-0.042087482955348));
#63294=CARTESIAN_POINT('Ctrl Pts',(-5.35137534985207,11.2019801129976,1.25069074479452));
#63295=CARTESIAN_POINT('Ctrl Pts',(-5.21590591317433,10.7792648066367,3.71609498960973));
#63296=CARTESIAN_POINT('Ctrl Pts',(-4.94473010944745,8.32199851399102,8.19258769576774));
#63297=CARTESIAN_POINT('Ctrl Pts',(-4.60678174808354,2.71605117015634,11.7185839329575));
#63298=CARTESIAN_POINT('Ctrl Pts',(-4.20200848807542,-5.17493114747134,
10.8269092912904));
#63299=CARTESIAN_POINT('Ctrl Pts',(-3.79831788923914,-10.7692241637846,
5.22634871152499));
#63300=CARTESIAN_POINT('Ctrl Pts',(-3.39554019651669,-11.6507475814523,
-2.62320453575906));
#63301=CARTESIAN_POINT('Ctrl Pts',(-2.9937247156788,-7.45642177572264,-9.29347997110535));
#63302=CARTESIAN_POINT('Ctrl Pts',(-2.59281954230867,-0.0314947741782245,
-11.8880880574117));
#63303=CARTESIAN_POINT('Ctrl Pts',(-2.20763151462572,7.09137672622204,-9.38831096546065));
#63304=CARTESIAN_POINT('Ctrl Pts',(-1.83801780398024,11.1273516583463,-3.46219474862477));
#63305=CARTESIAN_POINT('Ctrl Pts',(-1.54289134094969,11.1180669417964,2.25097185675394));
#63306=CARTESIAN_POINT('Ctrl Pts',(-1.33659549689802,9.43453563826111,5.73231011590964));
#63307=CARTESIAN_POINT('Ctrl Pts',(-1.21879423805378,8.07078426906925,7.44305473514828));
#63308=CARTESIAN_POINT('Ctrl Pts',(-1.07160989639206,6.06666256340522,9.3042532528442));
#63309=CARTESIAN_POINT('Ctrl Pts',(-0.865721126447319,2.54347562052076,
11.0016216538497));
#63310=CARTESIAN_POINT('Ctrl Pts',(-0.601366668027522,-2.47985430754189,
11.0002382352452));
#63311=CARTESIAN_POINT('Ctrl Pts',(-0.337362664902254,-6.99903814490822,
8.82485175419817));
#63312=CARTESIAN_POINT('Ctrl Pts',(-0.0736781085903364,-10.1219770993773,
4.90632513314084));
#63313=CARTESIAN_POINT('Ctrl Pts',(0.189674992112668,-11.2345321689752,
0.0284646833159565));
#63314=CARTESIAN_POINT('Ctrl Pts',(0.452713392534164,-10.1220192338548,
-4.84453573727029));
#63315=CARTESIAN_POINT('Ctrl Pts',(0.67166289107924,-7.52713561183215,-8.09544463026128));
#63316=CARTESIAN_POINT('Ctrl Pts',(0.846659961397844,-4.76311866049559,
-9.82909249637171));
#63317=CARTESIAN_POINT('Ctrl Pts',(1.02155884886147,-1.68579159229165,-10.9083821192465));
#63318=CARTESIAN_POINT('Ctrl Pts',(1.24002127021466,2.46400024803699,-10.9091007101121));
#63319=CARTESIAN_POINT('Ctrl Pts',(1.50188875307738,6.94836187168817,-8.74897629394682));
#63320=CARTESIAN_POINT('Ctrl Pts',(1.76348785755158,10.0440333746524,-4.8631934000533));
#63321=CARTESIAN_POINT('Ctrl Pts',(2.05386804068059,11.2798367272638,0.517220777416554));
#63322=CARTESIAN_POINT('Ctrl Pts',(2.3729315528289,9.4575572459586,6.4240027363545));
#63323=CARTESIAN_POINT('Ctrl Pts',(2.7205670766896,4.18824339806379,10.6206519716963));
#63324=CARTESIAN_POINT('Ctrl Pts',(3.06783538831903,-2.52100451397122,11.1220703552258));
#63325=CARTESIAN_POINT('Ctrl Pts',(3.41474007347489,-8.33749572436887,7.76230524925844));
#63326=CARTESIAN_POINT('Ctrl Pts',(3.76127533593318,-11.2565584243436,1.71039090787414));
#63327=CARTESIAN_POINT('Ctrl Pts',(4.04979793075202,-10.4177720610343,-3.8122691837163));
#63328=CARTESIAN_POINT('Ctrl Pts',(4.33813888512292,-7.3708240398822,-8.28046921219318));
#63329=CARTESIAN_POINT('Ctrl Pts',(4.59748984245561,-3.02638582682191,-10.7917381636151));
#63330=CARTESIAN_POINT('Ctrl Pts',(4.88546721176517,2.45091539459955,-10.7826813104226));
#63331=CARTESIAN_POINT('Ctrl Pts',(5.1445304772252,6.8841451987017,-8.65056781137807));
#63332=CARTESIAN_POINT('Ctrl Pts',(5.40347503369346,9.94931917680866,-4.8029005855658));
#63333=CARTESIAN_POINT('Ctrl Pts',(5.70543829551453,11.2356366599343,0.791211519736368));
#63334=CARTESIAN_POINT('Ctrl Pts',(6.05041155649914,9.01047842727854,7.17417649627677));
#63335=CARTESIAN_POINT('Ctrl Pts',(6.43831251816865,2.56488255568998,11.221964058039));
#63336=CARTESIAN_POINT('Ctrl Pts',(6.82608149851452,-4.98922558908911,10.3695983640868));
#63337=CARTESIAN_POINT('Ctrl Pts',(7.21375130836792,-10.3658135964222,4.99423232717637));
#63338=CARTESIAN_POINT('Ctrl Pts',(7.60136603652376,-11.2158267380261,-2.55973461164996));
#63339=CARTESIAN_POINT('Ctrl Pts',(7.98897057760673,-7.1733026858818,-8.99441899699579));
#63340=CARTESIAN_POINT('Ctrl Pts',(8.37658932011228,0.00392856028059459,
-11.5071255880267));
#63341=CARTESIAN_POINT('Ctrl Pts',(8.69968664503721,5.97856800044611,-9.40978986256599));
#63342=CARTESIAN_POINT('Ctrl Pts',(8.95817703611359,9.20571407746475,-5.77898138198752));
#63343=CARTESIAN_POINT('Ctrl Pts',(9.2167056998336,11.0767826600461,-1.29431029410649));
#63344=CARTESIAN_POINT('Ctrl Pts',(9.53998065507207,10.3809719106831,5.00005882195924));
#63345=CARTESIAN_POINT('Ctrl Pts',(9.92811301733877,4.98849876033169,10.3884980338129));
#63346=CARTESIAN_POINT('Ctrl Pts',(10.2733240631819,-1.73084177545552,11.1376898201042));
#63347=CARTESIAN_POINT('Ctrl Pts',(10.5755152860084,-6.90406708108543,8.63662622633531));
#63348=CARTESIAN_POINT('Ctrl Pts',(10.8346933356035,-9.97516159898725,4.79048819392321));
#63349=CARTESIAN_POINT('Ctrl Pts',(11.0939653660262,-11.0702259099571,-0.0135751203614283));
#63350=CARTESIAN_POINT('Ctrl Pts',(11.3534266941978,-9.97385187625692,-4.81905256665219));
#63351=CARTESIAN_POINT('Ctrl Pts',(11.6130348161363,-6.8990164224985,-8.67574529438917));
#63352=CARTESIAN_POINT('Ctrl Pts',(11.8728380427865,-2.45193812959834,-10.8184872441865));
#63353=CARTESIAN_POINT('Ctrl Pts',(12.1327787286265,2.48659962412208,-10.8176046460576));
#63354=CARTESIAN_POINT('Ctrl Pts',(12.3929463229376,6.94048671101919,-8.67331817585549));
#63355=CARTESIAN_POINT('Ctrl Pts',(12.6533133617581,10.0247151711056,-4.80685928816532));
#63356=CARTESIAN_POINT('Ctrl Pts',(12.9138935700488,11.1278743123892,0.0212671221230969));
#63357=CARTESIAN_POINT('Ctrl Pts',(13.1746990466231,10.0237725509645,4.8488500652197));
#63358=CARTESIAN_POINT('Ctrl Pts',(13.4792357338148,6.42231691433516,9.38216239452379));
#63359=CARTESIAN_POINT('Ctrl Pts',(13.8277236270411,-0.0196751530098743,
11.6463691748063));
#63360=CARTESIAN_POINT('Ctrl Pts',(14.2203419461442,-7.29096552102109,9.10302117489524));
#63361=CARTESIAN_POINT('Ctrl Pts',(14.6135758516643,-11.3943036180612,2.57588820150967));
#63362=CARTESIAN_POINT('Ctrl Pts',(15.007488851134,-10.5314196001733,-5.10041524523971));
#63363=CARTESIAN_POINT('Ctrl Pts',(15.4020230740337,-5.0636124069355,-10.5732295009402));
#63364=CARTESIAN_POINT('Ctrl Pts',(15.7974191042731,2.64381940191114,-11.4427898367074));
#63365=CARTESIAN_POINT('Ctrl Pts',(16.1272780854274,8.11545700277838,-8.00135572866133));
#63366=CARTESIAN_POINT('Ctrl Pts',(16.3919825984395,10.51368582042,-3.63176898342513));
#63367=CARTESIAN_POINT('Ctrl Pts',(16.5239960017223,10.9257856408219,-1.22936672503705));
#63368=CARTESIAN_POINT('Ctrl Pts',(16.5904023640647,10.9303320773702,0.0340899081360551));
#63369=CARTESIAN_POINT('Ctrl Pts',(-5.40297363237939,11.445432490473,-0.042087482955348));
#63370=CARTESIAN_POINT('Ctrl Pts',(-5.33369696111111,11.4406895414653,1.27598004405306));
#63371=CARTESIAN_POINT('Ctrl Pts',(-5.19521862607164,11.0085774465653,3.79612986924071));
#63372=CARTESIAN_POINT('Ctrl Pts',(-4.91840015088629,8.49992872694836,8.36573269447326));
#63373=CARTESIAN_POINT('Ctrl Pts',(-4.57320339639667,2.77438806679843,11.967805106163));
#63374=CARTESIAN_POINT('Ctrl Pts',(-4.15990469688328,-5.28321395100969,
11.056569093912));
#63375=CARTESIAN_POINT('Ctrl Pts',(-3.747686811287,-10.9955419925911,5.33820880446098));
#63376=CARTESIAN_POINT('Ctrl Pts',(-3.33647538038886,-11.8953437286105,
-2.67607624391012));
#63377=CARTESIAN_POINT('Ctrl Pts',(-2.92629230091383,-7.61357058494829,
-9.48509907357355));
#63378=CARTESIAN_POINT('Ctrl Pts',(-2.51711411539744,-0.0352081461009456,
-12.133141923791));
#63379=CARTESIAN_POINT('Ctrl Pts',(-2.12405346851776,7.23325257089384,-9.58201967934875));
#63380=CARTESIAN_POINT('Ctrl Pts',(-1.74697035839629,11.3507348234515,-3.53593739186965));
#63381=CARTESIAN_POINT('Ctrl Pts',(-1.44594495704173,11.3410956049915,2.29151330201399));
#63382=CARTESIAN_POINT('Ctrl Pts',(-1.23555813837642,9.62414272926665,5.84190263222694));
#63383=CARTESIAN_POINT('Ctrl Pts',(-1.11543119956109,8.23345778533256,7.58643680207061));
#63384=CARTESIAN_POINT('Ctrl Pts',(-0.965350761047819,6.18988758696103,
9.48427609552777));
#63385=CARTESIAN_POINT('Ctrl Pts',(-0.755455752947343,2.59800826091561,
11.2146857757666));
#63386=CARTESIAN_POINT('Ctrl Pts',(-0.486005297879084,-2.52226170629262,
11.2131697972667));
#63387=CARTESIAN_POINT('Ctrl Pts',(-0.216964169512981,-7.12771226807027,
8.99614845847778));
#63388=CARTESIAN_POINT('Ctrl Pts',(0.051673199605982,-10.3093017586739,
5.0037967419436));
#63389=CARTESIAN_POINT('Ctrl Pts',(0.319912004204202,-11.4424452984132,
0.0352862821531482));
#63390=CARTESIAN_POINT('Ctrl Pts',(0.587759827560524,-10.3093945561263,
-4.92692882386994));
#63391=CARTESIAN_POINT('Ctrl Pts',(0.810644510337,-7.66768866486485,-8.23632315062337));
#63392=CARTESIAN_POINT('Ctrl Pts',(0.9887628738834,-4.85431418623128,-10.0009017448057));
#63393=CARTESIAN_POINT('Ctrl Pts',(1.16675569936477,-1.72248496421437,-11.0992889627176));
#63394=CARTESIAN_POINT('Ctrl Pts',(1.38901397173341,2.49959534000996,-11.0999021750131));
#63395=CARTESIAN_POINT('Ctrl Pts',(1.65535913685916,7.06073570919373,-8.90264472811187));
#63396=CARTESIAN_POINT('Ctrl Pts',(1.92134523430893,10.2082911979719,-4.95142581114747));
#63397=CARTESIAN_POINT('Ctrl Pts',(2.21649491340346,11.464268710378,0.517623581655109));
#63398=CARTESIAN_POINT('Ctrl Pts',(2.54067136572795,9.61231028484355,6.51924754582076));
#63399=CARTESIAN_POINT('Ctrl Pts',(2.89372530199723,4.26040343756882,10.7809878391944));
#63400=CARTESIAN_POINT('Ctrl Pts',(3.24620579430313,-2.5499807271206,11.2895594263092));
#63401=CARTESIAN_POINT('Ctrl Pts',(3.59813519099429,-8.45086172951072,7.88046583695986));
#63402=CARTESIAN_POINT('Ctrl Pts',(3.94952923360969,-11.4105207073045,1.7432987177926));
#63403=CARTESIAN_POINT('Ctrl Pts',(4.24193167813174,-10.5600221745821,-3.85384587814088));
#63404=CARTESIAN_POINT('Ctrl Pts',(4.53402805814432,-7.47314001623606,-8.38031426693708));
#63405=CARTESIAN_POINT('Ctrl Pts',(4.79664370266186,-3.07363708606063,-10.9230350253262));
#63406=CARTESIAN_POINT('Ctrl Pts',(5.08810557752102,2.47013445948664,-10.9134823314909));
#63407=CARTESIAN_POINT('Ctrl Pts',(5.35017440554513,6.95492422204958,-8.75633618182547));
#63408=CARTESIAN_POINT('Ctrl Pts',(5.61200361956877,10.0542035018942,-4.86537952153394));
#63409=CARTESIAN_POINT('Ctrl Pts',(5.91720482332597,11.3540414258911,0.789064544875747));
#63410=CARTESIAN_POINT('Ctrl Pts',(6.26564105547289,9.10553979339257,7.23636750926088));
#63411=CARTESIAN_POINT('Ctrl Pts',(6.65717646488775,2.59867870246558,11.321535036503));
#63412=CARTESIAN_POINT('Ctrl Pts',(7.04828730943666,-5.02094595929096,10.4607994583915));
#63413=CARTESIAN_POINT('Ctrl Pts',(7.43900933211819,-10.4395500322981,5.04208746732736));
#63414=CARTESIAN_POINT('Ctrl Pts',(7.82938055234697,-11.2946782793107,-2.56617594127693));
#63415=CARTESIAN_POINT('Ctrl Pts',(8.21943575999143,-7.22551638204153,-9.04156914965989));
#63416=CARTESIAN_POINT('Ctrl Pts',(8.60921106212656,-0.0075686889805855,
-11.5674090717167));
#63417=CARTESIAN_POINT('Ctrl Pts',(8.93382080129404,5.99528673196386,-9.45936192902959));
#63418=CARTESIAN_POINT('Ctrl Pts',(9.19340748731854,9.23614030177817,-5.81293639312917));
#63419=CARTESIAN_POINT('Ctrl Pts',(9.45293101808351,11.1142702697208,-1.3107448337562));
#63420=CARTESIAN_POINT('Ctrl Pts',(9.77723136794952,10.4154952826205,5.00401083523754));
#63421=CARTESIAN_POINT('Ctrl Pts',(10.1662605952158,5.00921490063267,10.4044353775234));
#63422=CARTESIAN_POINT('Ctrl Pts',(10.5119839322498,-1.72077939907436,11.154116840079));
#63423=CARTESIAN_POINT('Ctrl Pts',(10.8144567422258,-6.89887898300864,8.65022675987097));
#63424=CARTESIAN_POINT('Ctrl Pts',(11.0737061869649,-9.97097573622103,4.80256799145211));
#63425=CARTESIAN_POINT('Ctrl Pts',(11.332954454476,-11.0656005972151,-0.0012636146746602));
#63426=CARTESIAN_POINT('Ctrl Pts',(11.592212676988,-9.96981484505854,-4.80333442118138));
#63427=CARTESIAN_POINT('Ctrl Pts',(11.8514921790329,-6.89841951530921,-8.65513848120015));
#63428=CARTESIAN_POINT('Ctrl Pts',(12.1108041978391,-2.45923784927583,-10.7938299796143));
#63429=CARTESIAN_POINT('Ctrl Pts',(12.3701601255276,2.46836208123245,-10.7925664321256));
#63430=CARTESIAN_POINT('Ctrl Pts',(12.6295710107042,6.9094980637413,-8.65413386138286));
#63431=CARTESIAN_POINT('Ctrl Pts',(12.8890481983849,9.98316171476258,-4.8004177652554));
#63432=CARTESIAN_POINT('Ctrl Pts',(13.1486032818335,11.0817124894507,0.00909499825818533));
#63433=CARTESIAN_POINT('Ctrl Pts',(13.4082458776239,9.98216422539828,4.81540788001813));
#63434=CARTESIAN_POINT('Ctrl Pts',(13.7112804745406,6.39794424339377,9.32638055254148));
#63435=CARTESIAN_POINT('Ctrl Pts',(14.0577858522366,-0.00835395432331517,
11.5770141955486));
#63436=CARTESIAN_POINT('Ctrl Pts',(14.4478987172592,-7.23337005489467,9.04881838019601));
#63437=CARTESIAN_POINT('Ctrl Pts',(14.8383177312182,-11.3068424364633,2.56726391915326));
#63438=CARTESIAN_POINT('Ctrl Pts',(15.2291319944184,-10.4497082271469,-5.04888270590908));
#63439=CARTESIAN_POINT('Ctrl Pts',(15.6202557238013,-5.02806227013448,-10.4744930049956));
#63440=CARTESIAN_POINT('Ctrl Pts',(16.0119892870161,2.60831854215743,-11.3347514386656));
#63441=CARTESIAN_POINT('Ctrl Pts',(16.338482088023,8.02442066121112,-7.9277656209221));
#63442=CARTESIAN_POINT('Ctrl Pts',(16.6004710641513,10.3977390912262,-3.60280630418266));
#63443=CARTESIAN_POINT('Ctrl Pts',(16.7309850253063,10.8049718643827,-1.22750855798432));
#63444=CARTESIAN_POINT('Ctrl Pts',(16.796746560446,10.8094741535653,0.0236795036592751));
#63445=CARTESIAN_POINT('',(-5.40297363237939,11.445432490473,-0.042087482955348));
#63446=CARTESIAN_POINT('Origin',(-6.2,11.5,0.));
#63447=CARTESIAN_POINT('',(16.796746560446,10.8094741535653,0.0236795036592751));
#63448=CARTESIAN_POINT('Ctrl Pts',(-5.40297363237939,11.445432490473,-0.042087482955348));
#63449=CARTESIAN_POINT('Ctrl Pts',(-5.33369696111111,11.4406895414653,1.27598004405306));
#63450=CARTESIAN_POINT('Ctrl Pts',(-5.19521862607164,11.0085774465653,3.79612986924071));
#63451=CARTESIAN_POINT('Ctrl Pts',(-4.91840015088629,8.49992872694836,8.36573269447326));
#63452=CARTESIAN_POINT('Ctrl Pts',(-4.57320339639667,2.77438806679843,11.967805106163));
#63453=CARTESIAN_POINT('Ctrl Pts',(-4.15990469688328,-5.28321395100969,
11.056569093912));
#63454=CARTESIAN_POINT('Ctrl Pts',(-3.747686811287,-10.9955419925911,5.33820880446098));
#63455=CARTESIAN_POINT('Ctrl Pts',(-3.33647538038886,-11.8953437286105,
-2.67607624391012));
#63456=CARTESIAN_POINT('Ctrl Pts',(-2.92629230091383,-7.61357058494829,
-9.48509907357355));
#63457=CARTESIAN_POINT('Ctrl Pts',(-2.51711411539744,-0.0352081461009456,
-12.133141923791));
#63458=CARTESIAN_POINT('Ctrl Pts',(-2.12405346851776,7.23325257089384,-9.58201967934875));
#63459=CARTESIAN_POINT('Ctrl Pts',(-1.74697035839629,11.3507348234515,-3.53593739186965));
#63460=CARTESIAN_POINT('Ctrl Pts',(-1.44594495704173,11.3410956049915,2.29151330201399));
#63461=CARTESIAN_POINT('Ctrl Pts',(-1.23555813837642,9.62414272926665,5.84190263222694));
#63462=CARTESIAN_POINT('Ctrl Pts',(-1.11543119956109,8.23345778533256,7.58643680207061));
#63463=CARTESIAN_POINT('Ctrl Pts',(-0.965350761047819,6.18988758696103,
9.48427609552777));
#63464=CARTESIAN_POINT('Ctrl Pts',(-0.755455752947343,2.59800826091561,
11.2146857757666));
#63465=CARTESIAN_POINT('Ctrl Pts',(-0.486005297879084,-2.52226170629262,
11.2131697972667));
#63466=CARTESIAN_POINT('Ctrl Pts',(-0.216964169512981,-7.12771226807027,
8.99614845847778));
#63467=CARTESIAN_POINT('Ctrl Pts',(0.051673199605982,-10.3093017586739,
5.0037967419436));
#63468=CARTESIAN_POINT('Ctrl Pts',(0.319912004204202,-11.4424452984132,
0.0352862821531482));
#63469=CARTESIAN_POINT('Ctrl Pts',(0.587759827560524,-10.3093945561263,
-4.92692882386994));
#63470=CARTESIAN_POINT('Ctrl Pts',(0.810644510337,-7.66768866486485,-8.23632315062337));
#63471=CARTESIAN_POINT('Ctrl Pts',(0.9887628738834,-4.85431418623128,-10.0009017448057));
#63472=CARTESIAN_POINT('Ctrl Pts',(1.16675569936477,-1.72248496421437,-11.0992889627176));
#63473=CARTESIAN_POINT('Ctrl Pts',(1.38901397173341,2.49959534000996,-11.0999021750131));
#63474=CARTESIAN_POINT('Ctrl Pts',(1.65535913685916,7.06073570919373,-8.90264472811187));
#63475=CARTESIAN_POINT('Ctrl Pts',(1.92134523430893,10.2082911979719,-4.95142581114747));
#63476=CARTESIAN_POINT('Ctrl Pts',(2.21649491340346,11.464268710378,0.517623581655109));
#63477=CARTESIAN_POINT('Ctrl Pts',(2.54067136572795,9.61231028484355,6.51924754582076));
#63478=CARTESIAN_POINT('Ctrl Pts',(2.89372530199723,4.26040343756882,10.7809878391944));
#63479=CARTESIAN_POINT('Ctrl Pts',(3.24620579430313,-2.5499807271206,11.2895594263092));
#63480=CARTESIAN_POINT('Ctrl Pts',(3.59813519099429,-8.45086172951072,7.88046583695986));
#63481=CARTESIAN_POINT('Ctrl Pts',(3.94952923360969,-11.4105207073045,1.7432987177926));
#63482=CARTESIAN_POINT('Ctrl Pts',(4.24193167813174,-10.5600221745821,-3.85384587814088));
#63483=CARTESIAN_POINT('Ctrl Pts',(4.53402805814432,-7.47314001623606,-8.38031426693708));
#63484=CARTESIAN_POINT('Ctrl Pts',(4.79664370266186,-3.07363708606063,-10.9230350253262));
#63485=CARTESIAN_POINT('Ctrl Pts',(5.08810557752102,2.47013445948664,-10.9134823314909));
#63486=CARTESIAN_POINT('Ctrl Pts',(5.35017440554513,6.95492422204958,-8.75633618182547));
#63487=CARTESIAN_POINT('Ctrl Pts',(5.61200361956877,10.0542035018942,-4.86537952153394));
#63488=CARTESIAN_POINT('Ctrl Pts',(5.91720482332597,11.3540414258911,0.789064544875747));
#63489=CARTESIAN_POINT('Ctrl Pts',(6.26564105547289,9.10553979339257,7.23636750926088));
#63490=CARTESIAN_POINT('Ctrl Pts',(6.65717646488775,2.59867870246558,11.321535036503));
#63491=CARTESIAN_POINT('Ctrl Pts',(7.04828730943666,-5.02094595929096,10.4607994583915));
#63492=CARTESIAN_POINT('Ctrl Pts',(7.43900933211819,-10.4395500322981,5.04208746732736));
#63493=CARTESIAN_POINT('Ctrl Pts',(7.82938055234697,-11.2946782793107,-2.56617594127693));
#63494=CARTESIAN_POINT('Ctrl Pts',(8.21943575999143,-7.22551638204153,-9.04156914965989));
#63495=CARTESIAN_POINT('Ctrl Pts',(8.60921106212656,-0.0075686889805855,
-11.5674090717167));
#63496=CARTESIAN_POINT('Ctrl Pts',(8.93382080129404,5.99528673196386,-9.45936192902959));
#63497=CARTESIAN_POINT('Ctrl Pts',(9.19340748731854,9.23614030177817,-5.81293639312917));
#63498=CARTESIAN_POINT('Ctrl Pts',(9.45293101808351,11.1142702697208,-1.3107448337562));
#63499=CARTESIAN_POINT('Ctrl Pts',(9.77723136794952,10.4154952826205,5.00401083523754));
#63500=CARTESIAN_POINT('Ctrl Pts',(10.1662605952158,5.00921490063267,10.4044353775234));
#63501=CARTESIAN_POINT('Ctrl Pts',(10.5119839322498,-1.72077939907436,11.154116840079));
#63502=CARTESIAN_POINT('Ctrl Pts',(10.8144567422258,-6.89887898300864,8.65022675987097));
#63503=CARTESIAN_POINT('Ctrl Pts',(11.0737061869649,-9.97097573622103,4.80256799145211));
#63504=CARTESIAN_POINT('Ctrl Pts',(11.332954454476,-11.0656005972151,-0.0012636146746602));
#63505=CARTESIAN_POINT('Ctrl Pts',(11.592212676988,-9.96981484505854,-4.80333442118138));
#63506=CARTESIAN_POINT('Ctrl Pts',(11.8514921790329,-6.89841951530921,-8.65513848120015));
#63507=CARTESIAN_POINT('Ctrl Pts',(12.1108041978391,-2.45923784927583,-10.7938299796143));
#63508=CARTESIAN_POINT('Ctrl Pts',(12.3701601255276,2.46836208123245,-10.7925664321256));
#63509=CARTESIAN_POINT('Ctrl Pts',(12.6295710107042,6.9094980637413,-8.65413386138286));
#63510=CARTESIAN_POINT('Ctrl Pts',(12.8890481983849,9.98316171476258,-4.8004177652554));
#63511=CARTESIAN_POINT('Ctrl Pts',(13.1486032818335,11.0817124894507,0.00909499825818533));
#63512=CARTESIAN_POINT('Ctrl Pts',(13.4082458776239,9.98216422539828,4.81540788001813));
#63513=CARTESIAN_POINT('Ctrl Pts',(13.7112804745406,6.39794424339377,9.32638055254148));
#63514=CARTESIAN_POINT('Ctrl Pts',(14.0577858522366,-0.00835395432331517,
11.5770141955486));
#63515=CARTESIAN_POINT('Ctrl Pts',(14.4478987172592,-7.23337005489467,9.04881838019601));
#63516=CARTESIAN_POINT('Ctrl Pts',(14.8383177312182,-11.3068424364633,2.56726391915326));
#63517=CARTESIAN_POINT('Ctrl Pts',(15.2291319944184,-10.4497082271469,-5.04888270590908));
#63518=CARTESIAN_POINT('Ctrl Pts',(15.6202557238013,-5.02806227013448,-10.4744930049956));
#63519=CARTESIAN_POINT('Ctrl Pts',(16.0119892870161,2.60831854215743,-11.3347514386656));
#63520=CARTESIAN_POINT('Ctrl Pts',(16.338482088023,8.02442066121112,-7.9277656209221));
#63521=CARTESIAN_POINT('Ctrl Pts',(16.6004710641513,10.3977390912262,-3.60280630418266));
#63522=CARTESIAN_POINT('Ctrl Pts',(16.7309850253063,10.8049718643827,-1.22750855798432));
#63523=CARTESIAN_POINT('Ctrl Pts',(16.796746560446,10.8094741535653,0.0236795036592751));
#63524=CARTESIAN_POINT('Origin',(17.2,11.5,-1.69309011255336E-14));
#63525=CARTESIAN_POINT('Origin',(17.2,11.5,-1.69309011255336E-14));
#63526=CARTESIAN_POINT('Origin',(-6.2,11.5,0.));
#63527=CARTESIAN_POINT('',(0.,0.,0.));
#63528=CARTESIAN_POINT('Origin',(18.5,0.,0.));
#63529=CARTESIAN_POINT('',(18.,-1.16341445918999E-15,9.5));
#63530=CARTESIAN_POINT('Origin',(18.,0.,0.));
#63531=CARTESIAN_POINT('',(18.5,-1.10218211923262E-15,9.));
#63532=CARTESIAN_POINT('Origin',(18.5,-1.16341445918999E-15,9.5));
#63533=CARTESIAN_POINT('',(18.5,-9.,-1.10218211923262E-15));
#63534=CARTESIAN_POINT('Origin',(18.5,0.,0.));
#63535=CARTESIAN_POINT('Origin',(18.5,0.,0.));
#63536=CARTESIAN_POINT('Origin',(19.5,0.,0.));
#63537=CARTESIAN_POINT('',(20.5,-1.10218211923262E-15,9.));
#63538=CARTESIAN_POINT('',(20.5,-9.,-1.10218211923262E-15));
#63539=CARTESIAN_POINT('Origin',(20.5,0.,0.));
#63540=CARTESIAN_POINT('Origin',(20.5,0.,0.));
#63541=CARTESIAN_POINT('',(19.5,-9.,-1.10218211923262E-15));
#63542=CARTESIAN_POINT('Origin',(18.,18.5,0.));
#63543=CARTESIAN_POINT('',(18.,10.8187337521542,-14.3542676580869));
#63544=CARTESIAN_POINT('',(18.,11.4987322084552,-15.034266114388));
#63545=CARTESIAN_POINT('',(18.,9.32726009489054,-12.8627940008233));
#63546=CARTESIAN_POINT('',(18.,10.8518846384445,-14.9828768864291));
#63547=CARTESIAN_POINT('Origin',(18.,11.145178817862,-15.3878195049812));
#63548=CARTESIAN_POINT('',(18.,-10.8518846384445,-14.9828768864291));
#63549=CARTESIAN_POINT('Origin',(18.,0.,0.));
#63550=CARTESIAN_POINT('',(18.,-11.4987322084552,-15.034266114388));
#63551=CARTESIAN_POINT('Origin',(18.,-11.145178817862,-15.3878195049812));
#63552=CARTESIAN_POINT('',(18.,-10.8187337521542,-14.3542676580869));
#63553=CARTESIAN_POINT('',(18.,-0.501524163602491,-4.0370580695352));
#63554=CARTESIAN_POINT('',(18.,-14.3542676580869,-10.8187337521542));
#63555=CARTESIAN_POINT('',(18.,-7.07761722863737,-18.0953841816037));
#63556=CARTESIAN_POINT('',(18.,-15.034266114388,-11.4987322084552));
#63557=CARTESIAN_POINT('',(18.,-3.61279400082328,-0.0772600948905389));
#63558=CARTESIAN_POINT('',(18.,-14.9828768864291,-10.8518846384445));
#63559=CARTESIAN_POINT('Origin',(18.,-15.3878195049812,-11.145178817862));
#63560=CARTESIAN_POINT('',(18.,-18.5,-2.2655965784226E-15));
#63561=CARTESIAN_POINT('Origin',(18.,0.,0.));
#63562=CARTESIAN_POINT('',(18.,-14.9828768864291,10.8518846384445));
#63563=CARTESIAN_POINT('Origin',(18.,0.,0.));
#63564=CARTESIAN_POINT('',(18.,-15.034266114388,11.4987322084552));
#63565=CARTESIAN_POINT('Origin',(18.,-15.3878195049812,11.145178817862));
#63566=CARTESIAN_POINT('',(18.,-14.3542676580869,10.8187337521542));
#63567=CARTESIAN_POINT('',(18.,-4.03705806953519,0.501524163602477));
#63568=CARTESIAN_POINT('',(18.,-10.8187337521542,14.3542676580869));
#63569=CARTESIAN_POINT('',(18.,-8.84538418160373,16.3276172286374));
#63570=CARTESIAN_POINT('',(18.,-11.4987322084552,15.034266114388));
#63571=CARTESIAN_POINT('',(18.,-0.07726009489054,3.61279400082328));
#63572=CARTESIAN_POINT('',(18.,-10.8518846384445,14.9828768864291));
#63573=CARTESIAN_POINT('Origin',(18.,-11.145178817862,15.3878195049812));
#63574=CARTESIAN_POINT('',(18.,10.8518846384445,14.9828768864291));
#63575=CARTESIAN_POINT('Origin',(18.,0.,0.));
#63576=CARTESIAN_POINT('',(18.,11.4987322084552,15.034266114388));
#63577=CARTESIAN_POINT('Origin',(18.,11.145178817862,15.3878195049812));
#63578=CARTESIAN_POINT('',(18.,10.8187337521542,14.3542676580869));
#63579=CARTESIAN_POINT('',(18.,9.75152416360247,13.2870580695352));
#63580=CARTESIAN_POINT('',(18.,14.3542676580869,10.8187337521542));
#63581=CARTESIAN_POINT('',(18.,16.3276172286374,8.84538418160373));
#63582=CARTESIAN_POINT('',(18.,15.034266114388,11.4987322084552));
#63583=CARTESIAN_POINT('',(18.,12.8627940008233,9.32726009489054));
#63584=CARTESIAN_POINT('',(18.,14.9828768864291,10.8518846384445));
#63585=CARTESIAN_POINT('Origin',(18.,15.3878195049812,11.145178817862));
#63586=CARTESIAN_POINT('',(18.,14.9828768864291,-10.8518846384445));
#63587=CARTESIAN_POINT('Origin',(18.,0.,0.));
#63588=CARTESIAN_POINT('',(18.,15.034266114388,-11.4987322084552));
#63589=CARTESIAN_POINT('Origin',(18.,15.3878195049812,-11.145178817862));
#63590=CARTESIAN_POINT('',(18.,14.3542676580869,-10.8187337521542));
#63591=CARTESIAN_POINT('',(18.,13.2870580695352,-9.75152416360247));
#63592=CARTESIAN_POINT('',(18.,18.0953841816037,-7.07761722863736));
#63593=CARTESIAN_POINT('Origin',(20.5,0.,0.));
#63594=CARTESIAN_POINT('',(21.,-1.16341445918999E-15,9.5));
#63595=CARTESIAN_POINT('Origin',(20.5,-1.16341445918999E-15,9.5));
#63596=CARTESIAN_POINT('Origin',(21.,0.,0.));
#63597=CARTESIAN_POINT('Origin',(21.,9.,0.));
#63598=CARTESIAN_POINT('',(21.,14.3542676580869,-10.8187337521542));
#63599=CARTESIAN_POINT('',(21.,14.7292483497821,-11.1937144438494));
#63600=CARTESIAN_POINT('',(21.,10.9120580695352,-7.37652416360247));
#63601=CARTESIAN_POINT('',(21.,14.7292483497821,11.1937144438494));
#63602=CARTESIAN_POINT('Origin',(21.,0.,0.));
#63603=CARTESIAN_POINT('',(21.,14.3542676580869,10.8187337521542));
#63604=CARTESIAN_POINT('',(21.,10.4877940008233,6.95226009489054));
#63605=CARTESIAN_POINT('',(21.,10.8187337521542,14.3542676580869));
#63606=CARTESIAN_POINT('',(21.,13.9526172286374,11.2203841816037));
#63607=CARTESIAN_POINT('',(21.,11.1937144438494,14.7292483497821));
#63608=CARTESIAN_POINT('',(21.,7.37652416360247,10.9120580695352));
#63609=CARTESIAN_POINT('',(21.,-11.1937144438494,14.7292483497821));
#63610=CARTESIAN_POINT('Origin',(21.,0.,0.));
#63611=CARTESIAN_POINT('',(21.,-10.8187337521542,14.3542676580869));
#63612=CARTESIAN_POINT('',(21.,-2.45226009489054,5.98779400082328));
#63613=CARTESIAN_POINT('',(21.,-14.3542676580869,10.8187337521542));
#63614=CARTESIAN_POINT('',(21.,-11.2203841816037,13.9526172286374));
#63615=CARTESIAN_POINT('',(21.,-14.7292483497821,11.1937144438494));
#63616=CARTESIAN_POINT('',(21.,-6.41205806953519,2.87652416360248));
#63617=CARTESIAN_POINT('',(21.,-14.9828768864291,-10.8518846384445));
#63618=CARTESIAN_POINT('Origin',(21.,0.,0.));
#63619=CARTESIAN_POINT('',(21.,-15.034266114388,-11.4987322084552));
#63620=CARTESIAN_POINT('Origin',(21.,-15.3878195049812,-11.145178817862));
#63621=CARTESIAN_POINT('',(21.,-14.3542676580869,-10.8187337521542));
#63622=CARTESIAN_POINT('',(21.,-5.98779400082328,-2.45226009489054));
#63623=CARTESIAN_POINT('',(21.,-10.8187337521542,-14.3542676580869));
#63624=CARTESIAN_POINT('',(21.,-9.45261722863737,-15.7203841816037));
#63625=CARTESIAN_POINT('',(21.,-11.4987322084552,-15.034266114388));
#63626=CARTESIAN_POINT('',(21.,-2.87652416360248,-6.4120580695352));
#63627=CARTESIAN_POINT('',(21.,-10.8518846384445,-14.9828768864291));
#63628=CARTESIAN_POINT('Origin',(21.,-11.145178817862,-15.3878195049812));
#63629=CARTESIAN_POINT('',(21.,11.1937144438493,-14.7292483497821));
#63630=CARTESIAN_POINT('Origin',(21.,0.,0.));
#63631=CARTESIAN_POINT('',(21.,10.8187337521542,-14.3542676580869));
#63632=CARTESIAN_POINT('',(21.,6.95226009489054,-10.4877940008233));
#63633=CARTESIAN_POINT('',(21.,15.7203841816037,-9.45261722863736));
#63634=CARTESIAN_POINT('Origin',(18.5,18.0953841816037,-7.07761722863736));
#63635=CARTESIAN_POINT('',(18.5,14.7078210486802,-11.1722871427475));
#63636=CARTESIAN_POINT('Origin',(18.5,14.3542676580869,-10.8187337521542));
#63637=CARTESIAN_POINT('',(18.5,11.1722871427474,-14.7078210486802));
#63638=CARTESIAN_POINT('',(18.5,18.448937572197,-7.43117061923064));
#63639=CARTESIAN_POINT('Origin',(18.5,10.8187337521542,-14.3542676580869));
#63640=CARTESIAN_POINT('Origin',(8.,14.7078210486802,-11.1722871427475));
#63641=CARTESIAN_POINT('',(20.5,14.7078210486802,-11.1722871427475));
#63642=CARTESIAN_POINT('',(8.,14.7078210486802,-11.1722871427475));
#63643=CARTESIAN_POINT('',(20.5,11.1722871427474,-14.7078210486802));
#63644=CARTESIAN_POINT('',(20.5,16.073937572197,-9.80617061923064));
#63645=CARTESIAN_POINT('',(8.,11.1722871427474,-14.7078210486802));
#63646=CARTESIAN_POINT('Origin',(20.5,15.7203841816037,-9.45261722863736));
#63647=CARTESIAN_POINT('Origin',(20.5,10.8187337521542,-14.3542676580869));
#63648=CARTESIAN_POINT('Origin',(20.5,14.3542676580869,-10.8187337521542));
#63649=CARTESIAN_POINT('Origin',(18.5,16.3276172286374,8.84538418160373));
#63650=CARTESIAN_POINT('',(18.5,11.1722871427475,14.7078210486802));
#63651=CARTESIAN_POINT('Origin',(18.5,10.8187337521542,14.3542676580869));
#63652=CARTESIAN_POINT('',(18.5,14.7078210486802,11.1722871427475));
#63653=CARTESIAN_POINT('',(18.5,16.6811706192306,9.19893757219701));
#63654=CARTESIAN_POINT('Origin',(18.5,14.3542676580869,10.8187337521542));
#63655=CARTESIAN_POINT('Origin',(8.,11.1722871427475,14.7078210486802));
#63656=CARTESIAN_POINT('',(20.5,11.1722871427475,14.7078210486802));
#63657=CARTESIAN_POINT('',(8.,11.1722871427475,14.7078210486802));
#63658=CARTESIAN_POINT('',(20.5,14.7078210486802,11.1722871427475));
#63659=CARTESIAN_POINT('',(20.5,14.3061706192306,11.573937572197));
#63660=CARTESIAN_POINT('',(8.,14.7078210486802,11.1722871427475));
#63661=CARTESIAN_POINT('Origin',(20.5,13.9526172286374,11.2203841816037));
#63662=CARTESIAN_POINT('Origin',(20.5,14.3542676580869,10.8187337521542));
#63663=CARTESIAN_POINT('Origin',(20.5,10.8187337521542,14.3542676580869));
#63664=CARTESIAN_POINT('Origin',(18.5,-8.84538418160373,16.3276172286374));
#63665=CARTESIAN_POINT('',(18.5,-14.7078210486802,11.1722871427475));
#63666=CARTESIAN_POINT('Origin',(18.5,-14.3542676580869,10.8187337521542));
#63667=CARTESIAN_POINT('',(18.5,-11.1722871427475,14.7078210486802));
#63668=CARTESIAN_POINT('',(18.5,-9.198937572197,16.6811706192306));
#63669=CARTESIAN_POINT('Origin',(18.5,-10.8187337521542,14.3542676580869));
#63670=CARTESIAN_POINT('Origin',(8.,-14.7078210486802,11.1722871427475));
#63671=CARTESIAN_POINT('',(20.5,-14.7078210486802,11.1722871427475));
#63672=CARTESIAN_POINT('',(8.,-14.7078210486802,11.1722871427475));
#63673=CARTESIAN_POINT('',(20.5,-11.1722871427475,14.7078210486802));
#63674=CARTESIAN_POINT('',(20.5,-11.573937572197,14.3061706192306));
#63675=CARTESIAN_POINT('',(8.,-11.1722871427475,14.7078210486802));
#63676=CARTESIAN_POINT('Origin',(20.5,-11.2203841816037,13.9526172286374));
#63677=CARTESIAN_POINT('Origin',(20.5,-10.8187337521542,14.3542676580869));
#63678=CARTESIAN_POINT('Origin',(20.5,-14.3542676580869,10.8187337521542));
#63679=CARTESIAN_POINT('Origin',(-6.,0.,0.));
#63680=CARTESIAN_POINT('',(-6.5,-19.8947609985231,4.00000000022632));
#63681=CARTESIAN_POINT('',(-6.35355339174144,-20.2413779209503,4.0696900904913));
#63682=CARTESIAN_POINT('Origin',(-6.,-19.8947609985231,4.00000000022632));
#63683=CARTESIAN_POINT('',(-6.35355339174133,-4.06969009049129,20.2413779209503));
#63684=CARTESIAN_POINT('Origin',(-6.35355339059327,0.,0.));
#63685=CARTESIAN_POINT('',(-6.5,-4.,19.8947609985686));
#63686=CARTESIAN_POINT('Origin',(-6.,-4.0000000002263,19.8947609985231));
#63687=CARTESIAN_POINT('Origin',(-6.5,0.,0.));
#63688=CARTESIAN_POINT('Origin',(-6.,-4.,19.8947609985686));
#63689=CARTESIAN_POINT('',(-5.99999999557354,-3.5,19.8947610075986));
#63690=CARTESIAN_POINT('Origin',(-6.,-4.,19.8947609985686));
#63691=CARTESIAN_POINT('Origin',(-6.,-4.,19.8947609985686));
#63692=CARTESIAN_POINT('Origin',(-6.,1.25,4.));
#63693=CARTESIAN_POINT('',(-5.99999999549636,-19.8947610077561,3.5));
#63694=CARTESIAN_POINT('Origin',(-6.,-19.8947610077561,4.));
#63695=CARTESIAN_POINT('',(-6.5,-18.5741756210067,4.));
#63696=CARTESIAN_POINT('',(-6.5,1.25,4.));
#63697=CARTESIAN_POINT('',(-6.,-18.5741756210067,3.5));
#63698=CARTESIAN_POINT('Origin',(-6.,-18.5741756210067,4.));
#63699=CARTESIAN_POINT('',(-6.,1.25,3.5));
#63700=CARTESIAN_POINT('Origin',(-6.,-18.5741756210067,4.00000000000001));
#63701=CARTESIAN_POINT('',(-6.,-18.0853815257171,3.89473684210527));
#63702=CARTESIAN_POINT('Origin',(-6.,-18.5741756210067,4.00000000000001));
#63703=CARTESIAN_POINT('Origin',(-6.,-18.5741756210067,4.));
#63704=CARTESIAN_POINT('Origin',(-6.00000000002274,-19.8947609985454,4.));
#63705=CARTESIAN_POINT('Origin',(-6.00000000002274,-19.8947609985454,4.));
#63706=CARTESIAN_POINT('Origin',(-6.,-4.,10.75));
#63707=CARTESIAN_POINT('',(-6.,-3.5,18.5741756210067));
#63708=CARTESIAN_POINT('',(-6.,-3.5,10.75));
#63709=CARTESIAN_POINT('',(-6.5,-4.,18.5741756210067));
#63710=CARTESIAN_POINT('Origin',(-6.,-4.,18.5741756210067));
#63711=CARTESIAN_POINT('',(-6.5,-4.,10.75));
#63712=CARTESIAN_POINT('Ctrl Pts',(-6.3535533914602,-4.06969009037718,20.2413779206745));
#63713=CARTESIAN_POINT('Ctrl Pts',(-6.28452498011738,-4.0694530322025,20.3118353849912));
#63714=CARTESIAN_POINT('Ctrl Pts',(-6.21548931122258,-4.06921836800461,
20.3822849965481));
#63715=CARTESIAN_POINT('Ctrl Pts',(-6.14644660940672,-4.06898602743283,
20.4527269996664));
#63716=CARTESIAN_POINT('Ctrl Pts',(-6.36166082255246,-3.98902655650089,
20.2493262896997));
#63717=CARTESIAN_POINT('Ctrl Pts',(-6.29260192814692,-3.98880661885721,
20.3197549728352));
#63718=CARTESIAN_POINT('Ctrl Pts',(-6.22353638113495,-3.98858899315046,
20.3901763349667));
#63719=CARTESIAN_POINT('Ctrl Pts',(-6.15446386581863,-3.98837349192522,
20.4605901563));
#63720=CARTESIAN_POINT('Ctrl Pts',(-6.34907271559258,-3.82240661064016,
20.2369851525001));
#63721=CARTESIAN_POINT('Ctrl Pts',(-6.2799695713994,-3.82224326499387,20.3073687547676));
#63722=CARTESIAN_POINT('Ctrl Pts',(-6.21086028406924,-3.82208099151617,
20.3777455503893));
#63723=CARTESIAN_POINT('Ctrl Pts',(-6.14174450682076,-3.82192100742865,
20.4481152762486));
#63724=CARTESIAN_POINT('Ctrl Pts',(-6.23193279948825,-3.5782931243035,20.1221434387457));
#63725=CARTESIAN_POINT('Ctrl Pts',(-6.16282464783201,-3.57824724809786,
20.1925063334978));
#63726=CARTESIAN_POINT('Ctrl Pts',(-6.09371017517293,-3.57820215914787,
20.2628625082749));
#63727=CARTESIAN_POINT('Ctrl Pts',(-6.02458951791509,-3.57815724852431,
20.3332121247398));
#63728=CARTESIAN_POINT('Ctrl Pts',(-6.08725162138116,-3.5,19.9803008030806));
#63729=CARTESIAN_POINT('Ctrl Pts',(-6.01819267795923,-3.50000086638446,
20.0506924552528));
#63730=CARTESIAN_POINT('Ctrl Pts',(-5.94912751000377,-3.49999915309731,
20.1210777460986));
#63731=CARTESIAN_POINT('Ctrl Pts',(-5.88005496058486,-3.5,20.1914556678078));
#63732=CARTESIAN_POINT('Ctrl Pts',(-6.00000000086693,-3.5,19.8947609976843));
#63733=CARTESIAN_POINT('Ctrl Pts',(-5.9309715895241,-3.5,19.9651707995687));
#63734=CARTESIAN_POINT('Ctrl Pts',(-5.8619359206293,-3.5,20.0355734829672));
#63735=CARTESIAN_POINT('Ctrl Pts',(-5.79289321881344,-3.5,20.1059692628831));
#63736=CARTESIAN_POINT('',(-6.14644660940672,-4.06898602743283,20.4527269996663));
#63737=CARTESIAN_POINT('Ctrl Pts',(-6.3535533914602,-4.06969009037718,20.2413779206745));
#63738=CARTESIAN_POINT('Ctrl Pts',(-6.28452498011738,-4.0694530322025,20.3118353849912));
#63739=CARTESIAN_POINT('Ctrl Pts',(-6.21548931122258,-4.06921836800461,
20.3822849965481));
#63740=CARTESIAN_POINT('Ctrl Pts',(-6.14644660940672,-4.06898602743283,
20.4527269996664));
#63741=CARTESIAN_POINT('',(-5.79289321881344,-3.5,20.1059692628831));
#63742=CARTESIAN_POINT('Origin',(-5.79289321881344,-4.,20.1059692628831));
#63743=CARTESIAN_POINT('Ctrl Pts',(-5.79289321881344,-3.5,20.1059692628831));
#63744=CARTESIAN_POINT('Ctrl Pts',(-5.86193591811196,-3.5,20.0355734855339));
#63745=CARTESIAN_POINT('Ctrl Pts',(-5.93097158448994,-3.5,19.9651708047025));
#63746=CARTESIAN_POINT('Ctrl Pts',(-5.99999999331647,-3.5,19.8947610053858));
#63747=CARTESIAN_POINT('Origin',(-6.25,0.,0.));
#63748=CARTESIAN_POINT('',(-6.14644660940672,-20.4527269996663,4.06898602743284));
#63749=CARTESIAN_POINT('Ctrl Pts',(-6.14644660940672,-20.4527269996663,
4.06898602743284));
#63750=CARTESIAN_POINT('Ctrl Pts',(-6.21548931371643,-20.3822849940037,
4.06921836801301));
#63751=CARTESIAN_POINT('Ctrl Pts',(-6.28452498219244,-20.3118353828732,
4.06945303220963));
#63752=CARTESIAN_POINT('Ctrl Pts',(-6.35355339146028,-20.2413779206745,
4.06969009037718));
#63753=CARTESIAN_POINT('Origin',(-6.14644660940672,-1.11022302462516E-15,
-1.11022302462516E-15));
#63754=CARTESIAN_POINT('Ctrl Pts',(-6.000000000867,-19.8947609976842,3.5));
#63755=CARTESIAN_POINT('Ctrl Pts',(-5.93097159159917,-19.9651707974521,
3.5));
#63756=CARTESIAN_POINT('Ctrl Pts',(-5.86193592312316,-20.0355734804245,
3.5));
#63757=CARTESIAN_POINT('Ctrl Pts',(-5.79289321881345,-20.1059692628831,
3.5));
#63758=CARTESIAN_POINT('Ctrl Pts',(-6.05816774787649,-19.9517875346151,
3.5));
#63759=CARTESIAN_POINT('Ctrl Pts',(-5.98911910175446,-20.0221853405778,
3.50000009695088));
#63760=CARTESIAN_POINT('Ctrl Pts',(-5.92006353441284,-20.0925762189771,
3.49999990514108));
#63761=CARTESIAN_POINT('Ctrl Pts',(-5.85100104666106,-20.1629601994995,
3.5));
#63762=CARTESIAN_POINT('Ctrl Pts',(-6.17423130885212,-20.0655740105676,
3.54067994796965));
#63763=CARTESIAN_POINT('Ctrl Pts',(-6.10514245467535,-20.1359480599334,
3.5406567970824));
#63764=CARTESIAN_POINT('Ctrl Pts',(-6.03604760619308,-20.2063157855124,
3.5406339242176));
#63765=CARTESIAN_POINT('Ctrl Pts',(-5.96694581109642,-20.2766763882766,
3.5406112586698));
#63766=CARTESIAN_POINT('Ctrl Pts',(-6.33051862773969,-20.2187950827352,
3.73714712174979));
#63767=CARTESIAN_POINT('Ctrl Pts',(-6.26140157368465,-20.2891625274127,
3.73702083787885));
#63768=CARTESIAN_POINT('Ctrl Pts',(-6.19227807841401,-20.359522954417,3.73689570997189));
#63769=CARTESIAN_POINT('Ctrl Pts',(-6.12314870346812,-20.4298769030473,
3.73677204602557));
#63770=CARTESIAN_POINT('Ctrl Pts',(-6.36571453809866,-20.2533004742123,
3.94869478956275));
#63771=CARTESIAN_POINT('Ctrl Pts',(-6.29663981942388,-20.3237142523843,
3.94848324312937));
#63772=CARTESIAN_POINT('Ctrl Pts',(-6.22756048974816,-20.394122502803,3.94827446993852));
#63773=CARTESIAN_POINT('Ctrl Pts',(-6.1584724940246,-20.4645217346169,3.94806722417142));
#63774=CARTESIAN_POINT('Ctrl Pts',(-6.35355339146028,-20.2413779206745,
4.06969009037718));
#63775=CARTESIAN_POINT('Ctrl Pts',(-6.28452498219244,-20.3118353828732,
4.06945303220963));
#63776=CARTESIAN_POINT('Ctrl Pts',(-6.21548931371643,-20.3822849940037,
4.06921836801301));
#63777=CARTESIAN_POINT('Ctrl Pts',(-6.14644660940672,-20.4527269996663,
4.06898602743284));
#63778=CARTESIAN_POINT('',(-5.79289321881345,-20.1059692628831,3.5));
#63779=CARTESIAN_POINT('Ctrl Pts',(-5.99999999319992,-19.8947610055047,
3.5));
#63780=CARTESIAN_POINT('Ctrl Pts',(-5.93097158648724,-19.9651708026652,
3.5));
#63781=CARTESIAN_POINT('Ctrl Pts',(-5.86193592056693,-20.0355734830308,
3.5));
#63782=CARTESIAN_POINT('Ctrl Pts',(-5.79289321881345,-20.1059692628831,
3.5));
#63783=CARTESIAN_POINT('Origin',(-5.79289321881345,-20.1059692628831,4.));
#63784=CARTESIAN_POINT('Origin',(-6.5,-18.,3.5));
#63785=CARTESIAN_POINT('',(-2.49011275698595,-18.5741756210067,3.5));
#63786=CARTESIAN_POINT('',(5.75,-18.5741756210067,3.5));
#63787=CARTESIAN_POINT('',(-2.5,-18.6748493969831,3.5));
#63788=CARTESIAN_POINT('Ctrl Pts',(-2.5,-18.6748493969831,3.5));
#63789=CARTESIAN_POINT('Ctrl Pts',(-2.5,-18.643018830074,3.5));
#63790=CARTESIAN_POINT('Ctrl Pts',(-2.49686768006346,-18.608225302467,3.5));
#63791=CARTESIAN_POINT('Ctrl Pts',(-2.49011275698578,-18.5741756210058,
3.5));
#63792=CARTESIAN_POINT('',(-2.5,-20.1059692628831,3.5));
#63793=CARTESIAN_POINT('',(-2.5,-18.,3.5));
#63794=CARTESIAN_POINT('',(11.6,-20.1059692628831,3.5));
#63795=CARTESIAN_POINT('Origin',(11.6,-20.1059692628831,4.));
#63796=CARTESIAN_POINT('',(-2.,-20.5963587570998,4.09756097560976));
#63797=CARTESIAN_POINT('',(-2.5,-20.1975426238546,3.50845720475184));
#63798=CARTESIAN_POINT('Ctrl Pts',(-2.,-20.5963587570998,4.09756097560976));
#63799=CARTESIAN_POINT('Ctrl Pts',(-2.0007819915549,-20.5965131903849,4.09678471788856));
#63800=CARTESIAN_POINT('Ctrl Pts',(-2.00156398410941,-20.5966657807117,
4.09600809248874));
#63801=CARTESIAN_POINT('Ctrl Pts',(-2.05717822849771,-20.6073867069003,
4.04074949570648));
#63802=CARTESIAN_POINT('Ctrl Pts',(-2.11233881531681,-20.6089573942057,
3.98414057845334));
#63803=CARTESIAN_POINT('Ctrl Pts',(-2.21839474851504,-20.5925290379239,
3.87165457010946));
#63804=CARTESIAN_POINT('Ctrl Pts',(-2.2700758750267,-20.5745079871765,3.81496483783112));
#63805=CARTESIAN_POINT('Ctrl Pts',(-2.3578137004182,-20.5197688252063,3.71434799515287));
#63806=CARTESIAN_POINT('Ctrl Pts',(-2.39549276964077,-20.4855489795038,
3.66919971187174));
#63807=CARTESIAN_POINT('Ctrl Pts',(-2.45004388530638,-20.4077033015026,
3.59868523815613));
#63808=CARTESIAN_POINT('Ctrl Pts',(-2.46954638452372,-20.3681432457135,
3.57134136668746));
#63809=CARTESIAN_POINT('Ctrl Pts',(-2.49393578234053,-20.2839850074225,
3.53073227474396));
#63810=CARTESIAN_POINT('Ctrl Pts',(-2.49999999999998,-20.2417646390697,
3.51669567066231));
#63811=CARTESIAN_POINT('Ctrl Pts',(-2.5,-20.1975426238548,3.50845720475187));
#63812=CARTESIAN_POINT('',(-5.79289321881345,-20.5963587570998,4.09756097560976));
#63813=CARTESIAN_POINT('',(11.6,-20.5963587570998,4.09756097560976));
#63814=CARTESIAN_POINT('Origin',(-5.79289321881345,-20.1059692628831,4.));
#63815=CARTESIAN_POINT('Origin',(-2.5,-20.1059692628831,4.));
#63816=CARTESIAN_POINT('Origin',(-5.79289321881345,-20.1059692628831,4.));
#63817=CARTESIAN_POINT('Origin',(-5.79289321881345,-20.1059692628831,4.));
#63818=CARTESIAN_POINT('Origin',(-6.5,20.5,0.));
#63819=CARTESIAN_POINT('Origin',(-6.5,0.,0.));
#63820=CARTESIAN_POINT('Origin',(-5.79289321881345,0.,0.));
#63821=CARTESIAN_POINT('',(-5.79289321881344,-4.09756097560975,20.5963587570998));
#63822=CARTESIAN_POINT('Origin',(-5.79289321881345,0.,0.));
#63823=CARTESIAN_POINT('Origin',(-5.79289321881344,-4.,20.1059692628831));
#63824=CARTESIAN_POINT('Origin',(11.6,0.,0.));
#63825=CARTESIAN_POINT('',(28.9928932188134,-21.,-2.57175827820944E-15));
#63826=CARTESIAN_POINT('',(28.9928932188134,-2.57175827820944E-15,21.));
#63827=CARTESIAN_POINT('Origin',(28.9928932188134,0.,0.));
#63828=CARTESIAN_POINT('',(-2.,-21.,-2.57175827820944E-15));
#63829=CARTESIAN_POINT('',(11.6,-21.,-2.57175827820944E-15));
#63830=CARTESIAN_POINT('',(-2.,-20.5963587570998,-4.09756097560975));
#63831=CARTESIAN_POINT('Origin',(-2.,0.,0.));
#63832=CARTESIAN_POINT('',(-6.,-20.5963587570998,-4.09756097560975));
#63833=CARTESIAN_POINT('',(11.6,-20.5963587570998,-4.09756097560975));
#63834=CARTESIAN_POINT('',(-6.,-4.09756097560976,-20.5963587570998));
#63835=CARTESIAN_POINT('Origin',(-6.,0.,0.));
#63836=CARTESIAN_POINT('',(-2.,-4.09756097560976,-20.5963587570998));
#63837=CARTESIAN_POINT('',(11.6,-4.09756097560976,-20.5963587570998));
#63838=CARTESIAN_POINT('',(-2.,4.09756097560975,-20.5963587570998));
#63839=CARTESIAN_POINT('Origin',(-2.,0.,0.));
#63840=CARTESIAN_POINT('',(-5.79289321881345,4.09756097560975,-20.5963587570998));
#63841=CARTESIAN_POINT('',(11.6,4.09756097560975,-20.5963587570998));
#63842=CARTESIAN_POINT('',(-5.79289321881345,20.5963587570998,-4.09756097560975));
#63843=CARTESIAN_POINT('Origin',(-5.79289321881345,0.,0.));
#63844=CARTESIAN_POINT('',(-2.,20.5963587570998,-4.09756097560975));
#63845=CARTESIAN_POINT('',(11.6,20.5963587570998,-4.09756097560975));
#63846=CARTESIAN_POINT('',(-2.,20.5963587570998,4.09756097560975));
#63847=CARTESIAN_POINT('Origin',(-2.,0.,0.));
#63848=CARTESIAN_POINT('',(-5.79289321881345,20.5963587570998,4.09756097560976));
#63849=CARTESIAN_POINT('',(11.6,20.5963587570998,4.09756097560975));
#63850=CARTESIAN_POINT('',(-5.79289321881345,4.09756097560976,20.5963587570998));
#63851=CARTESIAN_POINT('Origin',(-5.79289321881345,0.,0.));
#63852=CARTESIAN_POINT('',(-2.,4.09756097560976,20.5963587570998));
#63853=CARTESIAN_POINT('',(11.6,4.09756097560976,20.5963587570998));
#63854=CARTESIAN_POINT('',(-2.,-4.09756097560976,20.5963587570998));
#63855=CARTESIAN_POINT('Origin',(-2.,0.,0.));
#63856=CARTESIAN_POINT('',(11.6,-4.09756097560975,20.5963587570998));
#63857=CARTESIAN_POINT('Origin',(-2.,0.,0.));
#63858=CARTESIAN_POINT('Origin',(28.9928932188134,0.,0.));
#63859=CARTESIAN_POINT('Origin',(11.6,20.1059692628831,4.));
#63860=CARTESIAN_POINT('',(-2.5,20.1975426238546,3.50845720475184));
#63861=CARTESIAN_POINT('',(-2.5,20.1059692628831,3.5));
#63862=CARTESIAN_POINT('Origin',(-2.5,20.1059692628831,4.));
#63863=CARTESIAN_POINT('',(-5.79289321881345,20.1059692628831,3.5));
#63864=CARTESIAN_POINT('',(11.6,20.1059692628831,3.5));
#63865=CARTESIAN_POINT('Origin',(-5.79289321881345,20.1059692628831,4.));
#63866=CARTESIAN_POINT('Ctrl Pts',(-2.5,20.1975426238546,3.50845720475184));
#63867=CARTESIAN_POINT('Ctrl Pts',(-2.5,20.2417646390367,3.51669567065614));
#63868=CARTESIAN_POINT('Ctrl Pts',(-2.49393578234954,20.2839850073609,3.5307322747233));
#63869=CARTESIAN_POINT('Ctrl Pts',(-2.46954638455826,20.3681432456292,3.5713413666364));
#63870=CARTESIAN_POINT('Ctrl Pts',(-2.45004388535121,20.4077033014208,3.59868523809492));
#63871=CARTESIAN_POINT('Ctrl Pts',(-2.39549276970982,20.4855489794284,3.66919971178668));
#63872=CARTESIAN_POINT('Ctrl Pts',(-2.35781370050222,20.5197688251367,3.71434799505337));
#63873=CARTESIAN_POINT('Ctrl Pts',(-2.27007587511498,20.5745079871413,3.81496483773348));
#63874=CARTESIAN_POINT('Ctrl Pts',(-2.21839474858771,20.5925290379056,3.87165457003106));
#63875=CARTESIAN_POINT('Ctrl Pts',(-2.11233881535515,20.6089573942069,3.98414057841399));
#63876=CARTESIAN_POINT('Ctrl Pts',(-2.05717822853915,20.6073867068998,4.04074949570797));
#63877=CARTESIAN_POINT('Ctrl Pts',(-2.00156398410875,20.5966657807121,4.09600809248684));
#63878=CARTESIAN_POINT('Ctrl Pts',(-2.00078199155489,20.5965131903849,4.09678471788857));
#63879=CARTESIAN_POINT('Ctrl Pts',(-2.,20.5963587570998,4.09756097560976));
#63880=CARTESIAN_POINT('Origin',(-5.79289321881345,20.1059692628831,4.));
#63881=CARTESIAN_POINT('',(-6.14644660940673,20.4527269996663,4.06898602743283));
#63882=CARTESIAN_POINT('Origin',(-5.79289321881345,20.1059692628831,4.));
#63883=CARTESIAN_POINT('Origin',(-5.79289321881345,20.1059692628831,4.));
#63884=CARTESIAN_POINT('Origin',(-6.,19.8947609985686,4.));
#63885=CARTESIAN_POINT('',(-6.35355339059328,20.2413779215594,4.0696900903742));
#63886=CARTESIAN_POINT('',(-6.,19.8947609985686,3.5));
#63887=CARTESIAN_POINT('Origin',(-6.,19.8947609985686,4.));
#63888=CARTESIAN_POINT('',(-6.5,19.8947609985686,4.));
#63889=CARTESIAN_POINT('Origin',(-6.,19.8947609985686,4.));
#63890=CARTESIAN_POINT('Origin',(-6.,19.8947609985686,4.));
#63891=CARTESIAN_POINT('Ctrl Pts',(-6.35355339059328,20.2413779215594,4.0696900903742));
#63892=CARTESIAN_POINT('Ctrl Pts',(-6.28452498165401,20.3118353834226,4.0694530322078));
#63893=CARTESIAN_POINT('Ctrl Pts',(-6.21548931347971,20.3822849942452,4.06921836801221));
#63894=CARTESIAN_POINT('Ctrl Pts',(-6.14644660940673,20.4527269996663,4.06898602743283));
#63895=CARTESIAN_POINT('Ctrl Pts',(-6.36166082168515,20.2493262905843,3.98902655649813));
#63896=CARTESIAN_POINT('Ctrl Pts',(-6.29260192968424,20.3197549712672,3.98880661886213));
#63897=CARTESIAN_POINT('Ctrl Pts',(-6.22353638339306,20.3901763326647,3.98858899315751));
#63898=CARTESIAN_POINT('Ctrl Pts',(-6.15446386581864,20.4605901563,3.98837349192522));
#63899=CARTESIAN_POINT('Ctrl Pts',(-6.34907271472472,20.2369851533841,3.8224066106381));
#63900=CARTESIAN_POINT('Ctrl Pts',(-6.27996957293771,20.3073687532007,3.82224326499752));
#63901=CARTESIAN_POINT('Ctrl Pts',(-6.21086028632876,20.3777455480888,3.82208099152141));
#63902=CARTESIAN_POINT('Ctrl Pts',(-6.14174450682077,20.4481152762486,3.82192100742866));
#63903=CARTESIAN_POINT('Ctrl Pts',(-6.23193279862033,20.1221434396294,3.57829312430292));
#63904=CARTESIAN_POINT('Ctrl Pts',(-6.16282464937043,20.1925063319313,3.57824724809889));
#63905=CARTESIAN_POINT('Ctrl Pts',(-6.09371017743262,20.2628625059751,3.57820215914935));
#63906=CARTESIAN_POINT('Ctrl Pts',(-6.02458951791509,20.3332121247397,3.57815724852431));
#63907=CARTESIAN_POINT('Ctrl Pts',(-6.08725162051385,19.9803008039646,3.5));
#63908=CARTESIAN_POINT('Ctrl Pts',(-6.01819267949655,20.0506924536857,3.50000086638443));
#63909=CARTESIAN_POINT('Ctrl Pts',(-5.94912751226188,20.1210777437978,3.49999915309729));
#63910=CARTESIAN_POINT('Ctrl Pts',(-5.88005496058487,20.1914556678078,3.5));
#63911=CARTESIAN_POINT('Ctrl Pts',(-6.,19.8947609985686,3.5));
#63912=CARTESIAN_POINT('Ctrl Pts',(-5.93097159106074,19.9651707980012,3.5));
#63913=CARTESIAN_POINT('Ctrl Pts',(-5.86193592288644,20.0355734806659,3.5));
#63914=CARTESIAN_POINT('Ctrl Pts',(-5.79289321881345,20.1059692628831,3.5));
#63915=CARTESIAN_POINT('Ctrl Pts',(-6.35355339059328,20.2413779215594,4.0696900903742));
#63916=CARTESIAN_POINT('Ctrl Pts',(-6.28452498165401,20.3118353834226,4.0694530322078));
#63917=CARTESIAN_POINT('Ctrl Pts',(-6.21548931347971,20.3822849942452,4.06921836801221));
#63918=CARTESIAN_POINT('Ctrl Pts',(-6.14644660940673,20.4527269996663,4.06898602743283));
#63919=CARTESIAN_POINT('Ctrl Pts',(-5.79289321881345,20.1059692628831,3.5));
#63920=CARTESIAN_POINT('Ctrl Pts',(-5.86193592288644,20.0355734806659,3.5));
#63921=CARTESIAN_POINT('Ctrl Pts',(-5.93097159106074,19.9651707980012,3.5));
#63922=CARTESIAN_POINT('Ctrl Pts',(-6.,19.8947609985686,3.5));
#63923=CARTESIAN_POINT('Origin',(-5.79289321881345,0.,0.));
#63924=CARTESIAN_POINT('',(-6.14644665398816,4.06898603193227,20.4527269760436));
#63925=CARTESIAN_POINT('Origin',(-6.14644660940673,1.11022302462516E-15,
0.));
#63926=CARTESIAN_POINT('Origin',(-5.79289321881345,4.,20.1059692628831));
#63927=CARTESIAN_POINT('Origin',(-6.25,0.,0.));
#63928=CARTESIAN_POINT('',(-6.35355339059327,4.0696900903742,20.2413779215594));
#63929=CARTESIAN_POINT('Origin',(-6.35355339059328,1.11022302462516E-15,
0.));
#63930=CARTESIAN_POINT('Ctrl Pts',(-6.14644664306266,4.06898602754609,20.4527269653283));
#63931=CARTESIAN_POINT('Ctrl Pts',(-6.21548933585545,4.06921836808827,20.3822849714111));
#63932=CARTESIAN_POINT('Ctrl Pts',(-6.28452499284272,4.06945303224623,20.3118353720023));
#63933=CARTESIAN_POINT('Ctrl Pts',(-6.35355339059327,4.0696900903742,20.2413779215594));
#63934=CARTESIAN_POINT('Origin',(-6.,0.,0.));
#63935=CARTESIAN_POINT('',(-6.5,4.,19.8947609985686));
#63936=CARTESIAN_POINT('Origin',(-6.5,0.,0.));
#63937=CARTESIAN_POINT('Origin',(-6.,4.,19.8947609985686));
#63938=CARTESIAN_POINT('Origin',(-2.,0.,0.));
#63939=CARTESIAN_POINT('',(-2.5,20.1975426238546,-3.50845720475184));
#63940=CARTESIAN_POINT('Ctrl Pts',(-2.5,20.1975426238546,-3.50845720475184));
#63941=CARTESIAN_POINT('Ctrl Pts',(-2.5,20.2435547744773,-3.51702916902183));
#63942=CARTESIAN_POINT('Ctrl Pts',(-2.49343634644932,20.2873343735479,-3.53186471227266));
#63943=CARTESIAN_POINT('Ctrl Pts',(-2.46720605754511,20.3741519147674,-3.57485564306978));
#63944=CARTESIAN_POINT('Ctrl Pts',(-2.44629528850599,20.414637889374,-3.60381971113445));
#63945=CARTESIAN_POINT('Ctrl Pts',(-2.38730845067544,20.4946845355157,-3.67931541228553));
#63946=CARTESIAN_POINT('Ctrl Pts',(-2.3460988108993,20.529374025357,-3.72819973354602));
#63947=CARTESIAN_POINT('Ctrl Pts',(-2.25735953173236,20.5791609950881,-3.82895180434606));
#63948=CARTESIAN_POINT('Ctrl Pts',(-2.20924193430928,20.5945414427225,-3.88147391652599));
#63949=CARTESIAN_POINT('Ctrl Pts',(-2.10884374679329,20.6088074165326,-3.98771778608995));
#63950=CARTESIAN_POINT('Ctrl Pts',(-2.05580187972944,20.6070466944948,-4.0421021986681));
#63951=CARTESIAN_POINT('Ctrl Pts',(-2.0020305645695,20.5967566605905,-4.09554468173573));
#63952=CARTESIAN_POINT('Ctrl Pts',(-2.00101528119124,20.5965592620908,-4.09655313881285));
#63953=CARTESIAN_POINT('Ctrl Pts',(-2.,20.5963587570998,-4.09756097560975));
#63954=CARTESIAN_POINT('Origin',(-2.5,0.,0.));
#63955=CARTESIAN_POINT('Origin',(-2.5,19.75,0.));
#63956=CARTESIAN_POINT('',(-2.5,20.1059692628831,-3.5));
#63957=CARTESIAN_POINT('Origin',(-2.5,20.1059692628831,-4.));
#63958=CARTESIAN_POINT('',(-2.5,18.6748493969831,-3.5));
#63959=CARTESIAN_POINT('',(-2.5,18.,-3.5));
#63960=CARTESIAN_POINT('',(-2.5,18.6748493969831,3.5));
#63961=CARTESIAN_POINT('Origin',(-2.5,0.,0.));
#63962=CARTESIAN_POINT('',(-2.5,21.5,3.5));
#63963=CARTESIAN_POINT('Origin',(-6.,3.99999999999999,-19.8947609985686));
#63964=CARTESIAN_POINT('',(-6.35355339059327,4.06969009037419,-20.2413779215594));
#63965=CARTESIAN_POINT('',(-6.,3.5,-19.8947609985686));
#63966=CARTESIAN_POINT('Origin',(-6.,3.99999999999999,-19.8947609985686));
#63967=CARTESIAN_POINT('',(-6.5,4.,-19.8947609985686));
#63968=CARTESIAN_POINT('Origin',(-6.,4.,-19.8947609985686));
#63969=CARTESIAN_POINT('Origin',(-6.,3.99999999999999,-19.8947609985686));
#63970=CARTESIAN_POINT('Origin',(-5.79289321881345,0.,0.));
#63971=CARTESIAN_POINT('',(-6.14644660940673,4.06898602743283,-20.4527269996663));
#63972=CARTESIAN_POINT('Origin',(-5.79289321881345,4.,-20.1059692628831));
#63973=CARTESIAN_POINT('',(-6.14644660940673,20.4527269996663,-4.06898602743283));
#63974=CARTESIAN_POINT('Origin',(-6.14644660940673,-1.11022302462516E-15,
-1.11022302462516E-15));
#63975=CARTESIAN_POINT('Origin',(-5.79289321881345,20.1059692628831,-4.));
#63976=CARTESIAN_POINT('Origin',(-5.79289321881345,4.,-20.1059692628831));
#63977=CARTESIAN_POINT('',(-5.79289321881345,3.5,-20.1059692628831));
#63978=CARTESIAN_POINT('Origin',(-5.79289321881345,4.,-20.1059692628831));
#63979=CARTESIAN_POINT('Origin',(-5.79289321881345,4.,-20.1059692628831));
#63980=CARTESIAN_POINT('Origin',(-5.79289321881345,20.1059692628831,-4.));
#63981=CARTESIAN_POINT('',(-5.79289321881345,20.1059692628831,-3.5));
#63982=CARTESIAN_POINT('Origin',(-5.79289321881345,20.1059692628831,-4.));
#63983=CARTESIAN_POINT('Origin',(-5.79289321881345,20.1059692628831,-4.));
#63984=CARTESIAN_POINT('Origin',(-6.,19.8947609985686,-4.));
#63985=CARTESIAN_POINT('',(-6.,19.8947609985686,-3.5));
#63986=CARTESIAN_POINT('',(-6.35355339059327,20.2413779215594,-4.0696900903742));
#63987=CARTESIAN_POINT('Origin',(-6.,19.8947609985686,-4.));
#63988=CARTESIAN_POINT('',(-6.5,19.8947609985686,-4.));
#63989=CARTESIAN_POINT('Origin',(-6.,19.8947609985686,-4.));
#63990=CARTESIAN_POINT('Origin',(-6.,19.8947609985686,-4.));
#63991=CARTESIAN_POINT('Ctrl Pts',(-6.14644660940673,20.4527269996663,-4.06898602743283));
#63992=CARTESIAN_POINT('Ctrl Pts',(-6.21548931338964,20.3822849943371,-4.06921836801191));
#63993=CARTESIAN_POINT('Ctrl Pts',(-6.28452498159193,20.311835383486,-4.06945303220759));
#63994=CARTESIAN_POINT('Ctrl Pts',(-6.35355339059328,20.2413779215594,-4.0696900903742));
#63995=CARTESIAN_POINT('Ctrl Pts',(-6.15446386581864,20.4605901563,-3.98837349192522));
#63996=CARTESIAN_POINT('Ctrl Pts',(-6.22353638330296,20.3901763327566,-3.98858899315722));
#63997=CARTESIAN_POINT('Ctrl Pts',(-6.29260192962212,20.3197549713306,-3.98880661886193));
#63998=CARTESIAN_POINT('Ctrl Pts',(-6.36166082168515,20.2493262905843,-3.98902655649813));
#63999=CARTESIAN_POINT('Ctrl Pts',(-6.14174450682077,20.4481152762486,-3.82192100742866));
#64000=CARTESIAN_POINT('Ctrl Pts',(-6.21086028623859,20.3777455481806,-3.8220809915212));
#64001=CARTESIAN_POINT('Ctrl Pts',(-6.27996957287556,20.307368753264,-3.82224326499737));
#64002=CARTESIAN_POINT('Ctrl Pts',(-6.34907271472472,20.2369851533841,-3.8224066106381));
#64003=CARTESIAN_POINT('Ctrl Pts',(-6.02458951791509,20.3332121247397,-3.57815724852431));
#64004=CARTESIAN_POINT('Ctrl Pts',(-6.09371017734244,20.2628625060668,-3.57820215914929));
#64005=CARTESIAN_POINT('Ctrl Pts',(-6.16282464930827,20.1925063319946,-3.57824724809885));
#64006=CARTESIAN_POINT('Ctrl Pts',(-6.23193279862033,20.1221434396294,-3.57829312430293));
#64007=CARTESIAN_POINT('Ctrl Pts',(-5.88005496058487,20.1914556678078,-3.5));
#64008=CARTESIAN_POINT('Ctrl Pts',(-5.94912751217177,20.1210777438896,-3.49999915309729));
#64009=CARTESIAN_POINT('Ctrl Pts',(-6.01819267943444,20.0506924537491,-3.50000086638443));
#64010=CARTESIAN_POINT('Ctrl Pts',(-6.08725162051385,19.9803008039646,-3.5));
#64011=CARTESIAN_POINT('Ctrl Pts',(-5.79289321881345,20.1059692628831,-3.5));
#64012=CARTESIAN_POINT('Ctrl Pts',(-5.86193592279637,20.0355734807577,-3.5));
#64013=CARTESIAN_POINT('Ctrl Pts',(-5.93097159099865,19.9651707980645,-3.5));
#64014=CARTESIAN_POINT('Ctrl Pts',(-6.,19.8947609985686,-3.5));
#64015=CARTESIAN_POINT('Ctrl Pts',(-6.,19.8947609985686,-3.5));
#64016=CARTESIAN_POINT('Ctrl Pts',(-5.93097159099865,19.9651707980645,-3.5));
#64017=CARTESIAN_POINT('Ctrl Pts',(-5.86193592279637,20.0355734807577,-3.5));
#64018=CARTESIAN_POINT('Ctrl Pts',(-5.79289321881345,20.1059692628831,-3.5));
#64019=CARTESIAN_POINT('Ctrl Pts',(-6.14644660940673,20.4527269996663,-4.06898602743283));
#64020=CARTESIAN_POINT('Ctrl Pts',(-6.21548931338964,20.3822849943371,-4.06921836801191));
#64021=CARTESIAN_POINT('Ctrl Pts',(-6.28452498159193,20.311835383486,-4.06945303220759));
#64022=CARTESIAN_POINT('Ctrl Pts',(-6.35355339059328,20.2413779215594,-4.0696900903742));
#64023=CARTESIAN_POINT('Ctrl Pts',(-6.35355339059328,4.0696900903742,-20.2413779215594));
#64024=CARTESIAN_POINT('Ctrl Pts',(-6.28452498163503,4.06945303220773,-20.311835383442));
#64025=CARTESIAN_POINT('Ctrl Pts',(-6.2154893134119,4.06921836801198,-20.3822849943144));
#64026=CARTESIAN_POINT('Ctrl Pts',(-6.14644660940672,4.06898602743283,-20.4527269996663));
#64027=CARTESIAN_POINT('Ctrl Pts',(-6.36166082168515,3.98902655649812,-20.2493262905843));
#64028=CARTESIAN_POINT('Ctrl Pts',(-6.29260192966524,3.98880661886206,-20.3197549712866));
#64029=CARTESIAN_POINT('Ctrl Pts',(-6.22353638332523,3.98858899315729,-20.3901763327339));
#64030=CARTESIAN_POINT('Ctrl Pts',(-6.15446386581864,3.98837349192522,-20.4605901563));
#64031=CARTESIAN_POINT('Ctrl Pts',(-6.34907271472472,3.8224066106381,-20.2369851533841));
#64032=CARTESIAN_POINT('Ctrl Pts',(-6.2799695729187,3.82224326499747,-20.30736875322));
#64033=CARTESIAN_POINT('Ctrl Pts',(-6.21086028626087,3.82208099152124,-20.3777455481579));
#64034=CARTESIAN_POINT('Ctrl Pts',(-6.14174450682077,3.82192100742865,-20.4481152762486));
#64035=CARTESIAN_POINT('Ctrl Pts',(-6.23193279862032,3.57829312430292,-20.1221434396294));
#64036=CARTESIAN_POINT('Ctrl Pts',(-6.16282464935142,3.57824724809887,-20.1925063319507));
#64037=CARTESIAN_POINT('Ctrl Pts',(-6.09371017736473,3.5782021591493,-20.2628625060442));
#64038=CARTESIAN_POINT('Ctrl Pts',(-6.02458951791509,3.57815724852431,-20.3332121247398));
#64039=CARTESIAN_POINT('Ctrl Pts',(-6.08725162051385,3.5,-19.9803008039646));
#64040=CARTESIAN_POINT('Ctrl Pts',(-6.01819267947756,3.50000086638443,-20.0506924537051));
#64041=CARTESIAN_POINT('Ctrl Pts',(-5.94912751219404,3.49999915309729,-20.121077743867));
#64042=CARTESIAN_POINT('Ctrl Pts',(-5.88005496058487,3.5,-20.1914556678078));
#64043=CARTESIAN_POINT('Ctrl Pts',(-6.,3.5,-19.8947609985686));
#64044=CARTESIAN_POINT('Ctrl Pts',(-5.93097159104175,3.5,-19.9651707980205));
#64045=CARTESIAN_POINT('Ctrl Pts',(-5.86193592281863,3.5,-20.035573480735));
#64046=CARTESIAN_POINT('Ctrl Pts',(-5.79289321881345,3.5,-20.1059692628831));
#64047=CARTESIAN_POINT('Ctrl Pts',(-5.79289321881345,3.5,-20.1059692628831));
#64048=CARTESIAN_POINT('Ctrl Pts',(-5.86193592281863,3.5,-20.035573480735));
#64049=CARTESIAN_POINT('Ctrl Pts',(-5.93097159104175,3.5,-19.9651707980205));
#64050=CARTESIAN_POINT('Ctrl Pts',(-6.,3.5,-19.8947609985686));
#64051=CARTESIAN_POINT('Ctrl Pts',(-6.35355339059328,4.0696900903742,-20.2413779215594));
#64052=CARTESIAN_POINT('Ctrl Pts',(-6.28452498163503,4.06945303220773,-20.311835383442));
#64053=CARTESIAN_POINT('Ctrl Pts',(-6.2154893134119,4.06921836801198,-20.3822849943144));
#64054=CARTESIAN_POINT('Ctrl Pts',(-6.14644660940672,4.06898602743283,-20.4527269996663));
#64055=CARTESIAN_POINT('Origin',(11.6,4.,-20.1059692628831));
#64056=CARTESIAN_POINT('',(-2.5,3.50845720475183,-20.1975426238546));
#64057=CARTESIAN_POINT('Ctrl Pts',(-2.,4.09756097560975,-20.5963587570998));
#64058=CARTESIAN_POINT('Ctrl Pts',(-2.00101528119204,4.09655313881206,-20.596559262091));
#64059=CARTESIAN_POINT('Ctrl Pts',(-2.00203056456928,4.09554468173501,-20.5967566605907));
#64060=CARTESIAN_POINT('Ctrl Pts',(-2.05580187973614,4.0421021986728,-20.6070466944938));
#64061=CARTESIAN_POINT('Ctrl Pts',(-2.10884374679379,3.98771778608941,-20.6088074165326));
#64062=CARTESIAN_POINT('Ctrl Pts',(-2.20924193430949,3.88147391652575,-20.5945414427224));
#64063=CARTESIAN_POINT('Ctrl Pts',(-2.25735953173246,3.82895180434594,-20.579160995088));
#64064=CARTESIAN_POINT('Ctrl Pts',(-2.34609881089932,3.728199733546,-20.529374025357));
#64065=CARTESIAN_POINT('Ctrl Pts',(-2.38730845067544,3.67931541228552,-20.4946845355157));
#64066=CARTESIAN_POINT('Ctrl Pts',(-2.44629528850599,3.60381971113444,-20.414637889374));
#64067=CARTESIAN_POINT('Ctrl Pts',(-2.46720605754511,3.57485564306978,-20.3741519147674));
#64068=CARTESIAN_POINT('Ctrl Pts',(-2.49343634644932,3.53186471227267,-20.2873343735479));
#64069=CARTESIAN_POINT('Ctrl Pts',(-2.5,3.51702916902183,-20.2435547744773));
#64070=CARTESIAN_POINT('Ctrl Pts',(-2.5,3.50845720475183,-20.1975426238546));
#64071=CARTESIAN_POINT('',(-2.5,3.5,-20.1059692628831));
#64072=CARTESIAN_POINT('Origin',(-2.5,4.,-20.1059692628831));
#64073=CARTESIAN_POINT('',(11.6,3.5,-20.1059692628831));
#64074=CARTESIAN_POINT('Origin',(11.6,20.1059692628831,-4.));
#64075=CARTESIAN_POINT('',(11.6,20.1059692628831,-3.5));
#64076=CARTESIAN_POINT('Origin',(-6.5,18.,-3.5));
#64077=CARTESIAN_POINT('',(-6.,18.5741756210067,-3.5));
#64078=CARTESIAN_POINT('',(-6.,19.25,-3.5));
#64079=CARTESIAN_POINT('',(-2.49011275851364,18.5741756287074,-3.5));
#64080=CARTESIAN_POINT('',(5.75,18.5741756210067,-3.5));
#64081=CARTESIAN_POINT('Ctrl Pts',(-2.49011275851347,18.5741756287065,-3.5));
#64082=CARTESIAN_POINT('Ctrl Pts',(-2.49686768056593,18.6082253077097,-3.5));
#64083=CARTESIAN_POINT('Ctrl Pts',(-2.5,18.6430188324712,-3.5));
#64084=CARTESIAN_POINT('Ctrl Pts',(-2.5,18.6748493969831,-3.5));
#64085=CARTESIAN_POINT('Origin',(-6.,19.25,-4.));
#64086=CARTESIAN_POINT('',(-6.5,18.5741756210067,-4.));
#64087=CARTESIAN_POINT('',(-6.5,19.25,-4.));
#64088=CARTESIAN_POINT('Origin',(-6.,18.5741756210067,-4.));
#64089=CARTESIAN_POINT('Origin',(-2.,0.,0.));
#64090=CARTESIAN_POINT('',(-2.5,-20.1975426238546,-3.50845720475183));
#64091=CARTESIAN_POINT('Origin',(-2.5,0.,0.));
#64092=CARTESIAN_POINT('Ctrl Pts',(-2.,-20.5963587570998,-4.09756097560975));
#64093=CARTESIAN_POINT('Ctrl Pts',(-2.00101528119129,-20.5965592620909,
-4.0965531388128));
#64094=CARTESIAN_POINT('Ctrl Pts',(-2.00203056456968,-20.5967566605904,
-4.09554468173651));
#64095=CARTESIAN_POINT('Ctrl Pts',(-2.05580187972316,-20.607046694496,-4.04210219866254));
#64096=CARTESIAN_POINT('Ctrl Pts',(-2.10884374679332,-20.6088074165326,
-3.98771778608992));
#64097=CARTESIAN_POINT('Ctrl Pts',(-2.20924193430925,-20.5945414427225,
-3.88147391652601));
#64098=CARTESIAN_POINT('Ctrl Pts',(-2.25735953173235,-20.5791609950881,
-3.82895180434606));
#64099=CARTESIAN_POINT('Ctrl Pts',(-2.34609881089934,-20.529374025357,-3.72819973354597));
#64100=CARTESIAN_POINT('Ctrl Pts',(-2.38730845067544,-20.4946845355157,
-3.67931541228552));
#64101=CARTESIAN_POINT('Ctrl Pts',(-2.44629528850598,-20.414637889374,-3.60381971113446));
#64102=CARTESIAN_POINT('Ctrl Pts',(-2.46720605754511,-20.3741519147674,
-3.57485564306979));
#64103=CARTESIAN_POINT('Ctrl Pts',(-2.49343634644932,-20.2873343735479,
-3.53186471227267));
#64104=CARTESIAN_POINT('Ctrl Pts',(-2.5,-20.2435547744773,-3.51702916902183));
#64105=CARTESIAN_POINT('Ctrl Pts',(-2.5,-20.1975426238547,-3.50845720475183));
#64106=CARTESIAN_POINT('Origin',(-2.5,-19.75,2.77555756156289E-15));
#64107=CARTESIAN_POINT('',(-2.5,-18.6748493969831,-3.5));
#64108=CARTESIAN_POINT('Origin',(-2.5,0.,0.));
#64109=CARTESIAN_POINT('',(-2.5,-20.1059692628831,-3.5));
#64110=CARTESIAN_POINT('',(-2.5,-21.5,-3.5));
#64111=CARTESIAN_POINT('Origin',(-2.5,-20.1059692628831,-3.99999999999999));
#64112=CARTESIAN_POINT('Origin',(-5.79289321881344,-4.,20.1059692628831));
#64113=CARTESIAN_POINT('Origin',(-5.79289321881344,-4.,20.1059692628831));
#64114=CARTESIAN_POINT('Origin',(-6.,-4.,18.5741756210067));
#64115=CARTESIAN_POINT('',(-6.,-3.89473684210526,18.0853815257171));
#64116=CARTESIAN_POINT('Origin',(-6.,-4.,18.5741756210067));
#64117=CARTESIAN_POINT('Origin',(-6.,-4.,18.5741756210067));
#64118=CARTESIAN_POINT('Origin',(5.75,-4.,18.5741756210067));
#64119=CARTESIAN_POINT('',(-2.49011275698595,-3.5,18.5741756210067));
#64120=CARTESIAN_POINT('',(5.75,-3.5,18.5741756210067));
#64121=CARTESIAN_POINT('',(-2.,-3.89473684210526,18.0853815257171));
#64122=CARTESIAN_POINT('Ctrl Pts',(-2.49011275698595,-3.5,18.5741756210067));
#64123=CARTESIAN_POINT('Ctrl Pts',(-2.48031734397251,-3.5,18.5247996785933));
#64124=CARTESIAN_POINT('Ctrl Pts',(-2.46374257315005,-3.50729593903647,
18.4776012558686));
#64125=CARTESIAN_POINT('Ctrl Pts',(-2.41476836802978,-3.53660915976364,
18.3774000478142));
#64126=CARTESIAN_POINT('Ctrl Pts',(-2.3796567831271,-3.56195342180394,18.3274816176557));
#64127=CARTESIAN_POINT('Ctrl Pts',(-2.29338459766338,-3.62956958867484,
18.232217901755));
#64128=CARTESIAN_POINT('Ctrl Pts',(-2.23978806301794,-3.67485926714063,
18.1898427129628));
#64129=CARTESIAN_POINT('Ctrl Pts',(-2.12593686398508,-3.77570829974231,
18.122961239244));
#64130=CARTESIAN_POINT('Ctrl Pts',(-2.06428277651074,-3.83280835545914,
18.0991128412042));
#64131=CARTESIAN_POINT('Ctrl Pts',(-2.00210742973619,-3.89270461507943,
18.0858224890517));
#64132=CARTESIAN_POINT('Ctrl Pts',(-2.00105371344565,-3.89372038856671,
18.0856004217928));
#64133=CARTESIAN_POINT('Ctrl Pts',(-2.,-3.89473684210526,18.0853815257171));
#64134=CARTESIAN_POINT('',(5.75,-3.89473684210526,18.0853815257171));
#64135=CARTESIAN_POINT('Origin',(-6.5,-3.5,21.5));
#64136=CARTESIAN_POINT('',(-2.5,-3.5,20.1059692628831));
#64137=CARTESIAN_POINT('',(11.6,-3.5,20.1059692628831));
#64138=CARTESIAN_POINT('',(-2.5,-3.5,18.6748493969831));
#64139=CARTESIAN_POINT('',(-2.5,-3.5,21.5));
#64140=CARTESIAN_POINT('Ctrl Pts',(-2.49011275698578,-3.5,18.5741756210058));
#64141=CARTESIAN_POINT('Ctrl Pts',(-2.49686768006346,-3.5,18.608225302467));
#64142=CARTESIAN_POINT('Ctrl Pts',(-2.5,-3.5,18.643018830074));
#64143=CARTESIAN_POINT('Ctrl Pts',(-2.5,-3.5,18.6748493969831));
#64144=CARTESIAN_POINT('Origin',(11.6,-4.,20.1059692628831));
#64145=CARTESIAN_POINT('',(-2.5,-3.50845720475185,20.1975426238546));
#64146=CARTESIAN_POINT('Ctrl Pts',(-2.,-4.09756097560976,20.5963587570998));
#64147=CARTESIAN_POINT('Ctrl Pts',(-2.00105378229977,-4.09651492000783,
20.5965668655651));
#64148=CARTESIAN_POINT('Ctrl Pts',(-2.00210756704266,-4.0954681961015,20.5967716274829));
#64149=CARTESIAN_POINT('Ctrl Pts',(-2.0549061979377,-4.04299001366594,20.6068632667935));
#64150=CARTESIAN_POINT('Ctrl Pts',(-2.10691928575593,-3.98968902087216,
20.6087335302367));
#64151=CARTESIAN_POINT('Ctrl Pts',(-2.20527868202034,-3.88572666709869,
20.5954171359809));
#64152=CARTESIAN_POINT('Ctrl Pts',(-2.25234932765368,-3.83445109616703,
20.5809320554912));
#64153=CARTESIAN_POINT('Ctrl Pts',(-2.34137513158209,-3.73373520421152,
20.5329716863835));
#64154=CARTESIAN_POINT('Ctrl Pts',(-2.38366457683681,-3.68376379464004,
20.4984471810012));
#64155=CARTESIAN_POINT('Ctrl Pts',(-2.44417869145193,-3.60667572573032,
20.4183174732899));
#64156=CARTESIAN_POINT('Ctrl Pts',(-2.46565574270481,-3.57712046761784,
20.377790317302));
#64157=CARTESIAN_POINT('Ctrl Pts',(-2.49271418520348,-3.53326962999165,
20.2909211660461));
#64158=CARTESIAN_POINT('Ctrl Pts',(-2.49963949791362,-3.5180773748747,20.2472123458134));
#64159=CARTESIAN_POINT('Ctrl Pts',(-2.49999544513914,-3.5089131932808,20.1999653820114));
#64160=CARTESIAN_POINT('Ctrl Pts',(-2.5,-3.50868289295355,20.1987540614206));
#64161=CARTESIAN_POINT('Ctrl Pts',(-2.5,-3.50845720475181,20.1975426238545));
#64162=CARTESIAN_POINT('Origin',(-2.5,-4.,20.1059692628831));
#64163=CARTESIAN_POINT('Origin',(-6.,4.,19.8947609985686));
#64164=CARTESIAN_POINT('',(-6.,3.5,19.8947609985686));
#64165=CARTESIAN_POINT('Origin',(-6.,4.,19.8947609985686));
#64166=CARTESIAN_POINT('Origin',(-6.,4.,19.8947609985686));
#64167=CARTESIAN_POINT('Ctrl Pts',(-6.,3.5,19.8947609985686));
#64168=CARTESIAN_POINT('Ctrl Pts',(-5.93097160224944,3.5,19.9651707865886));
#64169=CARTESIAN_POINT('Ctrl Pts',(-5.86193594526217,3.5,20.0355734578471));
#64170=CARTESIAN_POINT('Ctrl Pts',(-5.79289325246939,3.5,20.1059692285676));
#64171=CARTESIAN_POINT('Ctrl Pts',(-6.05816774700923,3.5,19.9517875354993));
#64172=CARTESIAN_POINT('Ctrl Pts',(-5.98911911240786,3.50000009695086,20.0221853297161));
#64173=CARTESIAN_POINT('Ctrl Pts',(-5.92006355655825,3.4999999051411,20.0925761964034));
#64174=CARTESIAN_POINT('Ctrl Pts',(-5.85100108032663,3.5,20.1629601651898));
#64175=CARTESIAN_POINT('Ctrl Pts',(-6.17423130798436,3.54067994796936,20.0655740114515));
#64176=CARTESIAN_POINT('Ctrl Pts',(-6.10514246533496,3.54065679708597,20.1359480490754));
#64177=CARTESIAN_POINT('Ctrl Pts',(-6.03604762835117,3.54063392422494,20.2063157629463));
#64178=CARTESIAN_POINT('Ctrl Pts',(-5.96694584478107,3.54061125868084,20.2766763539781));
#64179=CARTESIAN_POINT('Ctrl Pts',(-6.33051862687158,3.7371471217482,20.218795083619));
#64180=CARTESIAN_POINT('Ctrl Pts',(-6.26140158434861,3.73702083789835,20.2891625165557));
#64181=CARTESIAN_POINT('Ctrl Pts',(-6.19227810058116,3.73689571001199,20.3595229318531));
#64182=CARTESIAN_POINT('Ctrl Pts',(-6.12314873716634,3.73677204608588,20.4298768687522));
#64183=CARTESIAN_POINT('Ctrl Pts',(-6.36571453723109,3.94869478956009,20.2533004750967));
#64184=CARTESIAN_POINT('Ctrl Pts',(-6.29663983008132,3.94848324316203,20.3237142415202));
#64185=CARTESIAN_POINT('Ctrl Pts',(-6.22756051190152,3.94827447000558,20.3941224802241));
#64186=CARTESIAN_POINT('Ctrl Pts',(-6.15847252770227,3.94806722427235,20.4645217002994));
#64187=CARTESIAN_POINT('Ctrl Pts',(-6.35355339059327,4.0696900903742,20.2413779215594));
#64188=CARTESIAN_POINT('Ctrl Pts',(-6.28452499284272,4.06945303224623,20.3118353720023));
#64189=CARTESIAN_POINT('Ctrl Pts',(-6.21548933585545,4.06921836808827,20.3822849714111));
#64190=CARTESIAN_POINT('Ctrl Pts',(-6.14644664306266,4.06898602754609,20.4527269653283));
#64191=CARTESIAN_POINT('',(-5.79289325247318,3.5,20.1059692285637));
#64192=CARTESIAN_POINT('Origin',(-5.79289325247318,4.,20.1059692285637));
#64193=CARTESIAN_POINT('Ctrl Pts',(-6.,3.5,19.8947609985686));
#64194=CARTESIAN_POINT('Ctrl Pts',(-5.93097160224944,3.5,19.9651707865886));
#64195=CARTESIAN_POINT('Ctrl Pts',(-5.86193594526217,3.5,20.0355734578471));
#64196=CARTESIAN_POINT('Ctrl Pts',(-5.79289325246939,3.5,20.1059692285676));
#64197=CARTESIAN_POINT('Origin',(11.6,4.,20.1059692628831));
#64198=CARTESIAN_POINT('Origin',(-5.79289321881345,4.,20.1059692628831));
#64199=CARTESIAN_POINT('',(-2.5,3.5,20.1059692628831));
#64200=CARTESIAN_POINT('',(11.6,3.5,20.1059692628831));
#64201=CARTESIAN_POINT('',(-2.5,3.50845720475185,20.1975426238546));
#64202=CARTESIAN_POINT('Origin',(-2.5,4.,20.1059692628831));
#64203=CARTESIAN_POINT('Ctrl Pts',(-2.5,3.50845720475184,20.1975426238546));
#64204=CARTESIAN_POINT('Ctrl Pts',(-2.5,3.517036693927,20.2435951662777));
#64205=CARTESIAN_POINT('Ctrl Pts',(-2.49342483977402,3.53189060449051,20.287410477654));
#64206=CARTESIAN_POINT('Ctrl Pts',(-2.46710761937579,3.57500889896805,20.3744340358278));
#64207=CARTESIAN_POINT('Ctrl Pts',(-2.44607731612422,3.60411954186725,20.4150481564303));
#64208=CARTESIAN_POINT('Ctrl Pts',(-2.3866307647472,3.68015463370752,20.4954497474577));
#64209=CARTESIAN_POINT('Ctrl Pts',(-2.3450061363464,3.72948787520241,20.5302485483201));
#64210=CARTESIAN_POINT('Ctrl Pts',(-2.2561617458898,3.83026319150449,20.579566056646));
#64211=CARTESIAN_POINT('Ctrl Pts',(-2.20846377743015,3.88230470098185,20.5946909756454));
#64212=CARTESIAN_POINT('Ctrl Pts',(-2.10864661377827,3.98791865791761,20.608794231553));
#64213=CARTESIAN_POINT('Ctrl Pts',(-2.05576282506689,4.04213858560532,20.607026997786));
#64214=CARTESIAN_POINT('Ctrl Pts',(-2.00210756704338,4.09546819610263,20.5967716274827));
#64215=CARTESIAN_POINT('Ctrl Pts',(-2.00105378229923,4.09651492000836,20.596566865565));
#64216=CARTESIAN_POINT('Ctrl Pts',(-2.,4.09756097560976,20.5963587570998));
#64217=CARTESIAN_POINT('Origin',(-2.,0.,0.));
#64218=CARTESIAN_POINT('Origin',(-2.5,0.,0.));
#64219=CARTESIAN_POINT('Origin',(-5.79289321881345,4.,20.1059692628831));
#64220=CARTESIAN_POINT('Origin',(-6.5,3.5,18.));
#64221=CARTESIAN_POINT('',(-6.,3.5,18.5741756210067));
#64222=CARTESIAN_POINT('',(-6.,3.5,9.));
#64223=CARTESIAN_POINT('',(-2.49011275698595,3.5,18.5741756210067));
#64224=CARTESIAN_POINT('',(5.75,3.5,18.5741756210067));
#64225=CARTESIAN_POINT('',(-2.5,3.5,18.6748493969831));
#64226=CARTESIAN_POINT('Ctrl Pts',(-2.5,3.5,18.6748493969831));
#64227=CARTESIAN_POINT('Ctrl Pts',(-2.5,3.5,18.643018830074));
#64228=CARTESIAN_POINT('Ctrl Pts',(-2.49686768006346,3.5,18.608225302467));
#64229=CARTESIAN_POINT('Ctrl Pts',(-2.49011275698578,3.5,18.5741756210058));
#64230=CARTESIAN_POINT('',(-2.5,3.5,18.));
#64231=CARTESIAN_POINT('Origin',(-6.,4.,9.));
#64232=CARTESIAN_POINT('',(-6.5,4.,18.5741756210067));
#64233=CARTESIAN_POINT('',(-6.5,4.,9.));
#64234=CARTESIAN_POINT('Origin',(-6.,4.,18.5741756210067));
#64235=CARTESIAN_POINT('Origin',(-6.5,20.5,0.));
#64236=CARTESIAN_POINT('',(-6.5,18.5741756210067,4.));
#64237=CARTESIAN_POINT('',(-6.5,21.,4.));
#64238=CARTESIAN_POINT('Origin',(-6.5,0.,0.));
#64239=CARTESIAN_POINT('Origin',(-6.,21.,4.));
#64240=CARTESIAN_POINT('',(-6.,18.5741756210067,3.5));
#64241=CARTESIAN_POINT('',(-6.,21.,3.5));
#64242=CARTESIAN_POINT('Origin',(-6.,18.5741756210067,4.));
#64243=CARTESIAN_POINT('Origin',(-6.,18.5741756210067,4.));
#64244=CARTESIAN_POINT('',(-6.,18.0853815257171,3.89473684210526));
#64245=CARTESIAN_POINT('Origin',(-6.,18.5741756210067,4.));
#64246=CARTESIAN_POINT('Origin',(-6.,18.5741756210067,4.));
#64247=CARTESIAN_POINT('Origin',(-2.,0.,0.));
#64248=CARTESIAN_POINT('',(-2.5,-3.50845720475184,-20.1975426238546));
#64249=CARTESIAN_POINT('Ctrl Pts',(-2.5,-3.50845720475184,-20.1975426238546));
#64250=CARTESIAN_POINT('Ctrl Pts',(-2.5,-3.51702916902184,-20.2435547744772));
#64251=CARTESIAN_POINT('Ctrl Pts',(-2.49343634644932,-3.53186471227267,
-20.2873343735479));
#64252=CARTESIAN_POINT('Ctrl Pts',(-2.46720605754511,-3.57485564306979,
-20.3741519147674));
#64253=CARTESIAN_POINT('Ctrl Pts',(-2.44629528850598,-3.60381971113447,
-20.414637889374));
#64254=CARTESIAN_POINT('Ctrl Pts',(-2.38730845067544,-3.67931541228553,
-20.4946845355157));
#64255=CARTESIAN_POINT('Ctrl Pts',(-2.34609881089932,-3.72819973354599,
-20.529374025357));
#64256=CARTESIAN_POINT('Ctrl Pts',(-2.25735953173236,-3.82895180434606,
-20.5791609950881));
#64257=CARTESIAN_POINT('Ctrl Pts',(-2.20924193430928,-3.88147391652601,
-20.5945414427225));
#64258=CARTESIAN_POINT('Ctrl Pts',(-2.10884374679334,-3.98771778608992,
-20.6088074165326));
#64259=CARTESIAN_POINT('Ctrl Pts',(-2.05580187972934,-4.04210219866796,
-20.6070466944948));
#64260=CARTESIAN_POINT('Ctrl Pts',(-2.00203056456934,-4.09554468173591,
-20.5967566605905));
#64261=CARTESIAN_POINT('Ctrl Pts',(-2.00101528119147,-4.09655313881263,
-20.5965592620909));
#64262=CARTESIAN_POINT('Ctrl Pts',(-2.,-4.09756097560976,-20.5963587570998));
#64263=CARTESIAN_POINT('Origin',(-2.5,0.,0.));
#64264=CARTESIAN_POINT('Origin',(-2.5,-3.33066907387547E-15,-19.75));
#64265=CARTESIAN_POINT('',(-2.5,-3.5,-20.1059692628831));
#64266=CARTESIAN_POINT('Origin',(-2.5,-4.,-20.1059692628831));
#64267=CARTESIAN_POINT('',(-2.5,-3.5,-18.6748493969831));
#64268=CARTESIAN_POINT('',(-2.5,-3.5,-18.));
#64269=CARTESIAN_POINT('',(-2.5,3.5,-18.6748493969831));
#64270=CARTESIAN_POINT('Origin',(-2.5,0.,0.));
#64271=CARTESIAN_POINT('',(-2.5,3.5,-21.5));
#64272=CARTESIAN_POINT('Origin',(-2.,0.,0.));
#64273=CARTESIAN_POINT('',(-2.,-3.89473684210527,-18.0853815257171));
#64274=CARTESIAN_POINT('',(-2.49011275851364,-3.5,-18.5741756287074));
#64275=CARTESIAN_POINT('Ctrl Pts',(-2.,-3.89473684210527,-18.0853815257171));
#64276=CARTESIAN_POINT('Ctrl Pts',(-2.00094797695669,-3.89382238615325,
-18.085578456331));
#64277=CARTESIAN_POINT('Ctrl Pts',(-2.00189595598416,-3.89290848084184,
-18.0857779535775));
#64278=CARTESIAN_POINT('Ctrl Pts',(-2.09304035837669,-3.80509320931406,
-18.105205568777));
#64279=CARTESIAN_POINT('Ctrl Pts',(-2.18153986698468,-3.7247983724995,-18.1472832140884));
#64280=CARTESIAN_POINT('Ctrl Pts',(-2.3185279168613,-3.60890246257771,-18.2551075840637));
#64281=CARTESIAN_POINT('Ctrl Pts',(-2.3696986038289,-3.56883721926646,-18.3118008095372));
#64282=CARTESIAN_POINT('Ctrl Pts',(-2.43934686237775,-3.52083652884264,
-18.4222997616512));
#64283=CARTESIAN_POINT('Ctrl Pts',(-2.46399052835428,-3.50656062686055,
-18.4752127841392));
#64284=CARTESIAN_POINT('Ctrl Pts',(-2.48396330014831,-3.50059284622875,
-18.54612986876));
#64285=CARTESIAN_POINT('Ctrl Pts',(-2.48732407582936,-3.49999999978351,
-18.560118656735));
#64286=CARTESIAN_POINT('Ctrl Pts',(-2.49011275851364,-3.5,-18.5741756287074));
#64287=CARTESIAN_POINT('',(-2.,3.89473684210526,-18.0853815257171));
#64288=CARTESIAN_POINT('Origin',(-2.,0.,0.));
#64289=CARTESIAN_POINT('',(-2.49011275851364,3.5,-18.5741756287073));
#64290=CARTESIAN_POINT('Ctrl Pts',(-2.49011275851364,3.5,-18.5741756287073));
#64291=CARTESIAN_POINT('Ctrl Pts',(-2.48732407582936,3.4999999997835,-18.560118656735));
#64292=CARTESIAN_POINT('Ctrl Pts',(-2.48396330014829,3.50059284622874,-18.5461298687599));
#64293=CARTESIAN_POINT('Ctrl Pts',(-2.46399052835424,3.50656062686056,-18.4752127841391));
#64294=CARTESIAN_POINT('Ctrl Pts',(-2.4393468623777,3.52083652884266,-18.4222997616511));
#64295=CARTESIAN_POINT('Ctrl Pts',(-2.36969860382856,3.5688372192667,-18.3118008095367));
#64296=CARTESIAN_POINT('Ctrl Pts',(-2.31852791686079,3.60890246257814,-18.2551075840632));
#64297=CARTESIAN_POINT('Ctrl Pts',(-2.1815398669833,3.72479837250067,-18.1472832140873));
#64298=CARTESIAN_POINT('Ctrl Pts',(-2.09304035837488,3.80509320931587,-18.1052055687765));
#64299=CARTESIAN_POINT('Ctrl Pts',(-2.00189595598381,3.89290848084216,-18.0857779535774));
#64300=CARTESIAN_POINT('Ctrl Pts',(-2.0009479769565,3.89382238615342,-18.0855784563309));
#64301=CARTESIAN_POINT('Ctrl Pts',(-2.,3.89473684210526,-18.0853815257171));
#64302=CARTESIAN_POINT('Ctrl Pts',(-2.5,3.5,-18.6748493969831));
#64303=CARTESIAN_POINT('Ctrl Pts',(-2.5,3.5,-18.6430188324712));
#64304=CARTESIAN_POINT('Ctrl Pts',(-2.49686768056593,3.5,-18.6082253077096));
#64305=CARTESIAN_POINT('Ctrl Pts',(-2.49011275851347,3.5,-18.5741756287065));
#64306=CARTESIAN_POINT('Ctrl Pts',(-2.49011275851347,-3.5,-18.5741756287065));
#64307=CARTESIAN_POINT('Ctrl Pts',(-2.49686768056593,-3.5,-18.6082253077096));
#64308=CARTESIAN_POINT('Ctrl Pts',(-2.5,-3.5,-18.6430188324712));
#64309=CARTESIAN_POINT('Ctrl Pts',(-2.5,-3.5,-18.6748493969831));
#64310=CARTESIAN_POINT('Origin',(-6.,0.,0.));
#64311=CARTESIAN_POINT('',(-6.,3.89473684210526,18.0853815257171));
#64312=CARTESIAN_POINT('Origin',(-6.,0.,0.));
#64313=CARTESIAN_POINT('Origin',(-6.,4.,18.5741756210067));
#64314=CARTESIAN_POINT('Origin',(5.75,18.5741756210067,4.));
#64315=CARTESIAN_POINT('',(-2.49011275698595,18.5741756210067,3.5));
#64316=CARTESIAN_POINT('',(5.75,18.5741756210067,3.5));
#64317=CARTESIAN_POINT('',(-2.,18.0853815257171,3.89473684210526));
#64318=CARTESIAN_POINT('Ctrl Pts',(-2.49011275698595,18.5741756210067,3.5));
#64319=CARTESIAN_POINT('Ctrl Pts',(-2.4803173439725,18.5247996785932,3.5));
#64320=CARTESIAN_POINT('Ctrl Pts',(-2.46374257315002,18.4776012558685,3.5072959390365));
#64321=CARTESIAN_POINT('Ctrl Pts',(-2.41476836802979,18.3774000478142,3.53660915976365));
#64322=CARTESIAN_POINT('Ctrl Pts',(-2.37965678312714,18.3274816176558,3.5619534218039));
#64323=CARTESIAN_POINT('Ctrl Pts',(-2.29338459766337,18.232217901755,3.62956958867484));
#64324=CARTESIAN_POINT('Ctrl Pts',(-2.23978806301794,18.1898427129628,3.67485926714064));
#64325=CARTESIAN_POINT('Ctrl Pts',(-2.12593686398496,18.1229612392439,3.77570829974241));
#64326=CARTESIAN_POINT('Ctrl Pts',(-2.0642827765073,18.0991128412049,3.83280835545585));
#64327=CARTESIAN_POINT('Ctrl Pts',(-2.00210742973639,18.0858224890517,3.89270461507972));
#64328=CARTESIAN_POINT('Ctrl Pts',(-2.00105371344551,18.0856004217928,3.89372038856684));
#64329=CARTESIAN_POINT('Ctrl Pts',(-2.,18.0853815257171,3.89473684210526));
#64330=CARTESIAN_POINT('',(5.75,18.0853815257171,3.89473684210526));
#64331=CARTESIAN_POINT('Origin',(-2.,0.,0.));
#64332=CARTESIAN_POINT('',(-2.,18.0853815257171,-3.89473684210526));
#64333=CARTESIAN_POINT('Ctrl Pts',(-2.,18.0853815257171,-3.89473684210527));
#64334=CARTESIAN_POINT('Ctrl Pts',(-2.00094797695641,18.0855784563309,-3.89382238615351));
#64335=CARTESIAN_POINT('Ctrl Pts',(-2.00189595598414,18.0857779535775,-3.89290848084185));
#64336=CARTESIAN_POINT('Ctrl Pts',(-2.09304035837568,18.1052055687767,-3.80509320931504));
#64337=CARTESIAN_POINT('Ctrl Pts',(-2.1815398669839,18.1472832140878,-3.72479837250016));
#64338=CARTESIAN_POINT('Ctrl Pts',(-2.31852791686109,18.2551075840635,-3.60890246257788));
#64339=CARTESIAN_POINT('Ctrl Pts',(-2.36969860382876,18.311800809537,-3.56883721926657));
#64340=CARTESIAN_POINT('Ctrl Pts',(-2.43934686237771,18.4222997616511,-3.52083652884266));
#64341=CARTESIAN_POINT('Ctrl Pts',(-2.46399052835424,18.4752127841391,-3.50656062686056));
#64342=CARTESIAN_POINT('Ctrl Pts',(-2.48396330014829,18.5461298687599,-3.50059284622875));
#64343=CARTESIAN_POINT('Ctrl Pts',(-2.48732407582936,18.560118656735,-3.4999999997835));
#64344=CARTESIAN_POINT('Ctrl Pts',(-2.49011275851364,18.5741756287074,-3.5));
#64345=CARTESIAN_POINT('Origin',(-2.,0.,0.));
#64346=CARTESIAN_POINT('Ctrl Pts',(-2.49011275698578,18.5741756210058,3.5));
#64347=CARTESIAN_POINT('Ctrl Pts',(-2.49686768006346,18.608225302467,3.5));
#64348=CARTESIAN_POINT('Ctrl Pts',(-2.5,18.643018830074,3.5));
#64349=CARTESIAN_POINT('Ctrl Pts',(-2.5,18.6748493969831,3.5));
#64350=CARTESIAN_POINT('Origin',(-6.,4.,18.5741756210067));
#64351=CARTESIAN_POINT('Origin',(-6.,4.,18.5741756210067));
#64352=CARTESIAN_POINT('Origin',(5.75,4.,18.5741756210067));
#64353=CARTESIAN_POINT('',(-2.,3.89473684210526,18.0853815257171));
#64354=CARTESIAN_POINT('',(5.75,3.89473684210526,18.0853815257171));
#64355=CARTESIAN_POINT('Ctrl Pts',(-2.,3.89473684210526,18.0853815257171));
#64356=CARTESIAN_POINT('Ctrl Pts',(-2.00105371344572,3.89372038856664,18.0856004217929));
#64357=CARTESIAN_POINT('Ctrl Pts',(-2.00210742973654,3.89270461507958,18.0858224890517));
#64358=CARTESIAN_POINT('Ctrl Pts',(-2.09351569465547,3.804646993342,18.1053615522589));
#64359=CARTESIAN_POINT('Ctrl Pts',(-2.18214848766776,3.72425195645496,18.1476027839865));
#64360=CARTESIAN_POINT('Ctrl Pts',(-2.31958013153081,3.60803698471264,18.2560609577767));
#64361=CARTESIAN_POINT('Ctrl Pts',(-2.37098023972695,3.56784861835865,18.3132986190986));
#64362=CARTESIAN_POINT('Ctrl Pts',(-2.44048867507143,3.52013110417152,18.4245257150294));
#64363=CARTESIAN_POINT('Ctrl Pts',(-2.46491477585542,3.50609467152981,18.4775461366035));
#64364=CARTESIAN_POINT('Ctrl Pts',(-2.48434736805698,3.50052662530646,18.5477361044576));
#64365=CARTESIAN_POINT('Ctrl Pts',(-2.48748442178262,3.5,18.5609269169995));
#64366=CARTESIAN_POINT('Ctrl Pts',(-2.49011275698595,3.5,18.5741756210067));
#64367=CARTESIAN_POINT('Origin',(5.75,0.,0.));
#64368=CARTESIAN_POINT('',(7.5,14.9828768864291,-10.8518846384445));
#64369=CARTESIAN_POINT('',(5.75,14.9828768864291,-10.8518846384445));
#64370=CARTESIAN_POINT('',(7.5,14.9828768864291,10.8518846384445));
#64371=CARTESIAN_POINT('',(5.75,14.9828768864291,10.8518846384445));
#64372=CARTESIAN_POINT('',(7.5,10.8518846384445,14.9828768864291));
#64373=CARTESIAN_POINT('Origin',(7.5,0.,0.));
#64374=CARTESIAN_POINT('',(5.75,10.8518846384445,14.9828768864291));
#64375=CARTESIAN_POINT('',(7.5,-10.8518846384445,14.9828768864291));
#64376=CARTESIAN_POINT('',(5.75,-10.8518846384445,14.9828768864291));
#64377=CARTESIAN_POINT('',(7.5,-14.9828768864291,10.8518846384445));
#64378=CARTESIAN_POINT('Origin',(7.5,0.,0.));
#64379=CARTESIAN_POINT('',(5.75,-14.9828768864291,10.8518846384445));
#64380=CARTESIAN_POINT('',(-2.,-18.5,-2.2655965784226E-15));
#64381=CARTESIAN_POINT('',(5.75,-18.5,-2.2655965784226E-15));
#64382=CARTESIAN_POINT('',(-2.,-18.0853815257171,3.89473684210527));
#64383=CARTESIAN_POINT('Origin',(-2.,0.,0.));
#64384=CARTESIAN_POINT('',(5.75,-18.0853815257171,3.89473684210527));
#64385=CARTESIAN_POINT('Origin',(-6.,0.,0.));
#64386=CARTESIAN_POINT('Origin',(-2.,0.,0.));
#64387=CARTESIAN_POINT('',(-6.,18.0853815257171,-3.89473684210526));
#64388=CARTESIAN_POINT('',(5.75,18.0853815257171,-3.89473684210526));
#64389=CARTESIAN_POINT('',(-6.,3.89473684210526,-18.0853815257171));
#64390=CARTESIAN_POINT('Origin',(-6.,0.,0.));
#64391=CARTESIAN_POINT('',(5.75,3.89473684210526,-18.0853815257171));
#64392=CARTESIAN_POINT('',(-6.,-3.89473684210527,-18.0853815257171));
#64393=CARTESIAN_POINT('',(5.75,-3.89473684210527,-18.0853815257171));
#64394=CARTESIAN_POINT('',(-6.,-18.0853815257171,-3.89473684210526));
#64395=CARTESIAN_POINT('Origin',(-6.,0.,0.));
#64396=CARTESIAN_POINT('',(-2.,-18.0853815257171,-3.89473684210526));
#64397=CARTESIAN_POINT('',(5.75,-18.0853815257171,-3.89473684210526));
#64398=CARTESIAN_POINT('Origin',(-2.,0.,0.));
#64399=CARTESIAN_POINT('',(7.5,-14.9828768864291,-10.8518846384445));
#64400=CARTESIAN_POINT('',(5.75,-14.9828768864291,-10.8518846384445));
#64401=CARTESIAN_POINT('',(7.5,-10.8518846384445,-14.9828768864291));
#64402=CARTESIAN_POINT('Origin',(7.5,0.,0.));
#64403=CARTESIAN_POINT('',(5.75,-10.8518846384445,-14.9828768864291));
#64404=CARTESIAN_POINT('',(7.5,10.8518846384445,-14.9828768864291));
#64405=CARTESIAN_POINT('',(5.75,10.8518846384445,-14.9828768864291));
#64406=CARTESIAN_POINT('Origin',(7.5,0.,0.));
#64407=CARTESIAN_POINT('Origin',(5.75,15.3878195049812,-11.145178817862));
#64408=CARTESIAN_POINT('',(7.99471483544825,15.034266114388,-11.4987322084552));
#64409=CARTESIAN_POINT('',(5.75,15.034266114388,-11.4987322084552));
#64410=CARTESIAN_POINT('Ctrl Pts',(7.5,14.9828768864291,-10.8518846384445));
#64411=CARTESIAN_POINT('Ctrl Pts',(7.50105371344594,14.9822669774522,-10.8527267217709));
#64412=CARTESIAN_POINT('Ctrl Pts',(7.50210742973669,14.9816596935127,-10.8535707098414));
#64413=CARTESIAN_POINT('Ctrl Pts',(7.59351569467899,14.9292065753492,-10.9269504763462));
#64414=CARTESIAN_POINT('Ctrl Pts',(7.68214848767697,14.8976245327992,-11.0120989243868));
#64415=CARTESIAN_POINT('Ctrl Pts',(7.81958013152899,14.8836434033438,-11.1704454530317));
#64416=CARTESIAN_POINT('Ctrl Pts',(7.87098023972546,14.8919941158644,-11.2398826207751));
#64417=CARTESIAN_POINT('Ctrl Pts',(7.94048867507039,14.9308215694372,-11.3545161973505));
#64418=CARTESIAN_POINT('Ctrl Pts',(7.96491477585465,14.9558097197837,-11.4033401554803));
#64419=CARTESIAN_POINT('Ctrl Pts',(7.98678347589511,15.0039319604954,-11.466290886942));
#64420=CARTESIAN_POINT('Ctrl Pts',(7.9914773312572,15.0185083904015,-11.4829744844688));
#64421=CARTESIAN_POINT('Ctrl Pts',(7.99471483544825,15.034266114388,-11.4987322084552));
#64422=CARTESIAN_POINT('Origin',(7.5,0.,0.));
#64423=CARTESIAN_POINT('',(7.99471483561597,11.4987322092715,-15.0342661152043));
#64424=CARTESIAN_POINT('Ctrl Pts',(7.99471483561596,11.4987322092715,-15.0342661152043));
#64425=CARTESIAN_POINT('Ctrl Pts',(7.9913625823211,11.4824159731374,-15.0179498789948));
#64426=CARTESIAN_POINT('Ctrl Pts',(7.98645003622193,11.4651126007102,-15.0029056934798));
#64427=CARTESIAN_POINT('Ctrl Pts',(7.96402271105306,11.4013638075407,-14.9546388364281));
#64428=CARTESIAN_POINT('Ctrl Pts',(7.93938632198296,11.3524620624659,-14.9298917928023));
#64429=CARTESIAN_POINT('Ctrl Pts',(7.86974221712864,11.2381679469927,-14.8917374982997));
#64430=CARTESIAN_POINT('Ctrl Pts',(7.81856316470143,11.1692008513045,-14.8836497863542));
#64431=CARTESIAN_POINT('Ctrl Pts',(7.68155929434285,11.0115152525768,-14.8978112789729));
#64432=CARTESIAN_POINT('Ctrl Pts',(7.59305526455752,10.9265492041506,-14.9294271056802));
#64433=CARTESIAN_POINT('Ctrl Pts',(7.50190235999067,10.8534064745166,-14.981777905381));
#64434=CARTESIAN_POINT('Ctrl Pts',(7.50095117894872,10.852644780527,-14.9823263263298));
#64435=CARTESIAN_POINT('Ctrl Pts',(7.5,10.8518846384445,-14.9828768864291));
#64436=CARTESIAN_POINT('',(8.,11.5504536489008,-15.0859875548336));
#64437=CARTESIAN_POINT('Ctrl Pts',(8.,11.5504536489008,-15.0859875548336));
#64438=CARTESIAN_POINT('Ctrl Pts',(8.,11.5339910291066,-15.0695249350393));
#64439=CARTESIAN_POINT('Ctrl Pts',(7.99834499880831,11.5164011008489,-15.0519350067816));
#64440=CARTESIAN_POINT('Ctrl Pts',(7.99471483561601,11.4987322092717,-15.0342661152045));
#64441=CARTESIAN_POINT('',(8.,15.0859875548336,-11.5504536489008));
#64442=CARTESIAN_POINT('Origin',(8.,0.,0.));
#64443=CARTESIAN_POINT('Ctrl Pts',(8.,15.0859875548336,-11.5504536489008));
#64444=CARTESIAN_POINT('Ctrl Pts',(8.,15.0695249347861,-11.5339910288533));
#64445=CARTESIAN_POINT('Ctrl Pts',(7.99834499875555,15.05193500624,-11.5164011003073));
#64446=CARTESIAN_POINT('Ctrl Pts',(7.9947148354483,15.0342661143882,-11.4987322084555));
#64447=CARTESIAN_POINT('Origin',(8.,13.3643181644257,-13.3643181644258));
#64448=CARTESIAN_POINT('',(8.,12.0208152801713,-15.556349186104));
#64449=CARTESIAN_POINT('',(8.,11.1722871427474,-14.7078210486802));
#64450=CARTESIAN_POINT('',(8.,15.556349186104,-12.0208152801713));
#64451=CARTESIAN_POINT('',(8.,12.0208152801713,-15.556349186104));
#64452=CARTESIAN_POINT('',(8.,15.556349186104,-12.0208152801713));
#64453=CARTESIAN_POINT('Origin',(5.75,-15.3878195049812,11.145178817862));
#64454=CARTESIAN_POINT('',(7.99471483544825,-15.034266114388,11.4987322084552));
#64455=CARTESIAN_POINT('',(5.75,-15.034266114388,11.4987322084552));
#64456=CARTESIAN_POINT('Ctrl Pts',(7.5,-14.9828768864291,10.8518846384445));
#64457=CARTESIAN_POINT('Ctrl Pts',(7.50105371344579,-14.9822669774523,10.8527267217707));
#64458=CARTESIAN_POINT('Ctrl Pts',(7.50210742973579,-14.9816596935132,10.8535707098407));
#64459=CARTESIAN_POINT('Ctrl Pts',(7.59351569467817,-14.9292065753492,10.9269504763458));
#64460=CARTESIAN_POINT('Ctrl Pts',(7.68214848767641,-14.8976245327994,11.0120989243863));
#64461=CARTESIAN_POINT('Ctrl Pts',(7.81958013152829,-14.8836434033437,11.1704454530308));
#64462=CARTESIAN_POINT('Ctrl Pts',(7.87098023972491,-14.8919941158642,11.2398826207743));
#64463=CARTESIAN_POINT('Ctrl Pts',(7.9404886750701,-14.9308215694369,11.3545161973499));
#64464=CARTESIAN_POINT('Ctrl Pts',(7.96491477585444,-14.9558097197834,11.4033401554798));
#64465=CARTESIAN_POINT('Ctrl Pts',(7.98678347589503,-15.0039319604951,11.4662908869417));
#64466=CARTESIAN_POINT('Ctrl Pts',(7.99147733125717,-15.0185083904014,11.4829744844687));
#64467=CARTESIAN_POINT('Ctrl Pts',(7.99471483544825,-15.034266114388,11.4987322084552));
#64468=CARTESIAN_POINT('Origin',(7.5,0.,0.));
#64469=CARTESIAN_POINT('',(7.99471483561596,-11.4987322092715,15.0342661152043));
#64470=CARTESIAN_POINT('Ctrl Pts',(7.99471483561596,-11.4987322092715,15.0342661152043));
#64471=CARTESIAN_POINT('Ctrl Pts',(7.99136258232109,-11.4824159731374,15.0179498789948));
#64472=CARTESIAN_POINT('Ctrl Pts',(7.98645003622191,-11.4651126007102,15.0029056934798));
#64473=CARTESIAN_POINT('Ctrl Pts',(7.964022711053,-11.4013638075406,14.954638836428));
#64474=CARTESIAN_POINT('Ctrl Pts',(7.93938632198288,-11.3524620624657,14.9298917928022));
#64475=CARTESIAN_POINT('Ctrl Pts',(7.86974221712845,-11.2381679469924,14.8917374982996));
#64476=CARTESIAN_POINT('Ctrl Pts',(7.81856316470117,-11.1692008513042,14.8836497863542));
#64477=CARTESIAN_POINT('Ctrl Pts',(7.68155929434292,-11.0115152525769,14.897811278973));
#64478=CARTESIAN_POINT('Ctrl Pts',(7.59305526455765,-10.9265492041507,14.9294271056801));
#64479=CARTESIAN_POINT('Ctrl Pts',(7.50190235999013,-10.8534064745162,14.9817779053813));
#64480=CARTESIAN_POINT('Ctrl Pts',(7.500951178949,-10.8526447805272,14.9823263263296));
#64481=CARTESIAN_POINT('Ctrl Pts',(7.5,-10.8518846384445,14.9828768864291));
#64482=CARTESIAN_POINT('',(8.,-11.5504536489008,15.0859875548336));
#64483=CARTESIAN_POINT('Ctrl Pts',(8.,-11.5504536489008,15.0859875548336));
#64484=CARTESIAN_POINT('Ctrl Pts',(8.,-11.5339910291066,15.0695249350393));
#64485=CARTESIAN_POINT('Ctrl Pts',(7.99834499880831,-11.5164011008489,15.0519350067816));
#64486=CARTESIAN_POINT('Ctrl Pts',(7.99471483561601,-11.4987322092717,15.0342661152045));
#64487=CARTESIAN_POINT('',(8.,-15.0859875548336,11.5504536489008));
#64488=CARTESIAN_POINT('Origin',(8.,0.,0.));
#64489=CARTESIAN_POINT('Ctrl Pts',(8.,-15.0859875548336,11.5504536489008));
#64490=CARTESIAN_POINT('Ctrl Pts',(8.,-15.0695249347861,11.5339910288533));
#64491=CARTESIAN_POINT('Ctrl Pts',(7.99834499875555,-15.05193500624,11.5164011003073));
#64492=CARTESIAN_POINT('Ctrl Pts',(7.9947148354483,-15.0342661143882,11.4987322084555));
#64493=CARTESIAN_POINT('Origin',(8.,-13.3643181644257,13.3643181644258));
#64494=CARTESIAN_POINT('',(8.,-12.0208152801713,15.556349186104));
#64495=CARTESIAN_POINT('',(8.,-11.1722871427475,14.7078210486802));
#64496=CARTESIAN_POINT('',(8.,-15.556349186104,12.0208152801713));
#64497=CARTESIAN_POINT('',(8.,-12.0208152801713,15.556349186104));
#64498=CARTESIAN_POINT('',(8.,-15.556349186104,12.0208152801713));
#64499=CARTESIAN_POINT('Origin',(5.75,-18.5741756210067,4.));
#64500=CARTESIAN_POINT('Ctrl Pts',(-2.,-18.0853815257171,3.89473684210527));
#64501=CARTESIAN_POINT('Ctrl Pts',(-2.00105371344577,-18.0856004217929,
3.89372038856659));
#64502=CARTESIAN_POINT('Ctrl Pts',(-2.00210742973639,-18.0858224890519,
3.8927046150788));
#64503=CARTESIAN_POINT('Ctrl Pts',(-2.09351569467844,-18.1053615522597,
3.80464699333924));
#64504=CARTESIAN_POINT('Ctrl Pts',(-2.1821484876768,-18.1476027839944,3.72425195644745));
#64505=CARTESIAN_POINT('Ctrl Pts',(-2.31958013152849,-18.2560609577744,
3.60803698471449));
#64506=CARTESIAN_POINT('Ctrl Pts',(-2.3709802397251,-18.3132986190962,3.56784861836004));
#64507=CARTESIAN_POINT('Ctrl Pts',(-2.44048867507028,-18.4245257150271,
3.52013110417223));
#64508=CARTESIAN_POINT('Ctrl Pts',(-2.46491477585457,-18.4775461366012,
3.50609467153023));
#64509=CARTESIAN_POINT('Ctrl Pts',(-2.48434736805665,-18.5477361044563,
3.50052662530652));
#64510=CARTESIAN_POINT('Ctrl Pts',(-2.48748442178248,-18.5609269169988,
3.5));
#64511=CARTESIAN_POINT('Ctrl Pts',(-2.49011275698595,-18.5741756210067,
3.5));
#64512=CARTESIAN_POINT('Origin',(-6.,0.,0.));
#64513=CARTESIAN_POINT('',(-6.5,-4.,-18.5741756210067));
#64514=CARTESIAN_POINT('Origin',(-6.,-4.00000000000001,-18.5741756210067));
#64515=CARTESIAN_POINT('',(-6.5,-18.6748493969831,-3.5));
#64516=CARTESIAN_POINT('Origin',(-6.5,0.,0.));
#64517=CARTESIAN_POINT('',(-6.49011275698595,-18.5741756210067,-3.5));
#64518=CARTESIAN_POINT('Ctrl Pts',(-6.5,-18.6748493969831,-3.5));
#64519=CARTESIAN_POINT('Ctrl Pts',(-6.5,-18.643018830074,-3.5));
#64520=CARTESIAN_POINT('Ctrl Pts',(-6.49686768006357,-18.6082253024678,
-3.5));
#64521=CARTESIAN_POINT('Ctrl Pts',(-6.49011275698595,-18.5741756210067,
-3.5));
#64522=CARTESIAN_POINT('Ctrl Pts',(-6.49011275698595,-18.5741756210067,
-3.5));
#64523=CARTESIAN_POINT('Ctrl Pts',(-6.48031734397251,-18.5247996785933,
-3.5));
#64524=CARTESIAN_POINT('Ctrl Pts',(-6.46374257315005,-18.4776012558686,
-3.50729593903647));
#64525=CARTESIAN_POINT('Ctrl Pts',(-6.41476836802977,-18.3774000478142,
-3.53660915976364));
#64526=CARTESIAN_POINT('Ctrl Pts',(-6.37965678312709,-18.3274816176557,
-3.56195342180394));
#64527=CARTESIAN_POINT('Ctrl Pts',(-6.29338459766337,-18.232217901755,-3.62956958867485));
#64528=CARTESIAN_POINT('Ctrl Pts',(-6.23978806301794,-18.1898427129628,
-3.67485926714064));
#64529=CARTESIAN_POINT('Ctrl Pts',(-6.12593686398507,-18.122961239244,-3.77570829974231));
#64530=CARTESIAN_POINT('Ctrl Pts',(-6.0642827765107,-18.0991128412042,-3.83280835545914));
#64531=CARTESIAN_POINT('Ctrl Pts',(-6.00210742973624,-18.0858224890518,
-3.89270461507938));
#64532=CARTESIAN_POINT('Ctrl Pts',(-6.0010537134456,-18.0856004217928,-3.89372038856676));
#64533=CARTESIAN_POINT('Ctrl Pts',(-6.,-18.0853815257171,-3.89473684210526));
#64534=CARTESIAN_POINT('Origin',(-6.,-4.,-18.5741756210067));
#64535=CARTESIAN_POINT('',(-6.,-3.5,-18.5741756210067));
#64536=CARTESIAN_POINT('Origin',(-6.,-4.,-18.5741756210067));
#64537=CARTESIAN_POINT('Origin',(-6.,-4.,-18.5741756210067));
#64538=CARTESIAN_POINT('Origin',(5.75,-18.5741756210067,-4.));
#64539=CARTESIAN_POINT('',(-2.49011275698595,-18.5741756210067,-3.5));
#64540=CARTESIAN_POINT('',(5.75,-18.5741756210067,-3.5));
#64541=CARTESIAN_POINT('Ctrl Pts',(-2.49011275698595,-18.5741756210067,
-3.5));
#64542=CARTESIAN_POINT('Ctrl Pts',(-2.48031734397251,-18.5247996785933,
-3.5));
#64543=CARTESIAN_POINT('Ctrl Pts',(-2.46374257315005,-18.4776012558686,
-3.50729593903647));
#64544=CARTESIAN_POINT('Ctrl Pts',(-2.41476836802978,-18.3774000478142,
-3.53660915976364));
#64545=CARTESIAN_POINT('Ctrl Pts',(-2.3796567831271,-18.3274816176557,-3.56195342180394));
#64546=CARTESIAN_POINT('Ctrl Pts',(-2.29338459766337,-18.232217901755,-3.62956958867485));
#64547=CARTESIAN_POINT('Ctrl Pts',(-2.23978806301794,-18.1898427129628,
-3.67485926714064));
#64548=CARTESIAN_POINT('Ctrl Pts',(-2.12593686398505,-18.122961239244,-3.77570829974233));
#64549=CARTESIAN_POINT('Ctrl Pts',(-2.06428277651057,-18.0991128412042,
-3.83280835545912));
#64550=CARTESIAN_POINT('Ctrl Pts',(-2.00210742973612,-18.0858224890517,
-3.89270461507951));
#64551=CARTESIAN_POINT('Ctrl Pts',(-2.0010537134457,-18.0856004217928,-3.89372038856666));
#64552=CARTESIAN_POINT('Ctrl Pts',(-2.,-18.0853815257171,-3.89473684210526));
#64553=CARTESIAN_POINT('Origin',(-2.,0.,0.));
#64554=CARTESIAN_POINT('Ctrl Pts',(-2.49011275698578,-18.5741756210058,
-3.5));
#64555=CARTESIAN_POINT('Ctrl Pts',(-2.49686768006346,-18.608225302467,-3.5));
#64556=CARTESIAN_POINT('Ctrl Pts',(-2.5,-18.643018830074,-3.5));
#64557=CARTESIAN_POINT('Ctrl Pts',(-2.5,-18.6748493969831,-3.5));
#64558=CARTESIAN_POINT('Origin',(-6.,0.,0.));
#64559=CARTESIAN_POINT('Origin',(-2.,0.,0.));
#64560=CARTESIAN_POINT('Origin',(-2.5,0.,0.));
#64561=CARTESIAN_POINT('Origin',(-2.5,1.11022302462516E-15,19.75));
#64562=CARTESIAN_POINT('Origin',(5.75,-4.,-18.5741756210067));
#64563=CARTESIAN_POINT('',(5.75,-3.5,-18.5741756210067));
#64564=CARTESIAN_POINT('Origin',(-6.,-4.,-9.));
#64565=CARTESIAN_POINT('',(-6.,-3.5,-20.1059692628831));
#64566=CARTESIAN_POINT('',(-6.,-3.5,-9.));
#64567=CARTESIAN_POINT('',(-6.5,-4.,-20.1059692628831));
#64568=CARTESIAN_POINT('Origin',(-6.,-4.,-20.1059692628831));
#64569=CARTESIAN_POINT('',(-6.5,-4.,-9.));
#64570=CARTESIAN_POINT('Origin',(-6.,-4.,-20.1059692628831));
#64571=CARTESIAN_POINT('Ctrl Pts',(-6.,-4.09756097560976,-20.5963587570998));
#64572=CARTESIAN_POINT('Ctrl Pts',(-6.,-4.0683589966744,-20.6021683708624));
#64573=CARTESIAN_POINT('Ctrl Pts',(-6.00276332358265,-4.03610462934205,
-20.6056974194132));
#64574=CARTESIAN_POINT('Ctrl Pts',(-6.01450725061641,-3.97271232495602,
-20.6060535888886));
#64575=CARTESIAN_POINT('Ctrl Pts',(-6.02348817950739,-3.94157444978542,
-20.6028809931646));
#64576=CARTESIAN_POINT('Ctrl Pts',(-6.04683850352093,-3.88079927444089,
-20.5906622808365));
#64577=CARTESIAN_POINT('Ctrl Pts',(-6.0663740221613,-3.84384286975754,-20.5777101026407));
#64578=CARTESIAN_POINT('Ctrl Pts',(-6.10731554914672,-3.78596404697746,
-20.5468117668285));
#64579=CARTESIAN_POINT('Ctrl Pts',(-6.13400314988651,-3.75806187938217,
-20.5247907757942));
#64580=CARTESIAN_POINT('Ctrl Pts',(-6.19164793481474,-3.71718369216096,
-20.4736489647519));
#64581=CARTESIAN_POINT('Ctrl Pts',(-6.22260859132108,-3.70420972323454,
-20.4445304195459));
#64582=CARTESIAN_POINT('Ctrl Pts',(-6.25150607875357,-3.69905785638952,
-20.4160958798464));
#64583=CARTESIAN_POINT('Ctrl Pts',(-6.2801544416415,-3.69395040366473,-20.3879064736302));
#64584=CARTESIAN_POINT('Ctrl Pts',(-6.31086688890514,-3.69580208067255,
-20.3563629124601));
#64585=CARTESIAN_POINT('Ctrl Pts',(-6.36807510645317,-3.71571514780993,
-20.2945810740561));
#64586=CARTESIAN_POINT('Ctrl Pts',(-6.39456832517073,-3.73377436649843,
-20.2643397343447));
#64587=CARTESIAN_POINT('Ctrl Pts',(-6.43496570369138,-3.77614009919508,
-20.2153893012592));
#64588=CARTESIAN_POINT('Ctrl Pts',(-6.45415498120474,-3.80533050967996,
-20.1903979662949));
#64589=CARTESIAN_POINT('Ctrl Pts',(-6.48727536023424,-3.8791679039915,-20.1426530305365));
#64590=CARTESIAN_POINT('Ctrl Pts',(-6.5,-3.94295127275524,-20.117318872842));
#64591=CARTESIAN_POINT('Ctrl Pts',(-6.5,-4.,-20.1059692628831));
#64592=CARTESIAN_POINT('Origin',(-6.,-4.,-20.1059692628831));
#64593=CARTESIAN_POINT('Origin',(11.6,-4.,-20.1059692628831));
#64594=CARTESIAN_POINT('',(11.6,-3.5,-20.1059692628831));
#64595=CARTESIAN_POINT('Origin',(-6.5,-3.5,-18.));
#64596=CARTESIAN_POINT('Origin',(-6.,0.,0.));
#64597=CARTESIAN_POINT('Origin',(-6.5,0.,0.));
#64598=CARTESIAN_POINT('Origin',(-6.35355339059327,-1.11022302462516E-15,
-1.11022302462516E-15));
#64599=CARTESIAN_POINT('Origin',(-6.5,20.5,0.));
#64600=CARTESIAN_POINT('',(-6.5,4.,-18.5741756210067));
#64601=CARTESIAN_POINT('',(-6.5,4.,-10.75));
#64602=CARTESIAN_POINT('Origin',(-6.5,0.,0.));
#64603=CARTESIAN_POINT('Origin',(-6.,4.,-10.75));
#64604=CARTESIAN_POINT('',(-6.,3.5,-18.5741756210067));
#64605=CARTESIAN_POINT('',(-6.,3.5,-10.75));
#64606=CARTESIAN_POINT('Origin',(-6.,4.,-18.5741756210067));
#64607=CARTESIAN_POINT('Origin',(-6.,4.,-18.5741756210067));
#64608=CARTESIAN_POINT('Origin',(-6.,4.,-18.5741756210067));
#64609=CARTESIAN_POINT('Origin',(-6.,4.,-18.5741756210067));
#64610=CARTESIAN_POINT('Origin',(-6.,18.5741756210067,-4.));
#64611=CARTESIAN_POINT('Origin',(-6.,18.5741756210067,-4.));
#64612=CARTESIAN_POINT('Origin',(-6.,18.5741756210067,-4.));
#64613=CARTESIAN_POINT('Origin',(5.75,18.5741756210067,-4.));
#64614=CARTESIAN_POINT('Origin',(-6.,0.,0.));
#64615=CARTESIAN_POINT('Origin',(5.75,4.,-18.5741756210067));
#64616=CARTESIAN_POINT('',(5.75,3.5,-18.5741756210067));
#64617=CARTESIAN_POINT('Origin',(-6.5,3.5,-21.5));
#64618=CARTESIAN_POINT('Origin',(-6.5,20.5,0.));
#64619=CARTESIAN_POINT('',(-6.5,-20.1975426238546,-3.50845720475184));
#64620=CARTESIAN_POINT('Origin',(-6.5,0.,0.));
#64621=CARTESIAN_POINT('',(-6.5,-20.1059692628831,-3.5));
#64622=CARTESIAN_POINT('Origin',(-6.5,-20.1059692628831,-3.99999999999999));
#64623=CARTESIAN_POINT('',(-6.5,-0.5,-3.5));
#64624=CARTESIAN_POINT('Origin',(11.6,-20.1059692628831,-3.99999999999999));
#64625=CARTESIAN_POINT('Ctrl Pts',(-6.5,-20.1975426238546,-3.50845720475183));
#64626=CARTESIAN_POINT('Ctrl Pts',(-6.44146838187229,-20.2550884935232,
-3.51917787596606));
#64627=CARTESIAN_POINT('Ctrl Pts',(-6.37838919138939,-20.3152794800863,
-3.54130503996253));
#64628=CARTESIAN_POINT('Ctrl Pts',(-6.2559198324237,-20.4273638888019,-3.6111352406743));
#64629=CARTESIAN_POINT('Ctrl Pts',(-6.19673011624031,-20.4788885029216,
-3.65972871821816));
#64630=CARTESIAN_POINT('Ctrl Pts',(-6.10742473363203,-20.5506848087795,
-3.76440047785072));
#64631=CARTESIAN_POINT('Ctrl Pts',(-6.06891141762746,-20.5788865473403,
-3.82410317982267));
#64632=CARTESIAN_POINT('Ctrl Pts',(-6.02857797268264,-20.6012039162238,
-3.92325195833915));
#64633=CARTESIAN_POINT('Ctrl Pts',(-6.01793177509303,-20.6054227657767,
-3.95789306108273));
#64634=CARTESIAN_POINT('Ctrl Pts',(-6.00364389418785,-20.6064145558324,
-4.02788015641737));
#64635=CARTESIAN_POINT('Ctrl Pts',(-6.,-20.6031896256267,-4.0632256674496));
#64636=CARTESIAN_POINT('Ctrl Pts',(-6.,-20.5963587570998,-4.09756097560975));
#64637=CARTESIAN_POINT('',(11.6,-20.1059692628831,-3.5));
#64638=CARTESIAN_POINT('Origin',(-6.5,-21.5,-3.5));
#64639=CARTESIAN_POINT('Origin',(5.75,11.145178817862,15.3878195049812));
#64640=CARTESIAN_POINT('',(7.9947148353915,11.4987322083171,15.0342661142498));
#64641=CARTESIAN_POINT('Ctrl Pts',(7.99471483544825,11.4987322084552,15.034266114388));
#64642=CARTESIAN_POINT('Ctrl Pts',(7.98790837769307,11.4656035153935,15.0011374213262));
#64643=CARTESIAN_POINT('Ctrl Pts',(7.97481356608163,11.4290648513116,14.9738935230493));
#64644=CARTESIAN_POINT('Ctrl Pts',(7.93533857113774,11.3448695865394,14.926398354714));
#64645=CARTESIAN_POINT('Ctrl Pts',(7.9072623646401,11.2974038150965,14.9091857104132));
#64646=CARTESIAN_POINT('Ctrl Pts',(7.83244151643846,11.1875808446044,14.8854247099832));
#64647=CARTESIAN_POINT('Ctrl Pts',(7.78233548373286,11.1255843049717,14.8848332489223));
#64648=CARTESIAN_POINT('Ctrl Pts',(7.65786764210673,10.9886851823176,14.9061789600546));
#64649=CARTESIAN_POINT('Ctrl Pts',(7.57955614016674,10.9156732068678,14.9371191012641));
#64650=CARTESIAN_POINT('Ctrl Pts',(7.50156833754672,10.8531390412775,14.9819705581587));
#64651=CARTESIAN_POINT('Ctrl Pts',(7.50078416818792,10.8525113125737,14.9824229952701));
#64652=CARTESIAN_POINT('Ctrl Pts',(7.5,10.8518846384445,14.9828768864291));
#64653=CARTESIAN_POINT('',(5.75,11.4987322084552,15.034266114388));
#64654=CARTESIAN_POINT('Origin',(8.,12.0208152801713,15.556349186104));
#64655=CARTESIAN_POINT('',(8.,11.5504536489008,15.0859875548336));
#64656=CARTESIAN_POINT('Ctrl Pts',(7.99471483541929,11.4987322083143,15.034266114247));
#64657=CARTESIAN_POINT('Ctrl Pts',(7.99834499874643,11.5164011002136,15.0519350061464));
#64658=CARTESIAN_POINT('Ctrl Pts',(8.,11.5339910288095,15.0695249347422));
#64659=CARTESIAN_POINT('Ctrl Pts',(8.,11.5504536489008,15.0859875548336));
#64660=CARTESIAN_POINT('',(8.,12.0208152801713,15.556349186104));
#64661=CARTESIAN_POINT('',(8.,12.0208152801713,15.556349186104));
#64662=CARTESIAN_POINT('',(29.337248848077,12.0208152801996,15.5563491860757));
#64663=CARTESIAN_POINT('',(8.,12.0208152801713,15.556349186104));
#64664=CARTESIAN_POINT('',(29.6961037355001,12.622503406322,16.1580373122142));
#64665=CARTESIAN_POINT('Ctrl Pts',(29.3372488480671,12.0208152801713,15.556349186104));
#64666=CARTESIAN_POINT('Ctrl Pts',(29.3635470277544,12.0208152801713,15.556349186104));
#64667=CARTESIAN_POINT('Ctrl Pts',(29.3897411711777,12.0223153633463,15.5578483797216));
#64668=CARTESIAN_POINT('Ctrl Pts',(29.415607431348,12.0252248665426,15.5607573876018));
#64669=CARTESIAN_POINT('Ctrl Pts',(29.4419059568771,12.0281829920537,15.5637150095193));
#64670=CARTESIAN_POINT('Ctrl Pts',(29.4678668567866,12.0325981572608,15.5681303086097));
#64671=CARTESIAN_POINT('Ctrl Pts',(29.4932488211205,12.0384121343065,15.5739465388115));
#64672=CARTESIAN_POINT('Ctrl Pts',(29.5056295238234,12.0412480504074,15.5767835539469));
#64673=CARTESIAN_POINT('Ctrl Pts',(29.5178722688888,12.0444173222899,15.5799544093235));
#64674=CARTESIAN_POINT('Ctrl Pts',(29.5299470752204,12.0479161878527,15.583455268391));
#64675=CARTESIAN_POINT('Ctrl Pts',(29.5545920296324,12.055057452062,15.5906006013887));
#64676=CARTESIAN_POINT('Ctrl Pts',(29.5783543573571,12.0635161276847,15.599065190727));
#64677=CARTESIAN_POINT('Ctrl Pts',(29.6010013147649,12.0732271832776,15.6087800031479));
#64678=CARTESIAN_POINT('Ctrl Pts',(29.6182267197699,12.0806134675631,15.6161691448982));
#64679=CARTESIAN_POINT('Ctrl Pts',(29.6348068591577,12.0887250603625,15.6242823638422));
#64680=CARTESIAN_POINT('Ctrl Pts',(29.6506294743871,12.0975465693583,15.6331010316835));
#64681=CARTESIAN_POINT('Ctrl Pts',(29.6654204617391,12.1057929196669,15.6413447260799));
#64682=CARTESIAN_POINT('Ctrl Pts',(29.6795495016601,12.11465988999,15.6502051489654));
#64683=CARTESIAN_POINT('Ctrl Pts',(29.6929623869925,12.1240948005673,15.6596335337303));
#64684=CARTESIAN_POINT('Ctrl Pts',(29.7117060225708,12.1372794749451,15.6728090887094));
#64685=CARTESIAN_POINT('Ctrl Pts',(29.7289079510306,12.1514701038323,15.6869909142991));
#64686=CARTESIAN_POINT('Ctrl Pts',(29.7444572669056,12.1664988608128,15.702017054101));
#64687=CARTESIAN_POINT('Ctrl Pts',(29.7600106951658,12.1815315925043,15.7170471679217));
#64688=CARTESIAN_POINT('Ctrl Pts',(29.7739113767554,12.1974036551567,15.7329229380823));
#64689=CARTESIAN_POINT('Ctrl Pts',(29.7860080855976,12.2139724871026,15.7495003064955));
#64690=CARTESIAN_POINT('Ctrl Pts',(29.791664963973,12.2217206993116,15.7572525106794));
#64691=CARTESIAN_POINT('Ctrl Pts',(29.7969266990531,12.2296215756952,15.7651583175465));
#64692=CARTESIAN_POINT('Ctrl Pts',(29.8017740895476,12.2376617310126,15.7732035029928));
#64693=CARTESIAN_POINT('Ctrl Pts',(29.8121759038628,12.2549147670066,15.790467332932));
#64694=CARTESIAN_POINT('Ctrl Pts',(29.8205897043332,12.2726701275567,15.8082344070815));
#64695=CARTESIAN_POINT('Ctrl Pts',(29.8268838981186,12.2907815683395,15.8263459586653));
#64696=CARTESIAN_POINT('Ctrl Pts',(29.8272913784438,12.2919540863824,15.8275184838813));
#64697=CARTESIAN_POINT('Ctrl Pts',(29.8276899587999,12.2931281037408,15.8286924566032));
#64698=CARTESIAN_POINT('Ctrl Pts',(29.8280795964848,12.2943035834062,15.8298678350682));
#64699=CARTESIAN_POINT('Ctrl Pts',(29.8341018209758,12.3124717501507,15.8480344376629));
#64700=CARTESIAN_POINT('Ctrl Pts',(29.8379920903211,12.3309885244332,15.8665369818169));
#64701=CARTESIAN_POINT('Ctrl Pts',(29.8397834073069,12.3496695928917,15.8852056233943));
#64702=CARTESIAN_POINT('Ctrl Pts',(29.8404573868658,12.3566983088467,15.8922296637593));
#64703=CARTESIAN_POINT('Ctrl Pts',(29.8408337073171,12.3637503539871,15.8992771857621));
#64704=CARTESIAN_POINT('Ctrl Pts',(29.8409122430702,12.3708160009656,15.9063388639076));
#64705=CARTESIAN_POINT('Ctrl Pts',(29.841120187594,12.3895242012339,15.9250365556235));
#64706=CARTESIAN_POINT('Ctrl Pts',(29.8392425388124,12.408176797555,15.9436833457277));
#64707=CARTESIAN_POINT('Ctrl Pts',(29.8353415852943,12.4265962129204,15.9621050094994));
#64708=CARTESIAN_POINT('Ctrl Pts',(29.8314529329103,12.444957545128,15.9804685830232));
#64709=CARTESIAN_POINT('Ctrl Pts',(29.8255535219378,12.4630881464923,15.9986093924684));
#64710=CARTESIAN_POINT('Ctrl Pts',(29.8176551502899,12.4808142028984,16.0163472264152));
#64711=CARTESIAN_POINT('Ctrl Pts',(29.8141109427822,12.4887683515505,16.0243066599602));
#64712=CARTESIAN_POINT('Ctrl Pts',(29.8101635813264,12.4966409819043,16.0321847640837));
#64713=CARTESIAN_POINT('Ctrl Pts',(29.8058109922455,12.5044157250982,16.0399639788116));
#64714=CARTESIAN_POINT('Ctrl Pts',(29.8017570288636,12.5116570528749,16.047209471336));
#64715=CARTESIAN_POINT('Ctrl Pts',(29.7973617576496,12.5187951035663,16.0543508658078));
#64716=CARTESIAN_POINT('Ctrl Pts',(29.7926271891834,12.5258177264801,16.0613748908172));
#64717=CARTESIAN_POINT('Ctrl Pts',(29.7829544505439,12.5401649677324,16.0757249965551));
#64718=CARTESIAN_POINT('Ctrl Pts',(29.7718670650361,12.5540309525854,16.0895860215957));
#64719=CARTESIAN_POINT('Ctrl Pts',(29.7594824084562,12.5673324817764,16.1028820334627));
#64720=CARTESIAN_POINT('Ctrl Pts',(29.7449214392347,12.5829714424452,16.1185145072673));
#64721=CARTESIAN_POINT('Ctrl Pts',(29.7286275829089,12.5977667684327,16.1333027723117));
#64722=CARTESIAN_POINT('Ctrl Pts',(29.7107932614126,12.6115882202006,16.1471218329623));
#64723=CARTESIAN_POINT('Ctrl Pts',(29.7060063962345,12.6152980011526,16.1508309721205));
#64724=CARTESIAN_POINT('Ctrl Pts',(29.701108313897,12.6189375257568,16.1544701493208));
#64725=CARTESIAN_POINT('Ctrl Pts',(29.6961022501539,12.622504030493,16.1580366171471));
#64726=CARTESIAN_POINT('',(29.8535533905933,12.5103262255613,16.0458601314941));
#64727=CARTESIAN_POINT('Ctrl Pts',(29.6961037355001,12.622503406322,16.1580373122142));
#64728=CARTESIAN_POINT('Ctrl Pts',(29.7751366074575,12.5661986334316,16.101732539364));
#64729=CARTESIAN_POINT('Ctrl Pts',(29.8535533905933,12.5103262255613,16.0458601314941));
#64730=CARTESIAN_POINT('',(30.,12.2583832540376,15.7939171599704));
#64731=CARTESIAN_POINT('Ctrl Pts',(29.8535533905933,12.5103262255613,16.0458601314941));
#64732=CARTESIAN_POINT('Ctrl Pts',(29.8971736290481,12.4792465554081,16.0147804613409));
#64733=CARTESIAN_POINT('Ctrl Pts',(29.9381460122713,12.4355437242224,15.9710776301552));
#64734=CARTESIAN_POINT('Ctrl Pts',(29.985486770529,12.3543653386467,15.8898992445794));
#64735=CARTESIAN_POINT('Ctrl Pts',(30.,12.3024682657458,15.8380021716785));
#64736=CARTESIAN_POINT('Ctrl Pts',(30.,12.2583832540376,15.7939171599704));
#64737=CARTESIAN_POINT('',(30.,11.5504536489008,15.0859875548336));
#64738=CARTESIAN_POINT('',(30.,9.75152416360247,13.2870580695352));
#64739=CARTESIAN_POINT('',(29.5,11.1937144438494,14.7292483497821));
#64740=CARTESIAN_POINT('Ctrl Pts',(29.5,11.1937144438494,14.7292483497821));
#64741=CARTESIAN_POINT('Ctrl Pts',(29.5615281526734,11.1937144438494,14.7292483497821));
#64742=CARTESIAN_POINT('Ctrl Pts',(29.6339241856893,11.2039672958034,14.7395012017362));
#64743=CARTESIAN_POINT('Ctrl Pts',(29.7477912665658,11.237498416831,14.7730323227637));
#64744=CARTESIAN_POINT('Ctrl Pts',(29.8093392860887,11.2667800757207,14.8023139816534));
#64745=CARTESIAN_POINT('Ctrl Pts',(29.8967622377582,11.3289413274527,14.8644752333855));
#64746=CARTESIAN_POINT('Ctrl Pts',(29.9380095827943,11.3728886696422,14.908422575575));
#64747=CARTESIAN_POINT('Ctrl Pts',(29.9854746058202,11.4543428055946,14.9898767115274));
#64748=CARTESIAN_POINT('Ctrl Pts',(30.,11.5063099570288,15.0418438629615));
#64749=CARTESIAN_POINT('Ctrl Pts',(30.,11.5504536489008,15.0859875548336));
#64750=CARTESIAN_POINT('',(25.5,11.1937144438494,14.7292483497821));
#64751=CARTESIAN_POINT('Origin',(7.5,0.,0.));
#64752=CARTESIAN_POINT('',(7.99471483561596,15.0342661152043,11.4987322092715));
#64753=CARTESIAN_POINT('',(8.,15.0859875548336,11.5504536489008));
#64754=CARTESIAN_POINT('Ctrl Pts',(8.,15.0859875548336,11.5504536489008));
#64755=CARTESIAN_POINT('Ctrl Pts',(8.,15.0695249350393,11.5339910291066));
#64756=CARTESIAN_POINT('Ctrl Pts',(7.99834499880831,15.0519350067816,11.5164011008489));
#64757=CARTESIAN_POINT('Ctrl Pts',(7.99471483561601,15.0342661152045,11.4987322092718));
#64758=CARTESIAN_POINT('Origin',(8.,0.,0.));
#64759=CARTESIAN_POINT('Ctrl Pts',(7.99471483561596,15.0342661152043,11.4987322092715));
#64760=CARTESIAN_POINT('Ctrl Pts',(7.99136258232187,15.0179498789986,11.4824159731412));
#64761=CARTESIAN_POINT('Ctrl Pts',(7.98645003622417,15.0029056934867,11.4651126007181));
#64762=CARTESIAN_POINT('Ctrl Pts',(7.96402271105946,14.9546388364367,11.4013638075551));
#64763=CARTESIAN_POINT('Ctrl Pts',(7.9393863219916,14.9298917928097,11.3524620624821));
#64764=CARTESIAN_POINT('Ctrl Pts',(7.86974221714271,14.8917374983038,11.2381679470131));
#64765=CARTESIAN_POINT('Ctrl Pts',(7.8185631647191,14.8836497863555,11.1692008513272));
#64766=CARTESIAN_POINT('Ctrl Pts',(7.68155929436919,14.8978112789661,11.011515252604));
#64767=CARTESIAN_POINT('Ctrl Pts',(7.59305526458688,14.9294271056729,10.9265492041609));
#64768=CARTESIAN_POINT('Ctrl Pts',(7.50190235999017,14.9817779053809,10.8534064745168));
#64769=CARTESIAN_POINT('Ctrl Pts',(7.5009511789491,14.9823263263295,10.8526447805273));
#64770=CARTESIAN_POINT('Ctrl Pts',(7.5,14.9828768864291,10.8518846384445));
#64771=CARTESIAN_POINT('Origin',(8.,13.3643181644258,13.3643181644258));
#64772=CARTESIAN_POINT('',(8.,15.556349186104,12.0208152801713));
#64773=CARTESIAN_POINT('',(8.,14.7078210486802,11.1722871427475));
#64774=CARTESIAN_POINT('',(8.,15.556349186104,12.0208152801713));
#64775=CARTESIAN_POINT('Origin',(28.9928932188134,0.,0.));
#64776=CARTESIAN_POINT('',(29.3464466094067,-2.55382374106385E-15,20.8535533905933));
#64777=CARTESIAN_POINT('',(29.3464466094067,-20.8535533905933,-2.55382374106385E-15));
#64778=CARTESIAN_POINT('Origin',(29.3464466094067,0.,-3.19227967632981E-15));
#64779=CARTESIAN_POINT('Origin',(29.3464466094067,0.,-3.19227967632981E-15));
#64780=CARTESIAN_POINT('Origin',(28.9928932188134,-2.51052593825207E-15,
20.5));
#64781=CARTESIAN_POINT('Origin',(29.6,0.,0.));
#64782=CARTESIAN_POINT('',(29.8535533905933,12.5103262255613,-16.0458601314941));
#64783=CARTESIAN_POINT('',(29.6961037355001,12.622503406322,-16.1580373122142));
#64784=CARTESIAN_POINT('Ctrl Pts',(29.8535533905933,12.5103262255613,-16.0458601314941));
#64785=CARTESIAN_POINT('Ctrl Pts',(29.775136607461,12.5661986334541,-16.1017325393463));
#64786=CARTESIAN_POINT('Ctrl Pts',(29.6961037355001,12.622503406322,-16.1580373122142));
#64787=CARTESIAN_POINT('',(29.8535533905933,-20.3464466094067,-2.49172107142325E-15));
#64788=CARTESIAN_POINT('Origin',(29.8535533905933,0.,-3.11465133927906E-15));
#64789=CARTESIAN_POINT('',(29.6,-20.6,-2.52277240624355E-15));
#64790=CARTESIAN_POINT('',(29.8535533905933,-16.0458601314941,12.5103262255613));
#64791=CARTESIAN_POINT('Origin',(29.8535533905933,0.,-3.11465133927906E-15));
#64792=CARTESIAN_POINT('',(29.6961037355001,-16.1580373122142,12.622503406322));
#64793=CARTESIAN_POINT('Ctrl Pts',(29.6961037355001,-16.1580373122142,12.622503406322));
#64794=CARTESIAN_POINT('Ctrl Pts',(29.7751366074575,-16.101732539364,12.5661986334316));
#64795=CARTESIAN_POINT('Ctrl Pts',(29.8535533905933,-16.0458601314941,12.5103262255613));
#64796=CARTESIAN_POINT('',(29.6961037355001,-12.622503406322,16.1580373122142));
#64797=CARTESIAN_POINT('Ctrl Pts',(29.6961021613978,-12.622503505457,16.1580371399984));
#64798=CARTESIAN_POINT('Ctrl Pts',(29.8947432207477,-13.7975614582838,14.9878688132478));
#64799=CARTESIAN_POINT('Ctrl Pts',(29.8947432207477,-14.9878688132478,13.7975614582838));
#64800=CARTESIAN_POINT('Ctrl Pts',(29.6961021613978,-16.1580371399984,12.622503505457));
#64801=CARTESIAN_POINT('',(29.8535533905933,-12.5103262255613,16.0458601314941));
#64802=CARTESIAN_POINT('Ctrl Pts',(29.8535533905933,-12.5103262255613,16.0458601314941));
#64803=CARTESIAN_POINT('Ctrl Pts',(29.775136607461,-12.5661986334541,16.1017325393463));
#64804=CARTESIAN_POINT('Ctrl Pts',(29.6961037355001,-12.622503406322,16.1580373122142));
#64805=CARTESIAN_POINT('Origin',(29.8535533905933,0.,-3.11465133927906E-15));
#64806=CARTESIAN_POINT('',(29.6961037355001,16.1580373122142,12.622503406322));
#64807=CARTESIAN_POINT('Ctrl Pts',(29.6961021613978,16.1580371399984,12.622503505457));
#64808=CARTESIAN_POINT('Ctrl Pts',(29.89474322789,14.9878687711962,13.7975615005113));
#64809=CARTESIAN_POINT('Ctrl Pts',(29.8947432136049,13.7975614160535,14.9878688553023));
#64810=CARTESIAN_POINT('Ctrl Pts',(29.6961021613977,12.622503505457,16.1580371399984));
#64811=CARTESIAN_POINT('',(29.8535533905933,16.0458601314941,12.5103262255613));
#64812=CARTESIAN_POINT('Ctrl Pts',(29.8535533905933,16.0458601314941,12.5103262255613));
#64813=CARTESIAN_POINT('Ctrl Pts',(29.775136607461,16.1017325393463,12.5661986334541));
#64814=CARTESIAN_POINT('Ctrl Pts',(29.6961037355001,16.1580373122142,12.622503406322));
#64815=CARTESIAN_POINT('',(29.8535533905933,16.0458601314941,-12.5103262255613));
#64816=CARTESIAN_POINT('Origin',(29.8535533905933,0.,-3.11465133927906E-15));
#64817=CARTESIAN_POINT('',(29.6961037355001,16.1580373122142,-12.622503406322));
#64818=CARTESIAN_POINT('Ctrl Pts',(29.6961037355001,16.1580373122142,-12.622503406322));
#64819=CARTESIAN_POINT('Ctrl Pts',(29.7751366074575,16.101732539364,-12.5661986334316));
#64820=CARTESIAN_POINT('Ctrl Pts',(29.8535533905933,16.0458601314941,-12.5103262255613));
#64821=CARTESIAN_POINT('Ctrl Pts',(29.6961021613978,12.622503505457,-16.1580371399984));
#64822=CARTESIAN_POINT('Ctrl Pts',(29.8947432207477,13.7975614582838,-14.9878688132478));
#64823=CARTESIAN_POINT('Ctrl Pts',(29.8947432207477,14.9878688132478,-13.7975614582838));
#64824=CARTESIAN_POINT('Ctrl Pts',(29.6961021613978,16.1580371399984,-12.622503505457));
#64825=CARTESIAN_POINT('Origin',(5.75,-11.145178817862,15.3878195049812));
#64826=CARTESIAN_POINT('',(5.75,-11.4987322084552,15.034266114388));
#64827=CARTESIAN_POINT('Origin',(8.,-11.1722871427475,14.7078210486802));
#64828=CARTESIAN_POINT('',(29.5,-11.1937144438494,14.7292483497821));
#64829=CARTESIAN_POINT('',(25.5,-11.1937144438494,14.7292483497821));
#64830=CARTESIAN_POINT('',(30.,-11.5504536489008,15.0859875548336));
#64831=CARTESIAN_POINT('Ctrl Pts',(30.,-11.5504536489008,15.0859875548336));
#64832=CARTESIAN_POINT('Ctrl Pts',(30.,-11.5063099570288,15.0418438629615));
#64833=CARTESIAN_POINT('Ctrl Pts',(29.9854746058202,-11.4543428055946,14.9898767115274));
#64834=CARTESIAN_POINT('Ctrl Pts',(29.9380095827943,-11.3728886696422,14.908422575575));
#64835=CARTESIAN_POINT('Ctrl Pts',(29.8967622377582,-11.3289413274527,14.8644752333855));
#64836=CARTESIAN_POINT('Ctrl Pts',(29.8093392860887,-11.2667800757207,14.8023139816534));
#64837=CARTESIAN_POINT('Ctrl Pts',(29.7477912665658,-11.237498416831,14.7730323227637));
#64838=CARTESIAN_POINT('Ctrl Pts',(29.6339241856893,-11.2039672958034,14.7395012017362));
#64839=CARTESIAN_POINT('Ctrl Pts',(29.5615281526734,-11.1937144438494,14.7292483497821));
#64840=CARTESIAN_POINT('Ctrl Pts',(29.5,-11.1937144438494,14.7292483497821));
#64841=CARTESIAN_POINT('',(30.,-12.2583832540376,15.7939171599704));
#64842=CARTESIAN_POINT('',(30.,-0.07726009489054,3.61279400082328));
#64843=CARTESIAN_POINT('Ctrl Pts',(30.,-12.2583832540376,15.7939171599704));
#64844=CARTESIAN_POINT('Ctrl Pts',(30.,-12.3024682657458,15.8380021716785));
#64845=CARTESIAN_POINT('Ctrl Pts',(29.985486770529,-12.3543653386467,15.8898992445794));
#64846=CARTESIAN_POINT('Ctrl Pts',(29.9381460122713,-12.4355437242224,15.9710776301552));
#64847=CARTESIAN_POINT('Ctrl Pts',(29.8971736290481,-12.4792465554081,16.0147804613409));
#64848=CARTESIAN_POINT('Ctrl Pts',(29.8535533905933,-12.5103262255613,16.0458601314941));
#64849=CARTESIAN_POINT('',(29.337248848077,-12.0208152801996,15.5563491860757));
#64850=CARTESIAN_POINT('Ctrl Pts',(29.6961022501482,-12.6225040304587,16.1580366171813));
#64851=CARTESIAN_POINT('Ctrl Pts',(29.7147933690558,-12.609187786889,16.1447205114285));
#64852=CARTESIAN_POINT('Ctrl Pts',(29.7319458264551,-12.5948812492744,16.1304187761189));
#64853=CARTESIAN_POINT('Ctrl Pts',(29.7473966610106,-12.5797304055295,16.1152743170362));
#64854=CARTESIAN_POINT('Ctrl Pts',(29.7626545344491,-12.5647687764009,16.1003189928335));
#64855=CARTESIAN_POINT('Ctrl Pts',(29.7762538563399,-12.5489829561878,16.084541176273));
#64856=CARTESIAN_POINT('Ctrl Pts',(29.787997904047,-12.5324961525768,16.0680539360822));
#64857=CARTESIAN_POINT('Ctrl Pts',(29.7895746977067,-12.5302825812383,16.0658403061271));
#64858=CARTESIAN_POINT('Ctrl Pts',(29.791117976733,-12.5280563584413,16.0636138598165));
#64859=CARTESIAN_POINT('Ctrl Pts',(29.79262719669,-12.5258177707357,16.0613748467601));
#64860=CARTESIAN_POINT('Ctrl Pts',(29.7964903838824,-12.5200876030991,16.0556435903428));
#64861=CARTESIAN_POINT('Ctrl Pts',(29.8001304563093,-12.5142764177544,16.0498300026419));
#64862=CARTESIAN_POINT('Ctrl Pts',(29.8035453933447,-12.5083905632827,16.0439410198973));
#64863=CARTESIAN_POINT('Ctrl Pts',(29.8135085249837,-12.4912184917917,16.0267598216216));
#64864=CARTESIAN_POINT('Ctrl Pts',(29.8214801888626,-12.4735473689987,16.0090741392566));
#64865=CARTESIAN_POINT('Ctrl Pts',(29.8274710013099,-12.455552830915,15.9910707602896));
#64866=CARTESIAN_POINT('Ctrl Pts',(29.8335196973064,-12.4373844286454,15.9728934317156));
#64867=CARTESIAN_POINT('Ctrl Pts',(29.8375493041986,-12.4188853503994,15.954391298432));
#64868=CARTESIAN_POINT('Ctrl Pts',(29.8395211658521,-12.4002313289882,15.9357419099974));
#64869=CARTESIAN_POINT('Ctrl Pts',(29.8404142905819,-12.3917822738514,15.9272949532968));
#64870=CARTESIAN_POINT('Ctrl Pts',(29.8408845785222,-12.3833014543909,15.9188176751431));
#64871=CARTESIAN_POINT('Ctrl Pts',(29.8409249324999,-12.3748057049165,15.9103263965022));
#64872=CARTESIAN_POINT('Ctrl Pts',(29.8410141353611,-12.3560257678752,15.8915563422819));
#64873=CARTESIAN_POINT('Ctrl Pts',(29.839005150545,-12.3373242933743,15.8728698715399));
#64874=CARTESIAN_POINT('Ctrl Pts',(29.8348849951903,-12.3188838478478,15.8544395081246));
#64875=CARTESIAN_POINT('Ctrl Pts',(29.8330414088442,-12.3106325683061,15.8461927398794));
#64876=CARTESIAN_POINT('Ctrl Pts',(29.8307744497582,-12.3024335569624,15.8379971208758));
#64877=CARTESIAN_POINT('Ctrl Pts',(29.828079594041,-12.2943035691538,15.8298678492748));
#64878=CARTESIAN_POINT('Ctrl Pts',(29.8221302029723,-12.2763551214691,15.8119209827503));
#64879=CARTESIAN_POINT('Ctrl Pts',(29.8140982090173,-12.2587417299286,15.7942966939978));
#64880=CARTESIAN_POINT('Ctrl Pts',(29.8041111241459,-12.2416040578225,15.777148298582));
#64881=CARTESIAN_POINT('Ctrl Pts',(29.7940809428845,-12.2243924330255,15.759925904202));
#64882=CARTESIAN_POINT('Ctrl Pts',(29.782158514763,-12.2077969859203,15.7433200368196));
#64883=CARTESIAN_POINT('Ctrl Pts',(29.7685166509587,-12.1919504656349,15.7274696634267));
#64884=CARTESIAN_POINT('Ctrl Pts',(29.7547832062128,-12.1759975640465,15.7115128828639));
#64885=CARTESIAN_POINT('Ctrl Pts',(29.7393064495632,-12.1608029018257,15.6963208650584));
#64886=CARTESIAN_POINT('Ctrl Pts',(29.7222165154168,-12.1465218786284,15.6820468667118));
#64887=CARTESIAN_POINT('Ctrl Pts',(29.714456352485,-12.1400371803322,15.6755653582456));
#64888=CARTESIAN_POINT('Ctrl Pts',(29.7063630119465,-12.133741204959,15.6692733727736));
#64889=CARTESIAN_POINT('Ctrl Pts',(29.6979461657047,-12.1276505214833,15.663186817225));
#64890=CARTESIAN_POINT('Ctrl Pts',(29.6830664509242,-12.1168831116564,15.6524267049506));
#64891=CARTESIAN_POINT('Ctrl Pts',(29.6672686286642,-12.106823322986,15.6423747899711));
#64892=CARTESIAN_POINT('Ctrl Pts',(29.6506294745141,-12.0975465700894,15.6331010309531));
#64893=CARTESIAN_POINT('Ctrl Pts',(29.6298333664988,-12.0859522093709,15.6215104120729));
#64894=CARTESIAN_POINT('Ctrl Pts',(29.6077235557432,-12.0755796101762,15.6111339862795));
#64895=CARTESIAN_POINT('Ctrl Pts',(29.5845492431071,-12.0664699003604,15.6020196611318));
#64896=CARTESIAN_POINT('Ctrl Pts',(29.5693077818247,-12.0604785559079,15.5960252812322));
#64897=CARTESIAN_POINT('Ctrl Pts',(29.5536050740522,-12.0550341298654,15.5905773505175));
#64898=CARTESIAN_POINT('Ctrl Pts',(29.5375065797936,-12.0501564727128,15.5856968465475));
#64899=CARTESIAN_POINT('Ctrl Pts',(29.5129698031991,-12.042722113826,15.5782581486383));
#64900=CARTESIAN_POINT('Ctrl Pts',(29.4876554246782,-12.0366454880391,15.5721786672796));
#64901=CARTESIAN_POINT('Ctrl Pts',(29.4618081716839,-12.0319809750165,15.5675131353444));
#64902=CARTESIAN_POINT('Ctrl Pts',(29.4544053482885,-12.030645027783,15.5661768962876));
#64903=CARTESIAN_POINT('Ctrl Pts',(29.4469586955947,-12.0294251369375,15.564956850236));
#64904=CARTESIAN_POINT('Ctrl Pts',(29.4394737482924,-12.0283231275853,15.5638548093301));
#64905=CARTESIAN_POINT('Ctrl Pts',(29.4134898262845,-12.0244975128009,15.5600290850074));
#64906=CARTESIAN_POINT('Ctrl Pts',(29.3871445400212,-12.0221044238458,15.5576374033428));
#64907=CARTESIAN_POINT('Ctrl Pts',(29.3606723115461,-12.0212111743809,15.5567447799941));
#64908=CARTESIAN_POINT('Ctrl Pts',(29.3528735776467,-12.0209480225692,15.5564818126367));
#64909=CARTESIAN_POINT('Ctrl Pts',(29.3450637756841,-12.0208152801713,15.556349186104));
#64910=CARTESIAN_POINT('Ctrl Pts',(29.3372488480671,-12.0208152801713,15.556349186104));
#64911=CARTESIAN_POINT('',(8.,-12.0208152801713,15.556349186104));
#64912=CARTESIAN_POINT('Origin',(5.75,15.3878195049812,11.145178817862));
#64913=CARTESIAN_POINT('',(5.75,15.034266114388,11.4987322084552));
#64914=CARTESIAN_POINT('Origin',(8.,14.7078210486802,11.1722871427475));
#64915=CARTESIAN_POINT('',(29.5,14.7292483497821,11.1937144438494));
#64916=CARTESIAN_POINT('',(25.5,14.7292483497821,11.1937144438494));
#64917=CARTESIAN_POINT('',(30.,15.0859875548336,11.5504536489008));
#64918=CARTESIAN_POINT('Ctrl Pts',(30.,15.0859875548336,11.5504536489008));
#64919=CARTESIAN_POINT('Ctrl Pts',(30.,15.0418438629615,11.5063099570288));
#64920=CARTESIAN_POINT('Ctrl Pts',(29.9854746058202,14.9898767115274,11.4543428055946));
#64921=CARTESIAN_POINT('Ctrl Pts',(29.9380095827943,14.908422575575,11.3728886696422));
#64922=CARTESIAN_POINT('Ctrl Pts',(29.8967622377582,14.8644752333855,11.3289413274527));
#64923=CARTESIAN_POINT('Ctrl Pts',(29.8093392860887,14.8023139816534,11.2667800757207));
#64924=CARTESIAN_POINT('Ctrl Pts',(29.7477912665658,14.7730323227637,11.237498416831));
#64925=CARTESIAN_POINT('Ctrl Pts',(29.6339241856893,14.7395012017362,11.2039672958034));
#64926=CARTESIAN_POINT('Ctrl Pts',(29.5615281526734,14.7292483497821,11.1937144438494));
#64927=CARTESIAN_POINT('Ctrl Pts',(29.5,14.7292483497821,11.1937144438494));
#64928=CARTESIAN_POINT('',(30.,15.7939171599704,12.2583832540376));
#64929=CARTESIAN_POINT('',(30.,12.8627940008233,9.32726009489054));
#64930=CARTESIAN_POINT('Ctrl Pts',(30.,15.7939171599704,12.2583832540376));
#64931=CARTESIAN_POINT('Ctrl Pts',(30.,15.8380021716785,12.3024682657458));
#64932=CARTESIAN_POINT('Ctrl Pts',(29.985486770529,15.8898992445794,12.3543653386467));
#64933=CARTESIAN_POINT('Ctrl Pts',(29.9381460122713,15.9710776301552,12.4355437242224));
#64934=CARTESIAN_POINT('Ctrl Pts',(29.8971736290481,16.0147804613409,12.4792465554081));
#64935=CARTESIAN_POINT('Ctrl Pts',(29.8535533905933,16.0458601314941,12.5103262255613));
#64936=CARTESIAN_POINT('',(29.337248848077,15.5563491860757,12.0208152801996));
#64937=CARTESIAN_POINT('Ctrl Pts',(29.6961022501425,16.1580366172154,12.6225040304245));
#64938=CARTESIAN_POINT('Ctrl Pts',(29.7147933690495,16.1447205114661,12.6091877868512));
#64939=CARTESIAN_POINT('Ctrl Pts',(29.7319458264482,16.1304187761599,12.5948812492331));
#64940=CARTESIAN_POINT('Ctrl Pts',(29.7473966610032,16.1152743170805,12.5797304054849));
#64941=CARTESIAN_POINT('Ctrl Pts',(29.7626545344412,16.1003189928811,12.5647687763529));
#64942=CARTESIAN_POINT('Ctrl Pts',(29.7762538563314,16.0845411763236,12.5489829561367));
#64943=CARTESIAN_POINT('Ctrl Pts',(29.787997904038,16.0680539361356,12.532496152523));
#64944=CARTESIAN_POINT('Ctrl Pts',(29.7895746976977,16.0658403061808,12.5302825811841));
#64945=CARTESIAN_POINT('Ctrl Pts',(29.7911179767239,16.0636138598707,12.5280563583868));
#64946=CARTESIAN_POINT('Ctrl Pts',(29.7926271966808,16.0613748468147,12.5258177706809));
#64947=CARTESIAN_POINT('Ctrl Pts',(29.7964903838731,16.0556435903983,12.5200876030434));
#64948=CARTESIAN_POINT('Ctrl Pts',(29.8001304562998,16.0498300026983,12.5142764176978));
#64949=CARTESIAN_POINT('Ctrl Pts',(29.8035453933351,16.0439410199545,12.5083905632253));
#64950=CARTESIAN_POINT('Ctrl Pts',(29.8135085249737,16.0267598216811,12.4912184917317));
#64951=CARTESIAN_POINT('Ctrl Pts',(29.8214801888522,16.0090741393181,12.4735473689368));
#64952=CARTESIAN_POINT('Ctrl Pts',(29.8274710012993,15.9910707603526,12.4555528308514));
#64953=CARTESIAN_POINT('Ctrl Pts',(29.8335196972955,15.97289343178,12.4373844285801));
#64954=CARTESIAN_POINT('Ctrl Pts',(29.8375493041875,15.9543912984974,12.418885350333));
#64955=CARTESIAN_POINT('Ctrl Pts',(29.8395211658409,15.9357419100632,12.4002313289212));
#64956=CARTESIAN_POINT('Ctrl Pts',(29.8404142905707,15.9272949533631,12.3917822737844));
#64957=CARTESIAN_POINT('Ctrl Pts',(29.8408845785109,15.9188176752096,12.3833014543239));
#64958=CARTESIAN_POINT('Ctrl Pts',(29.8409249324886,15.9103263965689,12.3748057048496));
#64959=CARTESIAN_POINT('Ctrl Pts',(29.8410141353498,15.8915563423485,12.3560257678082));
#64960=CARTESIAN_POINT('Ctrl Pts',(29.8390051505338,15.8728698716057,12.3373242933078));
#64961=CARTESIAN_POINT('Ctrl Pts',(29.8348849951791,15.8544395081892,12.3188838477822));
#64962=CARTESIAN_POINT('Ctrl Pts',(29.8330414088332,15.8461927399437,12.3106325682411));
#64963=CARTESIAN_POINT('Ctrl Pts',(29.8307744497472,15.8379971209396,12.3024335568982));
#64964=CARTESIAN_POINT('Ctrl Pts',(29.8280795940302,15.829867849338,12.2943035690904));
#64965=CARTESIAN_POINT('Ctrl Pts',(29.8221302029618,15.8119209828121,12.2763551214071));
#64966=CARTESIAN_POINT('Ctrl Pts',(29.8140982090071,15.7942966940576,12.2587417298686));
#64967=CARTESIAN_POINT('Ctrl Pts',(29.8041111241361,15.7771482986394,12.2416040577649));
#64968=CARTESIAN_POINT('Ctrl Pts',(29.7940809428751,15.759925904257,12.2243924329705));
#64969=CARTESIAN_POINT('Ctrl Pts',(29.7821585147542,15.7433200368719,12.2077969858681));
#64970=CARTESIAN_POINT('Ctrl Pts',(29.7685166509504,15.727469663476,12.1919504655859));
#64971=CARTESIAN_POINT('Ctrl Pts',(29.7547832062051,15.7115128829102,12.1759975640006));
#64972=CARTESIAN_POINT('Ctrl Pts',(29.7393064495563,15.6963208651015,12.1608029017832));
#64973=CARTESIAN_POINT('Ctrl Pts',(29.7222165154105,15.6820468667515,12.1465218785895));
#64974=CARTESIAN_POINT('Ctrl Pts',(29.7144563524789,15.6755653582836,12.1400371802947));
#64975=CARTESIAN_POINT('Ctrl Pts',(29.7063630119405,15.6692733728098,12.1337412049229));
#64976=CARTESIAN_POINT('Ctrl Pts',(29.6979461656987,15.6631868172595,12.1276505214487));
#64977=CARTESIAN_POINT('Ctrl Pts',(29.6830664509188,15.6524267049823,12.1168831116246));
#64978=CARTESIAN_POINT('Ctrl Pts',(29.6672686286593,15.6423747899999,12.1068233229571));
#64979=CARTESIAN_POINT('Ctrl Pts',(29.6506294745096,15.6331010309793,12.0975465700633));
#64980=CARTESIAN_POINT('Ctrl Pts',(29.629833366495,15.6215104120956,12.0859522093482));
#64981=CARTESIAN_POINT('Ctrl Pts',(29.60772355574,15.6111339862989,12.0755796101569));
#64982=CARTESIAN_POINT('Ctrl Pts',(29.5845492431045,15.6020196611483,12.0664699003441));
#64983=CARTESIAN_POINT('Ctrl Pts',(29.5693077818223,15.5960252812466,12.0604785558936));
#64984=CARTESIAN_POINT('Ctrl Pts',(29.5536050740501,15.59057735053,12.0550341298529));
#64985=CARTESIAN_POINT('Ctrl Pts',(29.5375065797918,15.5856968465582,12.0501564727021));
#64986=CARTESIAN_POINT('Ctrl Pts',(29.5129698031983,15.5782581486466,12.042722113818));
#64987=CARTESIAN_POINT('Ctrl Pts',(29.4876554246784,15.5721786672858,12.0366454880335));
#64988=CARTESIAN_POINT('Ctrl Pts',(29.4618081716851,15.567513135349,12.0319809750126));
#64989=CARTESIAN_POINT('Ctrl Pts',(29.4544053482892,15.5661768962915,12.0306450277795));
#64990=CARTESIAN_POINT('Ctrl Pts',(29.4469586955948,15.5649568502393,12.0294251369344));
#64991=CARTESIAN_POINT('Ctrl Pts',(29.4394737482919,15.5638548093329,12.0283231275825));
#64992=CARTESIAN_POINT('Ctrl Pts',(29.4134898262827,15.5600290850086,12.0244975127992));
#64993=CARTESIAN_POINT('Ctrl Pts',(29.387144540018,15.557637403343,12.022104423845));
#64994=CARTESIAN_POINT('Ctrl Pts',(29.3606723115413,15.5567447799941,12.0212111743806));
#64995=CARTESIAN_POINT('Ctrl Pts',(29.3528735776436,15.5564818126367,12.0209480225691));
#64996=CARTESIAN_POINT('Ctrl Pts',(29.3450637756825,15.556349186104,12.0208152801713));
#64997=CARTESIAN_POINT('Ctrl Pts',(29.3372488480671,15.556349186104,12.0208152801713));
#64998=CARTESIAN_POINT('',(8.,15.556349186104,12.0208152801713));
#64999=CARTESIAN_POINT('Origin',(5.75,11.145178817862,-15.3878195049812));
#65000=CARTESIAN_POINT('',(5.75,11.4987322084552,-15.034266114388));
#65001=CARTESIAN_POINT('Origin',(8.,11.1722871427474,-14.7078210486802));
#65002=CARTESIAN_POINT('',(29.5,11.1937144438493,-14.7292483497821));
#65003=CARTESIAN_POINT('',(25.5,11.1937144438493,-14.7292483497821));
#65004=CARTESIAN_POINT('',(30.,11.5504536489008,-15.0859875548336));
#65005=CARTESIAN_POINT('Ctrl Pts',(30.,11.5504536489008,-15.0859875548336));
#65006=CARTESIAN_POINT('Ctrl Pts',(30.,11.5063099570288,-15.0418438629615));
#65007=CARTESIAN_POINT('Ctrl Pts',(29.9854746058202,11.4543428055946,-14.9898767115274));
#65008=CARTESIAN_POINT('Ctrl Pts',(29.9380095827943,11.3728886696422,-14.908422575575));
#65009=CARTESIAN_POINT('Ctrl Pts',(29.8967622377582,11.3289413274527,-14.8644752333855));
#65010=CARTESIAN_POINT('Ctrl Pts',(29.8093392860887,11.2667800757207,-14.8023139816534));
#65011=CARTESIAN_POINT('Ctrl Pts',(29.7477912665658,11.237498416831,-14.7730323227637));
#65012=CARTESIAN_POINT('Ctrl Pts',(29.6339241856893,11.2039672958034,-14.7395012017362));
#65013=CARTESIAN_POINT('Ctrl Pts',(29.5615281526734,11.1937144438494,-14.7292483497821));
#65014=CARTESIAN_POINT('Ctrl Pts',(29.5,11.1937144438494,-14.7292483497821));
#65015=CARTESIAN_POINT('',(30.,12.2583832540376,-15.7939171599704));
#65016=CARTESIAN_POINT('',(30.,9.32726009489054,-12.8627940008233));
#65017=CARTESIAN_POINT('Ctrl Pts',(30.,12.2583832540376,-15.7939171599704));
#65018=CARTESIAN_POINT('Ctrl Pts',(30.,12.3024682657458,-15.8380021716785));
#65019=CARTESIAN_POINT('Ctrl Pts',(29.985486770529,12.3543653386467,-15.8898992445794));
#65020=CARTESIAN_POINT('Ctrl Pts',(29.9381460122713,12.4355437242224,-15.9710776301552));
#65021=CARTESIAN_POINT('Ctrl Pts',(29.8971736290481,12.4792465554081,-16.0147804613409));
#65022=CARTESIAN_POINT('Ctrl Pts',(29.8535533905933,12.5103262255613,-16.0458601314941));
#65023=CARTESIAN_POINT('',(29.337248848077,12.0208152801996,-15.5563491860757));
#65024=CARTESIAN_POINT('Ctrl Pts',(29.6961022501482,12.6225040304587,-16.1580366171813));
#65025=CARTESIAN_POINT('Ctrl Pts',(29.7147933690559,12.6091877868889,-16.1447205114284));
#65026=CARTESIAN_POINT('Ctrl Pts',(29.7319458264552,12.5948812492743,-16.1304187761187));
#65027=CARTESIAN_POINT('Ctrl Pts',(29.7473966610108,12.5797304055293,-16.115274317036));
#65028=CARTESIAN_POINT('Ctrl Pts',(29.7626545344494,12.5647687764006,-16.1003189928333));
#65029=CARTESIAN_POINT('Ctrl Pts',(29.7762538563401,12.5489829561875,-16.0845411762727));
#65030=CARTESIAN_POINT('Ctrl Pts',(29.7879979040472,12.5324961525765,-16.0680539360819));
#65031=CARTESIAN_POINT('Ctrl Pts',(29.7895746977069,12.530282581238,-16.0658403061268));
#65032=CARTESIAN_POINT('Ctrl Pts',(29.7911179767331,12.5280563584412,-16.0636138598164));
#65033=CARTESIAN_POINT('Ctrl Pts',(29.79262719669,12.5258177707357,-16.0613748467601));
#65034=CARTESIAN_POINT('Ctrl Pts',(29.7964903838824,12.5200876030991,-16.0556435903428));
#65035=CARTESIAN_POINT('Ctrl Pts',(29.8001304563093,12.5142764177544,-16.0498300026419));
#65036=CARTESIAN_POINT('Ctrl Pts',(29.8035453933447,12.5083905632827,-16.0439410198973));
#65037=CARTESIAN_POINT('Ctrl Pts',(29.8135085249837,12.4912184917917,-16.0267598216216));
#65038=CARTESIAN_POINT('Ctrl Pts',(29.8214801888625,12.4735473689988,-16.0090741392567));
#65039=CARTESIAN_POINT('Ctrl Pts',(29.8274710013099,12.4555528309151,-15.9910707602897));
#65040=CARTESIAN_POINT('Ctrl Pts',(29.8335196973064,12.4373844286455,-15.9728934317157));
#65041=CARTESIAN_POINT('Ctrl Pts',(29.8375493041985,12.4188853503995,-15.9543912984321));
#65042=CARTESIAN_POINT('Ctrl Pts',(29.8395211658521,12.4002313289884,-15.9357419099975));
#65043=CARTESIAN_POINT('Ctrl Pts',(29.8404142905819,12.3917822738516,-15.927294953297));
#65044=CARTESIAN_POINT('Ctrl Pts',(29.8408845785222,12.3833014543909,-15.9188176751432));
#65045=CARTESIAN_POINT('Ctrl Pts',(29.8409249324999,12.3748057049165,-15.9103263965022));
#65046=CARTESIAN_POINT('Ctrl Pts',(29.8410141353611,12.356025767875,-15.8915563422818));
#65047=CARTESIAN_POINT('Ctrl Pts',(29.839005150545,12.3373242933741,-15.8728698715396));
#65048=CARTESIAN_POINT('Ctrl Pts',(29.8348849951902,12.3188838478474,-15.8544395081242));
#65049=CARTESIAN_POINT('Ctrl Pts',(29.8330414088442,12.3106325683058,-15.8461927398792));
#65050=CARTESIAN_POINT('Ctrl Pts',(29.8307744497581,12.3024335569623,-15.8379971208756));
#65051=CARTESIAN_POINT('Ctrl Pts',(29.828079594041,12.2943035691539,-15.8298678492748));
#65052=CARTESIAN_POINT('Ctrl Pts',(29.8221302029723,12.2763551214691,-15.8119209827503));
#65053=CARTESIAN_POINT('Ctrl Pts',(29.8140982090173,12.2587417299286,-15.7942966939978));
#65054=CARTESIAN_POINT('Ctrl Pts',(29.8041111241459,12.2416040578225,-15.777148298582));
#65055=CARTESIAN_POINT('Ctrl Pts',(29.7940809428845,12.2243924330256,-15.759925904202));
#65056=CARTESIAN_POINT('Ctrl Pts',(29.7821585147631,12.2077969859204,-15.7433200368197));
#65057=CARTESIAN_POINT('Ctrl Pts',(29.7685166509588,12.1919504656351,-15.7274696634269));
#65058=CARTESIAN_POINT('Ctrl Pts',(29.754783206213,12.1759975640467,-15.7115128828641));
#65059=CARTESIAN_POINT('Ctrl Pts',(29.7393064495636,12.160802901826,-15.6963208650588));
#65060=CARTESIAN_POINT('Ctrl Pts',(29.7222165154172,12.1465218786288,-15.6820468667122));
#65061=CARTESIAN_POINT('Ctrl Pts',(29.7144563524853,12.1400371803324,-15.6755653582458));
#65062=CARTESIAN_POINT('Ctrl Pts',(29.7063630119467,12.1337412049591,-15.6692733727737));
#65063=CARTESIAN_POINT('Ctrl Pts',(29.6979461657046,12.1276505214833,-15.663186817225));
#65064=CARTESIAN_POINT('Ctrl Pts',(29.6830664509242,12.1168831116564,-15.6524267049506));
#65065=CARTESIAN_POINT('Ctrl Pts',(29.6672686286642,12.106823322986,-15.6423747899711));
#65066=CARTESIAN_POINT('Ctrl Pts',(29.6506294745141,12.0975465700894,-15.6331010309531));
#65067=CARTESIAN_POINT('Ctrl Pts',(29.6298333664989,12.085952209371,-15.6215104120729));
#65068=CARTESIAN_POINT('Ctrl Pts',(29.6077235557434,12.0755796101763,-15.6111339862796));
#65069=CARTESIAN_POINT('Ctrl Pts',(29.5845492431074,12.0664699003605,-15.602019661132));
#65070=CARTESIAN_POINT('Ctrl Pts',(29.5693077818249,12.060478555908,-15.5960252812323));
#65071=CARTESIAN_POINT('Ctrl Pts',(29.5536050740523,12.0550341298654,-15.5905773505176));
#65072=CARTESIAN_POINT('Ctrl Pts',(29.5375065797936,12.0501564727128,-15.5856968465475));
#65073=CARTESIAN_POINT('Ctrl Pts',(29.5129698031991,12.042722113826,-15.5782581486383));
#65074=CARTESIAN_POINT('Ctrl Pts',(29.4876554246782,12.0366454880391,-15.5721786672796));
#65075=CARTESIAN_POINT('Ctrl Pts',(29.4618081716839,12.0319809750165,-15.5675131353444));
#65076=CARTESIAN_POINT('Ctrl Pts',(29.4544053482885,12.0306450277829,-15.5661768962876));
#65077=CARTESIAN_POINT('Ctrl Pts',(29.4469586955947,12.0294251369375,-15.564956850236));
#65078=CARTESIAN_POINT('Ctrl Pts',(29.4394737482924,12.0283231275853,-15.5638548093301));
#65079=CARTESIAN_POINT('Ctrl Pts',(29.413489826283,12.0244975128006,-15.5600290850072));
#65080=CARTESIAN_POINT('Ctrl Pts',(29.3871445400181,12.0221044238455,-15.5576374033425));
#65081=CARTESIAN_POINT('Ctrl Pts',(29.3606723115414,12.0212111743808,-15.556744779994));
#65082=CARTESIAN_POINT('Ctrl Pts',(29.3528735776436,12.0209480225692,-15.5564818126366));
#65083=CARTESIAN_POINT('Ctrl Pts',(29.3450637756825,12.0208152801713,-15.556349186104));
#65084=CARTESIAN_POINT('Ctrl Pts',(29.3372488480671,12.0208152801713,-15.556349186104));
#65085=CARTESIAN_POINT('',(8.,12.0208152801713,-15.556349186104));
#65086=CARTESIAN_POINT('Origin',(29.5,-0.147970773009215,-4.39061146012847));
#65087=CARTESIAN_POINT('',(29.988172366943,-12.0208153231845,-16.1105655469847));
#65088=CARTESIAN_POINT('',(30.,-11.8557283302283,-16.0983690173476));
#65089=CARTESIAN_POINT('Ctrl Pts',(29.9881723667624,-12.0208153202678,-16.1105655869574));
#65090=CARTESIAN_POINT('Ctrl Pts',(29.9959139993979,-11.9675244706852,-16.1067121202485));
#65091=CARTESIAN_POINT('Ctrl Pts',(29.9997996576908,-11.913571858627,-16.1027290501183));
#65092=CARTESIAN_POINT('Ctrl Pts',(29.9999974820111,-11.8585310768755,-16.0985804389105));
#65093=CARTESIAN_POINT('Ctrl Pts',(30.,-11.8571296997207,-16.0984747560115));
#65094=CARTESIAN_POINT('Ctrl Pts',(30.,-11.8557283302283,-16.0983690173476));
#65095=CARTESIAN_POINT('',(30.,-11.145178817862,-15.3878195049812));
#65096=CARTESIAN_POINT('',(30.,-0.147970773009215,-4.39061146012847));
#65097=CARTESIAN_POINT('',(29.5,-11.4987322084552,-15.034266114388));
#65098=CARTESIAN_POINT('Origin',(29.5,-11.145178817862,-15.3878195049812));
#65099=CARTESIAN_POINT('',(29.5,-12.0208152801713,-15.556349186104));
#65100=CARTESIAN_POINT('',(29.5,-0.501524163602491,-4.0370580695352));
#65101=CARTESIAN_POINT('Origin',(29.5,-12.0208152801713,-16.2634559672906));
#65102=CARTESIAN_POINT('Origin',(29.5,0.,0.));
#65103=CARTESIAN_POINT('',(29.5,-10.8518846384445,-14.9828768864291));
#65104=CARTESIAN_POINT('Origin',(29.5,0.,0.));
#65105=CARTESIAN_POINT('Origin',(29.5,-11.145178817862,-15.3878195049812));
#65106=CARTESIAN_POINT('Origin',(30.,0.,0.));
#65107=CARTESIAN_POINT('Origin',(29.5,-11.145178817862,-15.3878195049812));
#65108=CARTESIAN_POINT('Origin',(29.5,-11.145178817862,-15.3878195049812));
#65109=CARTESIAN_POINT('Origin',(25.5,-11.145178817862,-15.3878195049812));
#65110=CARTESIAN_POINT('',(25.5,-10.8518846384445,-14.9828768864291));
#65111=CARTESIAN_POINT('',(25.5,-11.4987322084552,-15.034266114388));
#65112=CARTESIAN_POINT('Origin',(25.5,0.,0.));
#65113=CARTESIAN_POINT('Origin',(30.,18.5,0.));
#65114=CARTESIAN_POINT('Origin',(30.,0.,0.));
#65115=CARTESIAN_POINT('Ctrl Pts',(29.3372488480671,15.556349186104,-12.0208152801713));
#65116=CARTESIAN_POINT('Ctrl Pts',(29.5429564710669,14.3836353036043,-13.1935291626711));
#65117=CARTESIAN_POINT('Ctrl Pts',(29.5429564710669,13.1935291626711,-14.3836353036043));
#65118=CARTESIAN_POINT('Ctrl Pts',(29.3372488480671,12.0208152801713,-15.556349186104));
#65119=CARTESIAN_POINT('Ctrl Pts',(29.4482318142554,15.5660830361542,-12.0110814301211));
#65120=CARTESIAN_POINT('Ctrl Pts',(29.6555084018099,14.3871511086965,-13.1900026135806));
#65121=CARTESIAN_POINT('Ctrl Pts',(29.6555084018099,13.1900026135806,-14.3871511086965));
#65122=CARTESIAN_POINT('Ctrl Pts',(29.4482318142554,12.0110814301211,-15.5660830361542));
#65123=CARTESIAN_POINT('Ctrl Pts',(29.6698854043403,15.640712881006,-12.0468306632344));
#65124=CARTESIAN_POINT('Ctrl Pts',(29.8803030333723,14.449846680584,-13.2386772974356));
#65125=CARTESIAN_POINT('Ctrl Pts',(29.8803030333723,13.2386772974356,-14.449846680584));
#65126=CARTESIAN_POINT('Ctrl Pts',(29.6698854043403,12.0468306632344,-15.640712881006));
#65127=CARTESIAN_POINT('Ctrl Pts',(29.8584164372574,15.8692592876068,-12.2423065389736));
#65128=CARTESIAN_POINT('Ctrl Pts',(30.070315495024,14.6693103047466,-13.446404317352));
#65129=CARTESIAN_POINT('Ctrl Pts',(30.070315495024,13.446404317352,-14.6693103047466));
#65130=CARTESIAN_POINT('Ctrl Pts',(29.8584164372574,12.2423065389736,-15.8692592876068));
#65131=CARTESIAN_POINT('Ctrl Pts',(29.826995289044,16.074348363723,-12.4529072490931));
#65132=CARTESIAN_POINT('Ctrl Pts',(30.0363416090412,14.876799813501,-13.6562728118144));
#65133=CARTESIAN_POINT('Ctrl Pts',(30.0363416090412,13.6562728118144,-14.876799813501));
#65134=CARTESIAN_POINT('Ctrl Pts',(29.826995289044,12.4529072490931,-16.074348363723));
#65135=CARTESIAN_POINT('Ctrl Pts',(29.7297376388611,16.1642229909118,-12.5598419966883));
#65136=CARTESIAN_POINT('Ctrl Pts',(29.9363897461384,14.9718056381716,-13.7576323115672));
#65137=CARTESIAN_POINT('Ctrl Pts',(29.9363897461384,13.7576323115672,-14.9718056381716));
#65138=CARTESIAN_POINT('Ctrl Pts',(29.7297376388611,12.5598419966883,-16.1642229909118));
#65139=CARTESIAN_POINT('Ctrl Pts',(29.6908022386604,16.188980729523,-12.5914294562957));
#65140=CARTESIAN_POINT('Ctrl Pts',(29.8965098616602,14.9985443441187,-13.7869294139585));
#65141=CARTESIAN_POINT('Ctrl Pts',(29.8965098616602,13.7869294139585,-14.9985443441187));
#65142=CARTESIAN_POINT('Ctrl Pts',(29.6908022386603,12.5914294562957,-16.188980729523));
#65143=CARTESIAN_POINT('',(29.337248848077,15.5563491860757,-12.0208152801996));
#65144=CARTESIAN_POINT('Ctrl Pts',(29.3372488480671,15.556349186104,-12.0208152801713));
#65145=CARTESIAN_POINT('Ctrl Pts',(29.3635470277545,15.556349186104,-12.0208152801713));
#65146=CARTESIAN_POINT('Ctrl Pts',(29.3897411711777,15.5578483797221,-12.0223153633457));
#65147=CARTESIAN_POINT('Ctrl Pts',(29.4156074313478,15.5607573876035,-12.025224866541));
#65148=CARTESIAN_POINT('Ctrl Pts',(29.4419059568767,15.5637150095221,-12.028182992051));
#65149=CARTESIAN_POINT('Ctrl Pts',(29.467866856786,15.5681303086141,-12.0325981572563));
#65150=CARTESIAN_POINT('Ctrl Pts',(29.4932488211195,15.5739465388181,-12.0384121343));
#65151=CARTESIAN_POINT('Ctrl Pts',(29.5056295238222,15.5767835539545,-12.0412480503998));
#65152=CARTESIAN_POINT('Ctrl Pts',(29.5178722688873,15.5799544093323,-12.0444173222812));
#65153=CARTESIAN_POINT('Ctrl Pts',(29.5299470752187,15.583455268401,-12.0479161878428));
#65154=CARTESIAN_POINT('Ctrl Pts',(29.5545920296303,15.5906006014012,-12.0550574520495));
#65155=CARTESIAN_POINT('Ctrl Pts',(29.5783543573545,15.5990651907424,-12.0635161276693));
#65156=CARTESIAN_POINT('Ctrl Pts',(29.6010013147618,15.6087800031665,-12.0732271832591));
#65157=CARTESIAN_POINT('Ctrl Pts',(29.6182267197664,15.6161691449192,-12.0806134675421));
#65158=CARTESIAN_POINT('Ctrl Pts',(29.6348068591537,15.6242823638657,-12.088725060339));
#65159=CARTESIAN_POINT('Ctrl Pts',(29.6506294743827,15.6331010317096,-12.0975465693321));
#65160=CARTESIAN_POINT('Ctrl Pts',(29.6654204617342,15.6413447261084,-12.1057929196383));
#65161=CARTESIAN_POINT('Ctrl Pts',(29.6795495016548,15.6502051489965,-12.1146598899589));
#65162=CARTESIAN_POINT('Ctrl Pts',(29.6929623869868,15.6596335337639,-12.1240948005337));
#65163=CARTESIAN_POINT('Ctrl Pts',(29.7117060225645,15.6728090887466,-12.137279474908));
#65164=CARTESIAN_POINT('Ctrl Pts',(29.7289079510238,15.6869909143398,-12.1514701037918));
#65165=CARTESIAN_POINT('Ctrl Pts',(29.7444572668983,15.702017054145,-12.166498860769));
#65166=CARTESIAN_POINT('Ctrl Pts',(29.7600106951579,15.7170471679691,-12.1815315924573));
#65167=CARTESIAN_POINT('Ctrl Pts',(29.7739113767471,15.7329229381329,-12.1974036551066));
#65168=CARTESIAN_POINT('Ctrl Pts',(29.7860080855888,15.749500306549,-12.2139724870497));
#65169=CARTESIAN_POINT('Ctrl Pts',(29.7916649639638,15.757252510734,-12.2217206992573));
#65170=CARTESIAN_POINT('Ctrl Pts',(29.7969266990437,15.7651583176022,-12.2296215756395));
#65171=CARTESIAN_POINT('Ctrl Pts',(29.8017740895379,15.7732035030496,-12.2376617309556));
#65172=CARTESIAN_POINT('Ctrl Pts',(29.8121759038527,15.7904673329913,-12.2549147669471));
#65173=CARTESIAN_POINT('Ctrl Pts',(29.8205897043228,15.8082344071429,-12.2726701274951));
#65174=CARTESIAN_POINT('Ctrl Pts',(29.8268838981079,15.8263459587283,-12.2907815682763));
#65175=CARTESIAN_POINT('Ctrl Pts',(29.827291378433,15.8275184839444,-12.2919540863191));
#65176=CARTESIAN_POINT('Ctrl Pts',(29.8276899587891,15.8286924566664,-12.2931281036774));
#65177=CARTESIAN_POINT('Ctrl Pts',(29.828079596474,15.8298678351315,-12.2943035833427));
#65178=CARTESIAN_POINT('Ctrl Pts',(29.8341018209648,15.8480344377277,-12.3124717500857));
#65179=CARTESIAN_POINT('Ctrl Pts',(29.8379920903099,15.8665369818828,-12.3309885243672));
#65180=CARTESIAN_POINT('Ctrl Pts',(29.8397834072957,15.8852056234607,-12.3496695928252));
#65181=CARTESIAN_POINT('Ctrl Pts',(29.8404573868545,15.8922296638259,-12.35669830878));
#65182=CARTESIAN_POINT('Ctrl Pts',(29.8408337073058,15.8992771858287,-12.3637503539203));
#65183=CARTESIAN_POINT('Ctrl Pts',(29.8409122430589,15.9063388639742,-12.3708160008987));
#65184=CARTESIAN_POINT('Ctrl Pts',(29.8411201875827,15.9250365556903,-12.3895242011671));
#65185=CARTESIAN_POINT('Ctrl Pts',(29.8392425388012,15.9436833457942,-12.4081767974889));
#65186=CARTESIAN_POINT('Ctrl Pts',(29.8353415852832,15.9621050095651,-12.4265962128555));
#65187=CARTESIAN_POINT('Ctrl Pts',(29.8314529328993,15.9804685830881,-12.4449575450642));
#65188=CARTESIAN_POINT('Ctrl Pts',(29.8255535219269,15.9986093925319,-12.4630881464303));
#65189=CARTESIAN_POINT('Ctrl Pts',(29.8176551502792,16.0163472264769,-12.4808142028385));
#65190=CARTESIAN_POINT('Ctrl Pts',(29.8141109427718,16.0243066600206,-12.4887683514911));
#65191=CARTESIAN_POINT('Ctrl Pts',(29.8101635813163,16.0321847641428,-12.4966409818456));
#65192=CARTESIAN_POINT('Ctrl Pts',(29.8058109922358,16.0399639788694,-12.5044157250402));
#65193=CARTESIAN_POINT('Ctrl Pts',(29.801757028854,16.0472094713927,-12.5116570528179));
#65194=CARTESIAN_POINT('Ctrl Pts',(29.7973617576402,16.0543508658634,-12.5187951035103));
#65195=CARTESIAN_POINT('Ctrl Pts',(29.7926271891742,16.0613748908717,-12.5258177264253));
#65196=CARTESIAN_POINT('Ctrl Pts',(29.7829544505351,16.0757249966074,-12.5401649676799));
#65197=CARTESIAN_POINT('Ctrl Pts',(29.7718670650277,16.0895860216454,-12.5540309525354));
#65198=CARTESIAN_POINT('Ctrl Pts',(29.7594824084483,16.1028820335097,-12.5673324817292));
#65199=CARTESIAN_POINT('Ctrl Pts',(29.7449214392272,16.1185145073112,-12.5829714424013));
#65200=CARTESIAN_POINT('Ctrl Pts',(29.7286275829019,16.1333027723524,-12.5977667683923));
#65201=CARTESIAN_POINT('Ctrl Pts',(29.7107932614059,16.1471218329996,-12.6115882201639));
#65202=CARTESIAN_POINT('Ctrl Pts',(29.7060063962282,16.1508309721568,-12.6152980011167));
#65203=CARTESIAN_POINT('Ctrl Pts',(29.7011083138909,16.1544701493559,-12.6189375257217));
#65204=CARTESIAN_POINT('Ctrl Pts',(29.6961022501482,16.1580366171813,-12.6225040304587));
#65205=CARTESIAN_POINT('Ctrl Pts',(29.3372488480671,15.556349186104,-12.0208152801713));
#65206=CARTESIAN_POINT('Ctrl Pts',(29.5429564710669,14.3836353036043,-13.1935291626711));
#65207=CARTESIAN_POINT('Ctrl Pts',(29.5429564710669,13.1935291626711,-14.3836353036043));
#65208=CARTESIAN_POINT('Ctrl Pts',(29.3372488480671,12.0208152801713,-15.556349186104));
#65209=CARTESIAN_POINT('Origin',(8.,12.0208152801713,-15.556349186104));
#65210=CARTESIAN_POINT('',(8.,15.556349186104,-12.0208152801713));
#65211=CARTESIAN_POINT('Origin',(29.5,0.,0.));
#65212=CARTESIAN_POINT('',(30.,15.7939171599704,-12.2583832540376));
#65213=CARTESIAN_POINT('Ctrl Pts',(29.8535533905933,16.0458601314941,-12.5103262255613));
#65214=CARTESIAN_POINT('Ctrl Pts',(29.8971736290481,16.0147804613409,-12.4792465554081));
#65215=CARTESIAN_POINT('Ctrl Pts',(29.9381460122713,15.9710776301552,-12.4355437242224));
#65216=CARTESIAN_POINT('Ctrl Pts',(29.985486770529,15.8898992445794,-12.3543653386467));
#65217=CARTESIAN_POINT('Ctrl Pts',(30.,15.8380021716785,-12.3024682657458));
#65218=CARTESIAN_POINT('Ctrl Pts',(30.,15.7939171599704,-12.2583832540376));
#65219=CARTESIAN_POINT('Origin',(30.,0.,0.));
#65220=CARTESIAN_POINT('Origin',(30.,18.5,0.));
#65221=CARTESIAN_POINT('',(30.,15.0859875548336,-11.5504536489008));
#65222=CARTESIAN_POINT('',(30.,13.2870580695352,-9.75152416360247));
#65223=CARTESIAN_POINT('Origin',(30.,0.,0.));
#65224=CARTESIAN_POINT('Origin',(29.5,0.,0.));
#65225=CARTESIAN_POINT('',(29.5,14.7292483497821,-11.1937144438494));
#65226=CARTESIAN_POINT('Origin',(29.5,0.,0.));
#65227=CARTESIAN_POINT('Ctrl Pts',(29.5,14.7292483497821,-11.1937144438494));
#65228=CARTESIAN_POINT('Ctrl Pts',(29.5615281526734,14.7292483497821,-11.1937144438494));
#65229=CARTESIAN_POINT('Ctrl Pts',(29.6339241856893,14.7395012017362,-11.2039672958035));
#65230=CARTESIAN_POINT('Ctrl Pts',(29.7477912665658,14.7730323227637,-11.237498416831));
#65231=CARTESIAN_POINT('Ctrl Pts',(29.8093392860887,14.8023139816534,-11.2667800757207));
#65232=CARTESIAN_POINT('Ctrl Pts',(29.8967622377582,14.8644752333855,-11.3289413274527));
#65233=CARTESIAN_POINT('Ctrl Pts',(29.9380095827943,14.908422575575,-11.3728886696422));
#65234=CARTESIAN_POINT('Ctrl Pts',(29.9854746058202,14.9898767115274,-11.4543428055946));
#65235=CARTESIAN_POINT('Ctrl Pts',(30.,15.0418438629615,-11.5063099570288));
#65236=CARTESIAN_POINT('Ctrl Pts',(30.,15.0859875548336,-11.5504536489008));
#65237=CARTESIAN_POINT('Ctrl Pts',(29.3372488480671,12.0208152801713,15.556349186104));
#65238=CARTESIAN_POINT('Ctrl Pts',(29.5429564635396,13.1935291197589,14.3836353465164));
#65239=CARTESIAN_POINT('Ctrl Pts',(29.5429564785937,14.383635260695,13.1935292055803));
#65240=CARTESIAN_POINT('Ctrl Pts',(29.3372488480671,15.556349186104,12.0208152801713));
#65241=CARTESIAN_POINT('Ctrl Pts',(29.4482318142554,12.0110814301211,15.5660830361542));
#65242=CARTESIAN_POINT('Ctrl Pts',(29.6555083942252,13.1900025704413,14.3871511518362));
#65243=CARTESIAN_POINT('Ctrl Pts',(29.6555084093941,14.3871510655598,13.190002656717));
#65244=CARTESIAN_POINT('Ctrl Pts',(29.4482318142554,15.5660830361542,12.0110814301211));
#65245=CARTESIAN_POINT('Ctrl Pts',(29.6698854043403,12.0468306632344,15.640712881006));
#65246=CARTESIAN_POINT('Ctrl Pts',(29.8803030256726,13.2386772538233,14.4498467241604));
#65247=CARTESIAN_POINT('Ctrl Pts',(29.8803030410714,14.4498466370106,13.2386773410449));
#65248=CARTESIAN_POINT('Ctrl Pts',(29.6698854043403,15.640712881006,12.0468306632344));
#65249=CARTESIAN_POINT('Ctrl Pts',(29.8584164372574,12.2423065389736,15.8692592876068));
#65250=CARTESIAN_POINT('Ctrl Pts',(30.0703154872701,13.4464042732914,14.6693103486554));
#65251=CARTESIAN_POINT('Ctrl Pts',(30.0703155027773,14.6693102608408,13.4464043614096));
#65252=CARTESIAN_POINT('Ctrl Pts',(29.8584164372574,15.8692592876068,12.2423065389736));
#65253=CARTESIAN_POINT('Ctrl Pts',(29.826995289044,12.4529072490931,16.074348363723));
#65254=CARTESIAN_POINT('Ctrl Pts',(30.0363416013808,13.6562727677806,14.8767998573219));
#65255=CARTESIAN_POINT('Ctrl Pts',(30.0363416167011,14.8767997696831,13.6562728558452));
#65256=CARTESIAN_POINT('Ctrl Pts',(29.826995289044,16.074348363723,12.4529072490931));
#65257=CARTESIAN_POINT('Ctrl Pts',(29.7297376388611,12.5598419966883,16.1642229909118));
#65258=CARTESIAN_POINT('Ctrl Pts',(29.9363897385765,13.7576322677374,14.9718056818048));
#65259=CARTESIAN_POINT('Ctrl Pts',(29.9363897536997,14.9718055945414,13.7576323553939));
#65260=CARTESIAN_POINT('Ctrl Pts',(29.7297376388611,16.1642229909118,12.5598419966883));
#65261=CARTESIAN_POINT('Ctrl Pts',(29.6908022386603,12.5914294562957,16.188980729523));
#65262=CARTESIAN_POINT('Ctrl Pts',(29.8965098541329,13.7869293702126,14.9985443876794));
#65263=CARTESIAN_POINT('Ctrl Pts',(29.8965098691869,14.998544300561,13.7869294577015));
#65264=CARTESIAN_POINT('Ctrl Pts',(29.6908022386603,16.188980729523,12.5914294562957));
#65265=CARTESIAN_POINT('Ctrl Pts',(29.3372488480671,12.0208152801713,15.556349186104));
#65266=CARTESIAN_POINT('Ctrl Pts',(29.5429564635396,13.1935291197589,14.3836353465164));
#65267=CARTESIAN_POINT('Ctrl Pts',(29.5429564785937,14.383635260695,13.1935292055803));
#65268=CARTESIAN_POINT('Ctrl Pts',(29.3372488480671,15.556349186104,12.0208152801713));
#65269=CARTESIAN_POINT('Origin',(8.,15.556349186104,12.0208152801713));
#65270=CARTESIAN_POINT('Origin',(29.5,0.,0.));
#65271=CARTESIAN_POINT('Origin',(30.,0.,0.));
#65272=CARTESIAN_POINT('Origin',(30.,18.5,0.));
#65273=CARTESIAN_POINT('Origin',(30.,0.,0.));
#65274=CARTESIAN_POINT('Origin',(29.5,0.,0.));
#65275=CARTESIAN_POINT('Origin',(29.5,0.,0.));
#65276=CARTESIAN_POINT('Ctrl Pts',(29.3372488480671,-15.556349186104,12.0208152801713));
#65277=CARTESIAN_POINT('Ctrl Pts',(29.5429564710669,-14.3836353036043,13.1935291626711));
#65278=CARTESIAN_POINT('Ctrl Pts',(29.5429564710669,-13.1935291626711,14.3836353036043));
#65279=CARTESIAN_POINT('Ctrl Pts',(29.3372488480671,-12.0208152801713,15.556349186104));
#65280=CARTESIAN_POINT('Ctrl Pts',(29.4482318142553,-15.5660830361542,12.0110814301211));
#65281=CARTESIAN_POINT('Ctrl Pts',(29.6555084018099,-14.3871511086965,13.1900026135806));
#65282=CARTESIAN_POINT('Ctrl Pts',(29.6555084018099,-13.1900026135806,14.3871511086965));
#65283=CARTESIAN_POINT('Ctrl Pts',(29.4482318142553,-12.0110814301211,15.5660830361542));
#65284=CARTESIAN_POINT('Ctrl Pts',(29.6698854043403,-15.640712881006,12.0468306632344));
#65285=CARTESIAN_POINT('Ctrl Pts',(29.8803030333723,-14.449846680584,13.2386772974356));
#65286=CARTESIAN_POINT('Ctrl Pts',(29.8803030333723,-13.2386772974356,14.449846680584));
#65287=CARTESIAN_POINT('Ctrl Pts',(29.6698854043403,-12.0468306632344,15.640712881006));
#65288=CARTESIAN_POINT('Ctrl Pts',(29.8584164372574,-15.8692592876068,12.2423065389736));
#65289=CARTESIAN_POINT('Ctrl Pts',(30.070315495024,-14.6693103047466,13.446404317352));
#65290=CARTESIAN_POINT('Ctrl Pts',(30.070315495024,-13.446404317352,14.6693103047466));
#65291=CARTESIAN_POINT('Ctrl Pts',(29.8584164372574,-12.2423065389736,15.8692592876068));
#65292=CARTESIAN_POINT('Ctrl Pts',(29.826995289044,-16.074348363723,12.4529072490931));
#65293=CARTESIAN_POINT('Ctrl Pts',(30.0363416090412,-14.876799813501,13.6562728118144));
#65294=CARTESIAN_POINT('Ctrl Pts',(30.0363416090412,-13.6562728118144,14.876799813501));
#65295=CARTESIAN_POINT('Ctrl Pts',(29.826995289044,-12.4529072490931,16.074348363723));
#65296=CARTESIAN_POINT('Ctrl Pts',(29.7297376388611,-16.1642229909118,12.5598419966883));
#65297=CARTESIAN_POINT('Ctrl Pts',(29.9363897461384,-14.9718056381716,13.7576323115672));
#65298=CARTESIAN_POINT('Ctrl Pts',(29.9363897461384,-13.7576323115672,14.9718056381716));
#65299=CARTESIAN_POINT('Ctrl Pts',(29.7297376388611,-12.5598419966883,16.1642229909118));
#65300=CARTESIAN_POINT('Ctrl Pts',(29.6908022386603,-16.188980729523,12.5914294562957));
#65301=CARTESIAN_POINT('Ctrl Pts',(29.8965098616602,-14.9985443441187,13.7869294139585));
#65302=CARTESIAN_POINT('Ctrl Pts',(29.8965098616602,-13.7869294139585,14.9985443441187));
#65303=CARTESIAN_POINT('Ctrl Pts',(29.6908022386603,-12.5914294562957,16.188980729523));
#65304=CARTESIAN_POINT('',(29.337248848077,-15.5563491860757,12.0208152801996));
#65305=CARTESIAN_POINT('Ctrl Pts',(29.3372488480671,-15.556349186104,12.0208152801713));
#65306=CARTESIAN_POINT('Ctrl Pts',(29.3635470277544,-15.556349186104,12.0208152801713));
#65307=CARTESIAN_POINT('Ctrl Pts',(29.3897411711776,-15.5578483797221,12.0223153633457));
#65308=CARTESIAN_POINT('Ctrl Pts',(29.4156074313478,-15.5607573876035,12.025224866541));
#65309=CARTESIAN_POINT('Ctrl Pts',(29.4419059568766,-15.5637150095221,12.028182992051));
#65310=CARTESIAN_POINT('Ctrl Pts',(29.4678668567859,-15.5681303086141,12.0325981572563));
#65311=CARTESIAN_POINT('Ctrl Pts',(29.4932488211195,-15.5739465388181,12.0384121343));
#65312=CARTESIAN_POINT('Ctrl Pts',(29.5056295238221,-15.5767835539545,12.0412480503998));
#65313=CARTESIAN_POINT('Ctrl Pts',(29.5178722688873,-15.5799544093323,12.0444173222812));
#65314=CARTESIAN_POINT('Ctrl Pts',(29.5299470752186,-15.583455268401,12.0479161878428));
#65315=CARTESIAN_POINT('Ctrl Pts',(29.5545920296302,-15.5906006014011,12.0550574520495));
#65316=CARTESIAN_POINT('Ctrl Pts',(29.5783543573544,-15.5990651907424,12.0635161276693));
#65317=CARTESIAN_POINT('Ctrl Pts',(29.6010013147616,-15.6087800031665,12.073227183259));
#65318=CARTESIAN_POINT('Ctrl Pts',(29.6182267197663,-15.6161691449192,12.0806134675421));
#65319=CARTESIAN_POINT('Ctrl Pts',(29.6348068591536,-15.6242823638657,12.088725060339));
#65320=CARTESIAN_POINT('Ctrl Pts',(29.6506294743827,-15.6331010317096,12.0975465693321));
#65321=CARTESIAN_POINT('Ctrl Pts',(29.6654204617342,-15.6413447261084,12.1057929196383));
#65322=CARTESIAN_POINT('Ctrl Pts',(29.6795495016547,-15.6502051489965,12.1146598899589));
#65323=CARTESIAN_POINT('Ctrl Pts',(29.6929623869867,-15.6596335337639,12.1240948005337));
#65324=CARTESIAN_POINT('Ctrl Pts',(29.7117060225645,-15.6728090887465,12.137279474908));
#65325=CARTESIAN_POINT('Ctrl Pts',(29.7289079510236,-15.6869909143397,12.1514701037917));
#65326=CARTESIAN_POINT('Ctrl Pts',(29.7444572668981,-15.7020170541449,12.1664988607689));
#65327=CARTESIAN_POINT('Ctrl Pts',(29.7600106951577,-15.7170471679689,12.181531592457));
#65328=CARTESIAN_POINT('Ctrl Pts',(29.7739113767468,-15.7329229381326,12.1974036551064));
#65329=CARTESIAN_POINT('Ctrl Pts',(29.7860080855885,-15.7495003065487,12.2139724870494));
#65330=CARTESIAN_POINT('Ctrl Pts',(29.7916649639637,-15.7572525107338,12.221720699257));
#65331=CARTESIAN_POINT('Ctrl Pts',(29.7969266990436,-15.7651583176021,12.2296215756394));
#65332=CARTESIAN_POINT('Ctrl Pts',(29.8017740895379,-15.7732035030496,12.2376617309556));
#65333=CARTESIAN_POINT('Ctrl Pts',(29.8121759038527,-15.7904673329912,12.2549147669471));
#65334=CARTESIAN_POINT('Ctrl Pts',(29.8205897043228,-15.8082344071429,12.272670127495));
#65335=CARTESIAN_POINT('Ctrl Pts',(29.8268838981079,-15.8263459587282,12.2907815682763));
#65336=CARTESIAN_POINT('Ctrl Pts',(29.827291378433,-15.8275184839444,12.291954086319));
#65337=CARTESIAN_POINT('Ctrl Pts',(29.8276899587891,-15.8286924566664,12.2931281036774));
#65338=CARTESIAN_POINT('Ctrl Pts',(29.828079596474,-15.8298678351315,12.2943035833427));
#65339=CARTESIAN_POINT('Ctrl Pts',(29.8341018209648,-15.8480344377277,12.3124717500857));
#65340=CARTESIAN_POINT('Ctrl Pts',(29.8379920903099,-15.8665369818827,12.3309885243672));
#65341=CARTESIAN_POINT('Ctrl Pts',(29.8397834072957,-15.8852056234606,12.3496695928251));
#65342=CARTESIAN_POINT('Ctrl Pts',(29.8404573868545,-15.8922296638258,12.35669830878));
#65343=CARTESIAN_POINT('Ctrl Pts',(29.8408337073058,-15.8992771858287,12.3637503539203));
#65344=CARTESIAN_POINT('Ctrl Pts',(29.8409122430589,-15.9063388639742,12.3708160008987));
#65345=CARTESIAN_POINT('Ctrl Pts',(29.8411201875827,-15.9250365556902,12.389524201167));
#65346=CARTESIAN_POINT('Ctrl Pts',(29.8392425388012,-15.9436833457941,12.4081767974887));
#65347=CARTESIAN_POINT('Ctrl Pts',(29.8353415852832,-15.9621050095649,12.4265962128552));
#65348=CARTESIAN_POINT('Ctrl Pts',(29.8314529328994,-15.9804685830877,12.4449575450639));
#65349=CARTESIAN_POINT('Ctrl Pts',(29.8255535219271,-15.9986093925314,12.4630881464298));
#65350=CARTESIAN_POINT('Ctrl Pts',(29.8176551502795,-16.0163472264763,12.4808142028379));
#65351=CARTESIAN_POINT('Ctrl Pts',(29.814110942772,-16.0243066600203,12.4887683514908));
#65352=CARTESIAN_POINT('Ctrl Pts',(29.8101635813164,-16.0321847641427,12.4966409818454));
#65353=CARTESIAN_POINT('Ctrl Pts',(29.8058109922358,-16.0399639788694,12.5044157250402));
#65354=CARTESIAN_POINT('Ctrl Pts',(29.801757028854,-16.0472094713927,12.5116570528179));
#65355=CARTESIAN_POINT('Ctrl Pts',(29.7973617576402,-16.0543508658634,12.5187951035103));
#65356=CARTESIAN_POINT('Ctrl Pts',(29.7926271891742,-16.0613748908717,12.5258177264253));
#65357=CARTESIAN_POINT('Ctrl Pts',(29.7829544505351,-16.0757249966074,12.5401649676799));
#65358=CARTESIAN_POINT('Ctrl Pts',(29.7718670650277,-16.0895860216454,12.5540309525354));
#65359=CARTESIAN_POINT('Ctrl Pts',(29.7594824084483,-16.1028820335097,12.5673324817292));
#65360=CARTESIAN_POINT('Ctrl Pts',(29.7449214392259,-16.1185145073126,12.5829714424027));
#65361=CARTESIAN_POINT('Ctrl Pts',(29.728627582899,-16.133302772355,12.597766768395));
#65362=CARTESIAN_POINT('Ctrl Pts',(29.7107932614012,-16.1471218330033,12.6115882201676));
#65363=CARTESIAN_POINT('Ctrl Pts',(29.7060063962249,-16.1508309721592,12.6152980011191));
#65364=CARTESIAN_POINT('Ctrl Pts',(29.7011083138893,-16.1544701493571,12.6189375257229));
#65365=CARTESIAN_POINT('Ctrl Pts',(29.6961022501482,-16.1580366171813,12.6225040304587));
#65366=CARTESIAN_POINT('Ctrl Pts',(29.3372488480671,-15.556349186104,12.0208152801713));
#65367=CARTESIAN_POINT('Ctrl Pts',(29.5429564710669,-14.3836353036043,13.1935291626711));
#65368=CARTESIAN_POINT('Ctrl Pts',(29.5429564710669,-13.1935291626711,14.3836353036043));
#65369=CARTESIAN_POINT('Ctrl Pts',(29.3372488480671,-12.0208152801713,15.556349186104));
#65370=CARTESIAN_POINT('Origin',(8.,-12.0208152801713,15.556349186104));
#65371=CARTESIAN_POINT('',(8.,-15.556349186104,12.0208152801713));
#65372=CARTESIAN_POINT('Origin',(30.,18.5,0.));
#65373=CARTESIAN_POINT('',(30.,-15.0859875548336,11.5504536489008));
#65374=CARTESIAN_POINT('',(30.,-15.7939171599704,12.2583832540376));
#65375=CARTESIAN_POINT('',(30.,-4.03705806953519,0.501524163602477));
#65376=CARTESIAN_POINT('',(30.,-16.0983690173476,-11.8557283302283));
#65377=CARTESIAN_POINT('Origin',(30.,0.,0.));
#65378=CARTESIAN_POINT('',(30.,-15.3878195049812,-11.145178817862));
#65379=CARTESIAN_POINT('',(30.,-3.96634739141655,0.276293295702733));
#65380=CARTESIAN_POINT('Origin',(30.,0.,0.));
#65381=CARTESIAN_POINT('Origin',(29.5,0.,0.));
#65382=CARTESIAN_POINT('',(29.5,-14.7292483497821,11.1937144438494));
#65383=CARTESIAN_POINT('Ctrl Pts',(29.5,-14.7292483497821,11.1937144438494));
#65384=CARTESIAN_POINT('Ctrl Pts',(29.5615281526734,-14.7292483497821,11.1937144438494));
#65385=CARTESIAN_POINT('Ctrl Pts',(29.6339241856893,-14.7395012017362,11.2039672958034));
#65386=CARTESIAN_POINT('Ctrl Pts',(29.7477912665658,-14.7730323227637,11.237498416831));
#65387=CARTESIAN_POINT('Ctrl Pts',(29.8093392860887,-14.8023139816534,11.2667800757207));
#65388=CARTESIAN_POINT('Ctrl Pts',(29.8967622377582,-14.8644752333855,11.3289413274527));
#65389=CARTESIAN_POINT('Ctrl Pts',(29.9380095827943,-14.908422575575,11.3728886696422));
#65390=CARTESIAN_POINT('Ctrl Pts',(29.9854746058202,-14.9898767115274,11.4543428055946));
#65391=CARTESIAN_POINT('Ctrl Pts',(30.,-15.0418438629615,11.5063099570288));
#65392=CARTESIAN_POINT('Ctrl Pts',(30.,-15.0859875548336,11.5504536489008));
#65393=CARTESIAN_POINT('',(29.5,-14.9828768864291,-10.8518846384445));
#65394=CARTESIAN_POINT('Origin',(29.5,-15.3878195049812,-11.145178817862));
#65395=CARTESIAN_POINT('Origin',(29.5,0.,0.));
#65396=CARTESIAN_POINT('Origin',(29.5,-3.96634739141655,0.276293295702733));
#65397=CARTESIAN_POINT('',(29.9881723725086,-16.1105655835414,-12.0208152807707));
#65398=CARTESIAN_POINT('Ctrl Pts',(30.,-16.0983690173476,-11.8557283302283));
#65399=CARTESIAN_POINT('Ctrl Pts',(30.,-16.0984747560115,-11.8571296997209));
#65400=CARTESIAN_POINT('Ctrl Pts',(29.9999974820111,-16.0985804389106,-11.8585310768763));
#65401=CARTESIAN_POINT('Ctrl Pts',(29.9997996577384,-16.1027290491185,-11.9135718453621));
#65402=CARTESIAN_POINT('Ctrl Pts',(29.9959140013199,-16.1067121182789,-11.9675244439996));
#65403=CARTESIAN_POINT('Ctrl Pts',(29.9881723725061,-16.1105655840984,-12.02081528073));
#65404=CARTESIAN_POINT('',(29.5,-15.556349186104,-12.0208152801713));
#65405=CARTESIAN_POINT('Origin',(29.5,-16.2634559672906,-12.0208152801713));
#65406=CARTESIAN_POINT('',(29.5,-15.034266114388,-11.4987322084552));
#65407=CARTESIAN_POINT('',(29.5,-3.61279400082328,-0.0772600948905394));
#65408=CARTESIAN_POINT('Origin',(29.5,-15.3878195049812,-11.145178817862));
#65409=CARTESIAN_POINT('Origin',(29.5,-15.3878195049812,-11.145178817862));
#65410=CARTESIAN_POINT('Origin',(29.5,-15.3878195049812,-11.145178817862));
#65411=CARTESIAN_POINT('Origin',(25.5,0.,0.));
#65412=CARTESIAN_POINT('',(25.5,-14.9828768864291,-10.8518846384445));
#65413=CARTESIAN_POINT('',(25.5,-14.7292483497821,11.1937144438494));
#65414=CARTESIAN_POINT('Origin',(25.5,-15.3878195049812,-11.145178817862));
#65415=CARTESIAN_POINT('',(25.5,-15.034266114388,-11.4987322084552));
#65416=CARTESIAN_POINT('Origin',(8.,-14.7078210486802,-11.1722871427475));
#65417=CARTESIAN_POINT('',(8.,-15.556349186104,-12.0208152801713));
#65418=CARTESIAN_POINT('',(8.,-15.556349186104,-12.0208152801713));
#65419=CARTESIAN_POINT('',(8.,-15.0859875548336,-11.5504536489008));
#65420=CARTESIAN_POINT('',(8.,-14.7078210486802,-11.1722871427475));
#65421=CARTESIAN_POINT('',(7.99471483544825,-15.034266114388,-11.4987322084552));
#65422=CARTESIAN_POINT('Ctrl Pts',(7.9947148354483,-15.0342661143882,-11.4987322084555));
#65423=CARTESIAN_POINT('Ctrl Pts',(7.99834499875555,-15.05193500624,-11.5164011003073));
#65424=CARTESIAN_POINT('Ctrl Pts',(8.,-15.0695249347861,-11.5339910288533));
#65425=CARTESIAN_POINT('Ctrl Pts',(8.,-15.0859875548336,-11.5504536489008));
#65426=CARTESIAN_POINT('',(5.75,-15.034266114388,-11.4987322084552));
#65427=CARTESIAN_POINT('',(18.5,-14.7078210486802,-11.1722871427475));
#65428=CARTESIAN_POINT('Origin',(18.5,-14.3542676580869,-10.8187337521542));
#65429=CARTESIAN_POINT('',(20.5,-14.7078210486802,-11.1722871427475));
#65430=CARTESIAN_POINT('',(8.,-14.7078210486802,-11.1722871427475));
#65431=CARTESIAN_POINT('Origin',(20.5,-14.3542676580869,-10.8187337521542));
#65432=CARTESIAN_POINT('Origin',(29.5,0.,0.));
#65433=CARTESIAN_POINT('',(29.9932812305893,-12.316603510208,-15.8521374161407));
#65434=CARTESIAN_POINT('Ctrl Pts',(29.9932812305893,-12.316603510208,-15.8521374161407));
#65435=CARTESIAN_POINT('Ctrl Pts',(29.9919012225592,-12.2164522272255,-15.9405042246621));
#65436=CARTESIAN_POINT('Ctrl Pts',(29.9902210922164,-12.1178209250676,-16.0266428857885));
#65437=CARTESIAN_POINT('Ctrl Pts',(29.9881723734926,-12.0208153230367,-16.1105655469738));
#65438=CARTESIAN_POINT('',(29.9932812305893,-15.8521374161407,-12.3166035102079));
#65439=CARTESIAN_POINT('Ctrl Pts',(29.9932812305893,-12.316603510208,-15.8521374161407));
#65440=CARTESIAN_POINT('Ctrl Pts',(30.0014921231503,-12.912492379305,-15.3263648446124));
#65441=CARTESIAN_POINT('Ctrl Pts',(29.9999747373918,-13.5018717719603,-14.7749150943608));
#65442=CARTESIAN_POINT('Ctrl Pts',(29.9999996618613,-14.7028008951429,-13.5788340778648));
#65443=CARTESIAN_POINT('Ctrl Pts',(30.0020243268535,-15.2922859539755,-12.9511159833143));
#65444=CARTESIAN_POINT('Ctrl Pts',(29.9932812305893,-15.8521374161407,-12.3166035102079));
#65445=CARTESIAN_POINT('Ctrl Pts',(29.9881723725999,-16.1105655835412,-12.0208152807686));
#65446=CARTESIAN_POINT('Ctrl Pts',(29.9902249428434,-16.0264851557198,-12.1180032443948));
#65447=CARTESIAN_POINT('Ctrl Pts',(29.9919036240457,-15.940350448964,-12.2166265102365));
#65448=CARTESIAN_POINT('Ctrl Pts',(29.9932812305893,-15.8521374161407,-12.3166035102079));
#65449=CARTESIAN_POINT('Ctrl Pts',(29.8535533905933,-16.0458601314941,12.5103262255613));
#65450=CARTESIAN_POINT('Ctrl Pts',(29.8971736290481,-16.0147804613409,12.4792465554081));
#65451=CARTESIAN_POINT('Ctrl Pts',(29.9381460122713,-15.9710776301552,12.4355437242224));
#65452=CARTESIAN_POINT('Ctrl Pts',(29.985486770529,-15.8898992445794,12.3543653386467));
#65453=CARTESIAN_POINT('Ctrl Pts',(30.,-15.8380021716785,12.3024682657458));
#65454=CARTESIAN_POINT('Ctrl Pts',(30.,-15.7939171599704,12.2583832540376));
#65455=CARTESIAN_POINT('Origin',(29.5,-10.4010191002141,-17.8832521472478));
#65456=CARTESIAN_POINT('',(29.5,-10.0474657096209,-17.5296987566545));
#65457=CARTESIAN_POINT('Origin',(8.,-12.0208152801713,-15.556349186104));
#65458=CARTESIAN_POINT('',(20.5,-11.1722871427475,-14.7078210486802));
#65459=CARTESIAN_POINT('Origin',(20.5,-10.8187337521542,-14.3542676580869));
#65460=CARTESIAN_POINT('',(18.5,-11.1722871427475,-14.7078210486802));
#65461=CARTESIAN_POINT('',(8.,-11.1722871427475,-14.7078210486802));
#65462=CARTESIAN_POINT('Origin',(18.5,-10.8187337521542,-14.3542676580869));
#65463=CARTESIAN_POINT('',(7.99471483544825,-11.4987322084552,-15.034266114388));
#65464=CARTESIAN_POINT('',(5.75,-11.4987322084552,-15.034266114388));
#65465=CARTESIAN_POINT('',(8.,-11.5504536489008,-15.0859875548336));
#65466=CARTESIAN_POINT('Ctrl Pts',(8.,-11.5504536489008,-15.0859875548336));
#65467=CARTESIAN_POINT('Ctrl Pts',(8.,-11.5339910288533,-15.0695249347861));
#65468=CARTESIAN_POINT('Ctrl Pts',(7.99834499875555,-11.5164011003073,-15.05193500624));
#65469=CARTESIAN_POINT('Ctrl Pts',(7.9947148354483,-11.4987322084555,-15.0342661143882));
#65470=CARTESIAN_POINT('',(8.,-12.0208152801713,-15.556349186104));
#65471=CARTESIAN_POINT('',(8.,-12.0208152801713,-15.556349186104));
#65472=CARTESIAN_POINT('',(8.,-12.0208152801713,-15.556349186104));
#65473=CARTESIAN_POINT('Origin',(8.,-15.556349186104,-12.0208152801713));
#65474=CARTESIAN_POINT('',(8.,-15.556349186104,-12.0208152801713));
#65475=CARTESIAN_POINT('Origin',(18.5,-7.07761722863737,-18.0953841816037));
#65476=CARTESIAN_POINT('',(18.5,-7.43117061923064,-18.448937572197));
#65477=CARTESIAN_POINT('Origin',(8.,-11.1722871427475,-14.7078210486802));
#65478=CARTESIAN_POINT('',(20.5,-9.80617061923064,-16.073937572197));
#65479=CARTESIAN_POINT('Origin',(20.5,-9.45261722863737,-15.7203841816037));
#65480=CARTESIAN_POINT('Origin',(5.75,-15.3878195049812,-11.145178817862));
#65481=CARTESIAN_POINT('Ctrl Pts',(7.99471483544825,-15.034266114388,-11.4987322084552));
#65482=CARTESIAN_POINT('Ctrl Pts',(7.98769634133013,-15.0001053885364,-11.4645714826037));
#65483=CARTESIAN_POINT('Ctrl Pts',(7.97399551550773,-14.9722150037425,-11.4267999995771));
#65484=CARTESIAN_POINT('Ctrl Pts',(7.93177050929415,-14.9230460849828,-11.3379640139829));
#65485=CARTESIAN_POINT('Ctrl Pts',(7.90093775901624,-14.9057072463616,-11.2870133597151));
#65486=CARTESIAN_POINT('Ctrl Pts',(7.8176582095554,-14.8833482376701,-11.1678537278356));
#65487=CARTESIAN_POINT('Ctrl Pts',(7.76105956129052,-14.8858405817402,-11.1002085369641));
#65488=CARTESIAN_POINT('Ctrl Pts',(7.6384159401128,-14.9141444743334,-10.9707529826629));
#65489=CARTESIAN_POINT('Ctrl Pts',(7.57043047269953,-14.9424536474475,-10.9084183644052));
#65490=CARTESIAN_POINT('Ctrl Pts',(7.5021074297362,-14.9816596935131,-10.8535707098408));
#65491=CARTESIAN_POINT('Ctrl Pts',(7.50105371344569,-14.9822669774523,-10.8527267217707));
#65492=CARTESIAN_POINT('Ctrl Pts',(7.5,-14.9828768864291,-10.8518846384445));
#65493=CARTESIAN_POINT('Origin',(5.75,-11.145178817862,-15.3878195049812));
#65494=CARTESIAN_POINT('Ctrl Pts',(7.5,-10.8518846384445,-14.9828768864291));
#65495=CARTESIAN_POINT('Ctrl Pts',(7.50105371344605,-10.852726721771,-14.9822669774521));
#65496=CARTESIAN_POINT('Ctrl Pts',(7.5021074297361,-10.8535707098409,-14.981659693513));
#65497=CARTESIAN_POINT('Ctrl Pts',(7.59351569467807,-10.9269504763458,-14.9292065753494));
#65498=CARTESIAN_POINT('Ctrl Pts',(7.68214848767641,-11.0120989243862,-14.8976245327993));
#65499=CARTESIAN_POINT('Ctrl Pts',(7.81958013152834,-11.1704454530309,-14.8836434033438));
#65500=CARTESIAN_POINT('Ctrl Pts',(7.87098023972501,-11.2398826207744,-14.8919941158642));
#65501=CARTESIAN_POINT('Ctrl Pts',(7.94048867507028,-11.3545161973503,-14.930821569437));
#65502=CARTESIAN_POINT('Ctrl Pts',(7.96491477585457,-11.4033401554801,-14.9558097197836));
#65503=CARTESIAN_POINT('Ctrl Pts',(7.98678347589508,-11.4662908869419,-15.0039319604953));
#65504=CARTESIAN_POINT('Ctrl Pts',(7.99147733125719,-11.4829744844687,-15.0185083904015));
#65505=CARTESIAN_POINT('Ctrl Pts',(7.99471483544825,-11.4987322084552,-15.034266114388));
#65506=CARTESIAN_POINT('Origin',(7.5,0.,0.));
#65507=CARTESIAN_POINT('Origin',(8.,0.,0.));
#65508=CARTESIAN_POINT('Origin',(8.,-13.3643181644258,-13.3643181644257));
#65509=CARTESIAN_POINT('Origin',(8.,-15.556349186104,12.0208152801713));
#65510=CARTESIAN_POINT('Origin',(8.,15.556349186104,-12.0208152801713));
#65511=CARTESIAN_POINT('',(25.5,14.7292483497821,-11.1937144438494));
#65512=CARTESIAN_POINT('Origin',(25.5,0.,0.));
#65513=CARTESIAN_POINT('Origin',(25.5,0.,0.));
#65514=CARTESIAN_POINT('Origin',(-6.5,21.5,3.5));
#65515=CARTESIAN_POINT('Origin',(-6.25,0.,0.));
#65516=CARTESIAN_POINT('Origin',(-6.25,0.,0.));
#65517=CARTESIAN_POINT('',(0.,0.,0.));
#65518=CARTESIAN_POINT('',(0.,0.,0.));
#65519=CARTESIAN_POINT('',(25.,-5.55111512312578E-16,0.));
#65520=CARTESIAN_POINT('',(-12.5,21.650635094611,0.));
#65521=CARTESIAN_POINT('',(-12.5,-21.650635094611,0.));
#65522=CARTESIAN_POINT('',(25.,0.,0.));
#65523=CARTESIAN_POINT('',(-12.5,21.650635094611,0.));
#65524=CARTESIAN_POINT('',(-12.5,-21.650635094611,0.));
#65525=CARTESIAN_POINT('',(27.2236110756821,27.2236110756821,-82.5));
#65526=CARTESIAN_POINT('',(-27.2236110756821,27.2236110756821,-82.5));
#65527=CARTESIAN_POINT('',(-27.2236110756821,-27.2236110756821,-82.5));
#65528=CARTESIAN_POINT('',(27.2236110756821,-27.2236110756821,-82.5));
#65529=CARTESIAN_POINT('',(27.2236110756821,27.2236110756821,-82.5));
#65530=CARTESIAN_POINT('',(-27.2236110756821,27.2236110756821,-82.5));
#65531=CARTESIAN_POINT('',(-27.2236110756821,-27.2236110756821,-82.5));
#65532=CARTESIAN_POINT('',(27.2236110756821,-27.2236110756821,-82.5));
#65533=CARTESIAN_POINT('',(0.,0.,0.));
#65534=CARTESIAN_POINT('',(0.,0.,0.));
#65535=CARTESIAN_POINT('',(0.,0.,0.));
#65536=CARTESIAN_POINT('',(0.,0.,0.));
#65537=CARTESIAN_POINT('',(0.,0.,0.));
#65538=UNCERTAINTY_MEASURE_WITH_UNIT(LENGTH_MEASURE(0.01),#65564,
'DISTANCE_ACCURACY_VALUE',
'Maximum model space distance between geometric entities at asserted c
onnectivities');
#65539=UNCERTAINTY_MEASURE_WITH_UNIT(LENGTH_MEASURE(0.01),#65564,
'DISTANCE_ACCURACY_VALUE',
'Maximum model space distance between geometric entities at asserted c
onnectivities');
#65540=UNCERTAINTY_MEASURE_WITH_UNIT(LENGTH_MEASURE(0.01),#65564,
'DISTANCE_ACCURACY_VALUE',
'Maximum model space distance between geometric entities at asserted c
onnectivities');
#65541=UNCERTAINTY_MEASURE_WITH_UNIT(LENGTH_MEASURE(0.01),#65564,
'DISTANCE_ACCURACY_VALUE',
'Maximum model space distance between geometric entities at asserted c
onnectivities');
#65542=UNCERTAINTY_MEASURE_WITH_UNIT(LENGTH_MEASURE(0.01),#65564,
'DISTANCE_ACCURACY_VALUE',
'Maximum model space distance between geometric entities at asserted c
onnectivities');
#65543=UNCERTAINTY_MEASURE_WITH_UNIT(LENGTH_MEASURE(0.01),#65564,
'DISTANCE_ACCURACY_VALUE',
'Maximum model space distance between geometric entities at asserted c
onnectivities');
#65544=UNCERTAINTY_MEASURE_WITH_UNIT(LENGTH_MEASURE(0.01),#65564,
'DISTANCE_ACCURACY_VALUE',
'Maximum model space distance between geometric entities at asserted c
onnectivities');
#65545=UNCERTAINTY_MEASURE_WITH_UNIT(LENGTH_MEASURE(0.01),#65564,
'DISTANCE_ACCURACY_VALUE',
'Maximum model space distance between geometric entities at asserted c
onnectivities');
#65546=UNCERTAINTY_MEASURE_WITH_UNIT(LENGTH_MEASURE(0.01),#65564,
'DISTANCE_ACCURACY_VALUE',
'Maximum model space distance between geometric entities at asserted c
onnectivities');
#65547=UNCERTAINTY_MEASURE_WITH_UNIT(LENGTH_MEASURE(0.01),#65564,
'DISTANCE_ACCURACY_VALUE',
'Maximum model space distance between geometric entities at asserted c
onnectivities');
#65548=UNCERTAINTY_MEASURE_WITH_UNIT(LENGTH_MEASURE(0.01),#65564,
'DISTANCE_ACCURACY_VALUE',
'Maximum model space distance between geometric entities at asserted c
onnectivities');
#65549=UNCERTAINTY_MEASURE_WITH_UNIT(LENGTH_MEASURE(0.01),#65564,
'DISTANCE_ACCURACY_VALUE',
'Maximum model space distance between geometric entities at asserted c
onnectivities');
#65550=UNCERTAINTY_MEASURE_WITH_UNIT(LENGTH_MEASURE(0.01),#65564,
'DISTANCE_ACCURACY_VALUE',
'Maximum model space distance between geometric entities at asserted c
onnectivities');
#65551=(
GEOMETRIC_REPRESENTATION_CONTEXT(3)
GLOBAL_UNCERTAINTY_ASSIGNED_CONTEXT((#65538))
GLOBAL_UNIT_ASSIGNED_CONTEXT((#65564,#65566,#65567))
REPRESENTATION_CONTEXT('','3D')
);
#65552=(
GEOMETRIC_REPRESENTATION_CONTEXT(3)
GLOBAL_UNCERTAINTY_ASSIGNED_CONTEXT((#65539))
GLOBAL_UNIT_ASSIGNED_CONTEXT((#65564,#65566,#65567))
REPRESENTATION_CONTEXT('','3D')
);
#65553=(
GEOMETRIC_REPRESENTATION_CONTEXT(3)
GLOBAL_UNCERTAINTY_ASSIGNED_CONTEXT((#65540))
GLOBAL_UNIT_ASSIGNED_CONTEXT((#65564,#65566,#65567))
REPRESENTATION_CONTEXT('','3D')
);
#65554=(
GEOMETRIC_REPRESENTATION_CONTEXT(3)
GLOBAL_UNCERTAINTY_ASSIGNED_CONTEXT((#65541))
GLOBAL_UNIT_ASSIGNED_CONTEXT((#65564,#65566,#65567))
REPRESENTATION_CONTEXT('','3D')
);
#65555=(
GEOMETRIC_REPRESENTATION_CONTEXT(3)
GLOBAL_UNCERTAINTY_ASSIGNED_CONTEXT((#65542))
GLOBAL_UNIT_ASSIGNED_CONTEXT((#65564,#65566,#65567))
REPRESENTATION_CONTEXT('','3D')
);
#65556=(
GEOMETRIC_REPRESENTATION_CONTEXT(3)
GLOBAL_UNCERTAINTY_ASSIGNED_CONTEXT((#65543))
GLOBAL_UNIT_ASSIGNED_CONTEXT((#65564,#65566,#65567))
REPRESENTATION_CONTEXT('','3D')
);
#65557=(
GEOMETRIC_REPRESENTATION_CONTEXT(3)
GLOBAL_UNCERTAINTY_ASSIGNED_CONTEXT((#65544))
GLOBAL_UNIT_ASSIGNED_CONTEXT((#65564,#65566,#65567))
REPRESENTATION_CONTEXT('','3D')
);
#65558=(
GEOMETRIC_REPRESENTATION_CONTEXT(3)
GLOBAL_UNCERTAINTY_ASSIGNED_CONTEXT((#65545))
GLOBAL_UNIT_ASSIGNED_CONTEXT((#65564,#65566,#65567))
REPRESENTATION_CONTEXT('','3D')
);
#65559=(
GEOMETRIC_REPRESENTATION_CONTEXT(3)
GLOBAL_UNCERTAINTY_ASSIGNED_CONTEXT((#65546))
GLOBAL_UNIT_ASSIGNED_CONTEXT((#65564,#65566,#65567))
REPRESENTATION_CONTEXT('','3D')
);
#65560=(
GEOMETRIC_REPRESENTATION_CONTEXT(3)
GLOBAL_UNCERTAINTY_ASSIGNED_CONTEXT((#65547))
GLOBAL_UNIT_ASSIGNED_CONTEXT((#65564,#65566,#65567))
REPRESENTATION_CONTEXT('','3D')
);
#65561=(
GEOMETRIC_REPRESENTATION_CONTEXT(3)
GLOBAL_UNCERTAINTY_ASSIGNED_CONTEXT((#65548))
GLOBAL_UNIT_ASSIGNED_CONTEXT((#65564,#65566,#65567))
REPRESENTATION_CONTEXT('','3D')
);
#65562=(
GEOMETRIC_REPRESENTATION_CONTEXT(3)
GLOBAL_UNCERTAINTY_ASSIGNED_CONTEXT((#65549))
GLOBAL_UNIT_ASSIGNED_CONTEXT((#65564,#65566,#65567))
REPRESENTATION_CONTEXT('','3D')
);
#65563=(
GEOMETRIC_REPRESENTATION_CONTEXT(3)
GLOBAL_UNCERTAINTY_ASSIGNED_CONTEXT((#65550))
GLOBAL_UNIT_ASSIGNED_CONTEXT((#65564,#65566,#65567))
REPRESENTATION_CONTEXT('','3D')
);
#65564=(
LENGTH_UNIT()
NAMED_UNIT(*)
SI_UNIT(.MILLI.,.METRE.)
);
#65565=(
LENGTH_UNIT()
NAMED_UNIT(*)
SI_UNIT($,.METRE.)
);
#65566=(
NAMED_UNIT(*)
PLANE_ANGLE_UNIT()
SI_UNIT($,.RADIAN.)
);
#65567=(
NAMED_UNIT(*)
SI_UNIT($,.STERADIAN.)
SOLID_ANGLE_UNIT()
);
#65568=SHAPE_DEFINITION_REPRESENTATION(#65580,#65613);
#65569=SHAPE_DEFINITION_REPRESENTATION(#65581,#65614);
#65570=SHAPE_DEFINITION_REPRESENTATION(#65582,#65615);
#65571=SHAPE_DEFINITION_REPRESENTATION(#65583,#65616);
#65572=SHAPE_DEFINITION_REPRESENTATION(#65584,#65617);
#65573=SHAPE_DEFINITION_REPRESENTATION(#65585,#65618);
#65574=SHAPE_DEFINITION_REPRESENTATION(#65586,#65619);
#65575=SHAPE_DEFINITION_REPRESENTATION(#65587,#65620);
#65576=SHAPE_DEFINITION_REPRESENTATION(#65588,#65621);
#65577=SHAPE_DEFINITION_REPRESENTATION(#65589,#65622);
#65578=SHAPE_DEFINITION_REPRESENTATION(#65590,#65623);
#65579=SHAPE_DEFINITION_REPRESENTATION(#65591,#65624);
#65580=PRODUCT_DEFINITION_SHAPE('',$,#65626);
#65581=PRODUCT_DEFINITION_SHAPE('',$,#65627);
#65582=PRODUCT_DEFINITION_SHAPE('',$,#65628);
#65583=PRODUCT_DEFINITION_SHAPE('',$,#65629);
#65584=PRODUCT_DEFINITION_SHAPE('',$,#65630);
#65585=PRODUCT_DEFINITION_SHAPE('',$,#65631);
#65586=PRODUCT_DEFINITION_SHAPE('',$,#65632);
#65587=PRODUCT_DEFINITION_SHAPE('',$,#65633);
#65588=PRODUCT_DEFINITION_SHAPE('',$,#65634);
#65589=PRODUCT_DEFINITION_SHAPE('',$,#65635);
#65590=PRODUCT_DEFINITION_SHAPE('',$,#65636);
#65591=PRODUCT_DEFINITION_SHAPE('',$,#65637);
#65592=PRODUCT_DEFINITION_SHAPE($,$,#74);
#65593=PRODUCT_DEFINITION_SHAPE($,$,#75);
#65594=PRODUCT_DEFINITION_SHAPE($,$,#76);
#65595=PRODUCT_DEFINITION_SHAPE($,$,#77);
#65596=PRODUCT_DEFINITION_SHAPE($,$,#78);
#65597=PRODUCT_DEFINITION_SHAPE($,$,#79);
#65598=PRODUCT_DEFINITION_SHAPE($,$,#80);
#65599=PRODUCT_DEFINITION_SHAPE($,$,#81);
#65600=PRODUCT_DEFINITION_SHAPE($,$,#82);
#65601=PRODUCT_DEFINITION_SHAPE($,$,#83);
#65602=PRODUCT_DEFINITION_SHAPE($,$,#84);
#65603=PRODUCT_DEFINITION_SHAPE($,$,#85);
#65604=PRODUCT_DEFINITION_SHAPE($,$,#86);
#65605=PRODUCT_DEFINITION_SHAPE($,$,#87);
#65606=PRODUCT_DEFINITION_SHAPE($,$,#88);
#65607=PRODUCT_DEFINITION_SHAPE($,$,#89);
#65608=PRODUCT_DEFINITION_SHAPE($,$,#90);
#65609=PRODUCT_DEFINITION_SHAPE($,$,#91);
#65610=PRODUCT_DEFINITION_SHAPE($,$,#92);
#65611=PRODUCT_DEFINITION_SHAPE($,$,#93);
#65612=PRODUCT_DEFINITION_SHAPE($,$,#94);
#65613=SHAPE_REPRESENTATION('',(#20141,#22382,#22383,#22384,#22385,#22386,
#22387,#22388,#22389,#22390,#22391,#22392,#22393,#22394,#22395,#22396,#22397,
#22398,#22399,#22400,#22401,#22402),#65551);
#65614=SHAPE_REPRESENTATION('',(#20142),#65552);
#65615=SHAPE_REPRESENTATION('',(#20555),#65553);
#65616=SHAPE_REPRESENTATION('',(#21298),#65554);
#65617=SHAPE_REPRESENTATION('',(#21673),#65555);
#65618=SHAPE_REPRESENTATION('',(#21701),#65556);
#65619=SHAPE_REPRESENTATION('',(#21742),#65557);
#65620=SHAPE_REPRESENTATION('',(#21770),#65558);
#65621=SHAPE_REPRESENTATION('',(#21777),#65559);
#65622=SHAPE_REPRESENTATION('',(#22009),#65560);
#65623=SHAPE_REPRESENTATION('',(#22036),#65561);
#65624=SHAPE_REPRESENTATION('',(#22041),#65562);
#65625=PRODUCT_DEFINITION_CONTEXT('part definition',#65663,'design');
#65626=PRODUCT_DEFINITION('2026-10-10-05-45-21-003','MAS-366',#65638,#65625);
#65627=PRODUCT_DEFINITION('2026-10-10-05-45-21-337',
'01_Axle_with_Machined_Sun_Pinion_Z15_M1.25',#65639,#65625);
#65628=PRODUCT_DEFINITION('2026-10-10-05-45-22-506',
'02_Planet_Cage_Bottom_Disc_and_Notched_Top_Plate',#65640,#65625);
#65629=PRODUCT_DEFINITION('2026-10-10-05-45-24-894',
'03_Compound_Planet_Pinion_Z25-Z14_M1.25',#65641,#65625);
#65630=PRODUCT_DEFINITION('2026-10-10-05-45-27-457',
'04_Planet_Pin_D6x65',#65642,#65625);
#65631=PRODUCT_DEFINITION('2026-10-10-05-45-27-787',
'05_Cage_Ratchet_Pawl',#65643,#65625);
#65632=PRODUCT_DEFINITION('2026-10-10-05-45-28-330',
'06_ISO_8734_Pawl_Pin_D2.5x10',#65644,#65625);
#65633=PRODUCT_DEFINITION('2026-10-10-05-45-28-717',
'07_Pawl_Spring_Ring_Wire_D1.2',#65645,#65625);
#65634=PRODUCT_DEFINITION('2026-10-10-05-45-28-951',
'08_Sliding_Clutch_Collar',#65646,#65625);
#65635=PRODUCT_DEFINITION('2026-10-10-05-45-29-923',
'09_Axle_Key_4x4x19.8',#65647,#65625);
#65636=PRODUCT_DEFINITION('2026-10-10-05-45-30-305',
'10_Clutch_Compression_Spring_d1.6',#65648,#65625);
#65637=PRODUCT_DEFINITION('2026-10-10-05-45-31-198',
'11_Brass_Driver_Sleeve',#65649,#65625);
#65638=PRODUCT_DEFINITION_FORMATION('',$,#65665);
#65639=PRODUCT_DEFINITION_FORMATION('',$,#65666);
#65640=PRODUCT_DEFINITION_FORMATION('',$,#65667);
#65641=PRODUCT_DEFINITION_FORMATION('',$,#65668);
#65642=PRODUCT_DEFINITION_FORMATION('',$,#65669);
#65643=PRODUCT_DEFINITION_FORMATION('',$,#65670);
#65644=PRODUCT_DEFINITION_FORMATION('',$,#65671);
#65645=PRODUCT_DEFINITION_FORMATION('',$,#65672);
#65646=PRODUCT_DEFINITION_FORMATION('',$,#65673);
#65647=PRODUCT_DEFINITION_FORMATION('',$,#65674);
#65648=PRODUCT_DEFINITION_FORMATION('',$,#65675);
#65649=PRODUCT_DEFINITION_FORMATION('',$,#65676);
#65650=PRODUCT_RELATED_PRODUCT_CATEGORY('MAS-366','MAS-366',(#65665));
#65651=PRODUCT_RELATED_PRODUCT_CATEGORY(
'01_Axle_with_Machined_Sun_Pinion_Z15_M1.25',
'01_Axle_with_Machined_Sun_Pinion_Z15_M1.25',(#65666));
#65652=PRODUCT_RELATED_PRODUCT_CATEGORY(
'02_Planet_Cage_Bottom_Disc_and_Notched_Top_Plate',
'02_Planet_Cage_Bottom_Disc_and_Notched_Top_Plate',(#65667));
#65653=PRODUCT_RELATED_PRODUCT_CATEGORY(
'03_Compound_Planet_Pinion_Z25-Z14_M1.25',
'03_Compound_Planet_Pinion_Z25-Z14_M1.25',(#65668));
#65654=PRODUCT_RELATED_PRODUCT_CATEGORY('04_Planet_Pin_D6x65',
'04_Planet_Pin_D6x65',(#65669));
#65655=PRODUCT_RELATED_PRODUCT_CATEGORY('05_Cage_Ratchet_Pawl',
'05_Cage_Ratchet_Pawl',(#65670));
#65656=PRODUCT_RELATED_PRODUCT_CATEGORY('06_ISO_8734_Pawl_Pin_D2.5x10',
'06_ISO_8734_Pawl_Pin_D2.5x10',(#65671));
#65657=PRODUCT_RELATED_PRODUCT_CATEGORY('07_Pawl_Spring_Ring_Wire_D1.2',
'07_Pawl_Spring_Ring_Wire_D1.2',(#65672));
#65658=PRODUCT_RELATED_PRODUCT_CATEGORY('08_Sliding_Clutch_Collar',
'08_Sliding_Clutch_Collar',(#65673));
#65659=PRODUCT_RELATED_PRODUCT_CATEGORY('09_Axle_Key_4x4x19.8',
'09_Axle_Key_4x4x19.8',(#65674));
#65660=PRODUCT_RELATED_PRODUCT_CATEGORY(
'10_Clutch_Compression_Spring_d1.6','10_Clutch_Compression_Spring_d1.6',
(#65675));
#65661=PRODUCT_RELATED_PRODUCT_CATEGORY('11_Brass_Driver_Sleeve',
'11_Brass_Driver_Sleeve',(#65676));
#65662=APPLICATION_PROTOCOL_DEFINITION('international standard',
'automotive_design',2009,#65663);
#65663=APPLICATION_CONTEXT(
'Core Data for Automotive Mechanical Design Process');
#65664=PRODUCT_CONTEXT('part definition',#65663,'mechanical');
#65665=PRODUCT('2026-10-10-05-45-21-003','MAS-366',$,(#65664));
#65666=PRODUCT('2026-10-10-05-45-21-337',
'01_Axle_with_Machined_Sun_Pinion_Z15_M1.25',$,(#65664));
#65667=PRODUCT('2026-10-10-05-45-22-506',
'02_Planet_Cage_Bottom_Disc_and_Notched_Top_Plate',$,(#65664));
#65668=PRODUCT('2026-10-10-05-45-24-894',
'03_Compound_Planet_Pinion_Z25-Z14_M1.25',$,(#65664));
#65669=PRODUCT('2026-10-10-05-45-27-457','04_Planet_Pin_D6x65',$,(#65664));
#65670=PRODUCT('2026-10-10-05-45-27-787','05_Cage_Ratchet_Pawl',$,(#65664));
#65671=PRODUCT('2026-10-10-05-45-28-330','06_ISO_8734_Pawl_Pin_D2.5x10',
$,(#65664));
#65672=PRODUCT('2026-10-10-05-45-28-717',
'07_Pawl_Spring_Ring_Wire_D1.2',$,(#65664));
#65673=PRODUCT('2026-10-10-05-45-28-951','08_Sliding_Clutch_Collar',$,(#65664));
#65674=PRODUCT('2026-10-10-05-45-29-923','09_Axle_Key_4x4x19.8',$,(#65664));
#65675=PRODUCT('2026-10-10-05-45-30-305',
'10_Clutch_Compression_Spring_d1.6',$,(#65664));
#65676=PRODUCT('2026-10-10-05-45-31-198','11_Brass_Driver_Sleeve',$,(#65664));
#65677=PRESENTATION_STYLE_ASSIGNMENT((#65689));
#65678=PRESENTATION_STYLE_ASSIGNMENT((#65690));
#65679=PRESENTATION_STYLE_ASSIGNMENT((#65691));
#65680=PRESENTATION_STYLE_ASSIGNMENT((#65692));
#65681=PRESENTATION_STYLE_ASSIGNMENT((#65693));
#65682=PRESENTATION_STYLE_ASSIGNMENT((#65694));
#65683=PRESENTATION_STYLE_ASSIGNMENT((#65695));
#65684=PRESENTATION_STYLE_ASSIGNMENT((#65696));
#65685=PRESENTATION_STYLE_ASSIGNMENT((#65697));
#65686=PRESENTATION_STYLE_ASSIGNMENT((#65698));
#65687=PRESENTATION_STYLE_ASSIGNMENT((#65699));
#65688=PRESENTATION_STYLE_ASSIGNMENT((#65700));
#65689=SURFACE_STYLE_USAGE(.BOTH.,#65701);
#65690=SURFACE_STYLE_USAGE(.BOTH.,#65702);
#65691=SURFACE_STYLE_USAGE(.BOTH.,#65703);
#65692=SURFACE_STYLE_USAGE(.BOTH.,#65704);
#65693=SURFACE_STYLE_USAGE(.BOTH.,#65705);
#65694=SURFACE_STYLE_USAGE(.BOTH.,#65706);
#65695=SURFACE_STYLE_USAGE(.BOTH.,#65707);
#65696=SURFACE_STYLE_USAGE(.BOTH.,#65708);
#65697=SURFACE_STYLE_USAGE(.BOTH.,#65709);
#65698=SURFACE_STYLE_USAGE(.BOTH.,#65710);
#65699=SURFACE_STYLE_USAGE(.BOTH.,#65711);
#65700=SURFACE_STYLE_USAGE(.BOTH.,#65712);
#65701=SURFACE_SIDE_STYLE('',(#65713));
#65702=SURFACE_SIDE_STYLE('',(#65714));
#65703=SURFACE_SIDE_STYLE('',(#65715));
#65704=SURFACE_SIDE_STYLE('',(#65716));
#65705=SURFACE_SIDE_STYLE('',(#65717));
#65706=SURFACE_SIDE_STYLE('',(#65718));
#65707=SURFACE_SIDE_STYLE('',(#65719));
#65708=SURFACE_SIDE_STYLE('',(#65720));
#65709=SURFACE_SIDE_STYLE('',(#65721));
#65710=SURFACE_SIDE_STYLE('',(#65722));
#65711=SURFACE_SIDE_STYLE('',(#65723));
#65712=SURFACE_SIDE_STYLE('',(#65724));
#65713=SURFACE_STYLE_FILL_AREA(#65725);
#65714=SURFACE_STYLE_FILL_AREA(#65726);
#65715=SURFACE_STYLE_FILL_AREA(#65727);
#65716=SURFACE_STYLE_FILL_AREA(#65728);
#65717=SURFACE_STYLE_FILL_AREA(#65729);
#65718=SURFACE_STYLE_FILL_AREA(#65730);
#65719=SURFACE_STYLE_FILL_AREA(#65731);
#65720=SURFACE_STYLE_FILL_AREA(#65732);
#65721=SURFACE_STYLE_FILL_AREA(#65733);
#65722=SURFACE_STYLE_FILL_AREA(#65734);
#65723=SURFACE_STYLE_FILL_AREA(#65735);
#65724=SURFACE_STYLE_FILL_AREA(#65736);
#65725=FILL_AREA_STYLE('Steel - Satin',(#65737));
#65726=FILL_AREA_STYLE('MAS366_axle',(#65738));
#65727=FILL_AREA_STYLE('MAS366_cage',(#65739));
#65728=FILL_AREA_STYLE('MAS366_planet',(#65740));
#65729=FILL_AREA_STYLE('MAS366_pin',(#65741));
#65730=FILL_AREA_STYLE('MAS366_pawl',(#65742));
#65731=FILL_AREA_STYLE('MAS366_pawlpin',(#65743));
#65732=FILL_AREA_STYLE('MAS366_ringspring',(#65744));
#65733=FILL_AREA_STYLE('MAS366_clutch',(#65745));
#65734=FILL_AREA_STYLE('MAS366_key',(#65746));
#65735=FILL_AREA_STYLE('MAS366_spring',(#65747));
#65736=FILL_AREA_STYLE('MAS366_driver',(#65748));
#65737=FILL_AREA_STYLE_COLOUR('Steel - Satin',#65749);
#65738=FILL_AREA_STYLE_COLOUR('MAS366_axle',#65750);
#65739=FILL_AREA_STYLE_COLOUR('MAS366_cage',#65751);
#65740=FILL_AREA_STYLE_COLOUR('MAS366_planet',#65752);
#65741=FILL_AREA_STYLE_COLOUR('MAS366_pin',#65753);
#65742=FILL_AREA_STYLE_COLOUR('MAS366_pawl',#65754);
#65743=FILL_AREA_STYLE_COLOUR('MAS366_pawlpin',#65755);
#65744=FILL_AREA_STYLE_COLOUR('MAS366_ringspring',#65756);
#65745=FILL_AREA_STYLE_COLOUR('MAS366_clutch',#65757);
#65746=FILL_AREA_STYLE_COLOUR('MAS366_key',#65758);
#65747=FILL_AREA_STYLE_COLOUR('MAS366_spring',#65759);
#65748=FILL_AREA_STYLE_COLOUR('MAS366_driver',#65760);
#65749=COLOUR_RGB('Steel - Satin',0.627450980392157,0.627450980392157,0.627450980392157);
#65750=COLOUR_RGB('MAS366_axle',0.619607843137255,0.603921568627451,0.572549019607843);
#65751=COLOUR_RGB('MAS366_cage',0.376470588235294,0.364705882352941,0.345098039215686);
#65752=COLOUR_RGB('MAS366_planet',0.690196078431373,0.682352941176471,0.658823529411765);
#65753=COLOUR_RGB('MAS366_pin',0.823529411764706,0.835294117647059,0.854901960784314);
#65754=COLOUR_RGB('MAS366_pawl',0.713725490196078,0.72156862745098,0.737254901960784);
#65755=COLOUR_RGB('MAS366_pawlpin',0.831372549019608,0.843137254901961,
0.862745098039216);
#65756=COLOUR_RGB('MAS366_ringspring',0.807843137254902,0.819607843137255,
0.83921568627451);
#65757=COLOUR_RGB('MAS366_clutch',0.588235294117647,0.576470588235294,0.549019607843137);
#65758=COLOUR_RGB('MAS366_key',0.807843137254902,0.819607843137255,0.83921568627451);
#65759=COLOUR_RGB('MAS366_spring',0.83921568627451,0.850980392156863,0.870588235294118);
#65760=COLOUR_RGB('MAS366_driver',0.709803921568627,0.588235294117647,0.36078431372549);
#65761=COLOUR_RGB('Dark Blue',0.08,0.2,0.34);
#65762=FILL_AREA_STYLE_COLOUR('',#65761);
#65763=FILL_AREA_STYLE('',(#65762));
#65764=SURFACE_STYLE_FILL_AREA(#65763);
#65765=SURFACE_SIDE_STYLE('',(#65764));
#65766=SURFACE_STYLE_USAGE(.BOTH.,#65765);
#65767=PRESENTATION_STYLE_ASSIGNMENT((#65766));
#65768=COLOUR_RGB('Light Blue',0.38,0.62,0.78);
#65769=FILL_AREA_STYLE_COLOUR('',#65768);
#65770=FILL_AREA_STYLE('',(#65769));
#65771=SURFACE_STYLE_FILL_AREA(#65770);
#65772=SURFACE_SIDE_STYLE('',(#65771));
#65773=SURFACE_STYLE_USAGE(.BOTH.,#65772);
#65774=PRESENTATION_STYLE_ASSIGNMENT((#65773));
#65775=COLOUR_RGB('Sky Blue',0.24,0.69,0.87);
#65776=FILL_AREA_STYLE_COLOUR('',#65775);
#65777=FILL_AREA_STYLE('',(#65776));
#65778=SURFACE_STYLE_FILL_AREA(#65777);
#65779=SURFACE_SIDE_STYLE('',(#65778));
#65780=SURFACE_STYLE_USAGE(.BOTH.,#65779);
#65781=PRESENTATION_STYLE_ASSIGNMENT((#65780));
#65782=COLOUR_RGB('Grey',0.48,0.52,0.57);
#65783=FILL_AREA_STYLE_COLOUR('',#65782);
#65784=FILL_AREA_STYLE('',(#65783));
#65785=SURFACE_STYLE_FILL_AREA(#65784);
#65786=SURFACE_SIDE_STYLE('',(#65785));
#65787=SURFACE_STYLE_USAGE(.BOTH.,#65786);
#65788=PRESENTATION_STYLE_ASSIGNMENT((#65787));
#65789=COLOUR_RGB('Black',0.12,0.14,0.17);
#65790=FILL_AREA_STYLE_COLOUR('',#65789);
#65791=FILL_AREA_STYLE('',(#65790));
#65792=SURFACE_STYLE_FILL_AREA(#65791);
#65793=SURFACE_SIDE_STYLE('',(#65792));
#65794=SURFACE_STYLE_USAGE(.BOTH.,#65793);
#65795=PRESENTATION_STYLE_ASSIGNMENT((#65794));
#65796=COLOUR_RGB('Off White',0.89,0.88,0.83);
#65797=FILL_AREA_STYLE_COLOUR('',#65796);
#65798=FILL_AREA_STYLE('',(#65797));
#65799=SURFACE_STYLE_FILL_AREA(#65798);
#65800=SURFACE_SIDE_STYLE('',(#65799));
#65801=SURFACE_STYLE_USAGE(.BOTH.,#65800);
#65802=PRESENTATION_STYLE_ASSIGNMENT((#65801));
ENDSEC;
END-ISO-10303-21;
